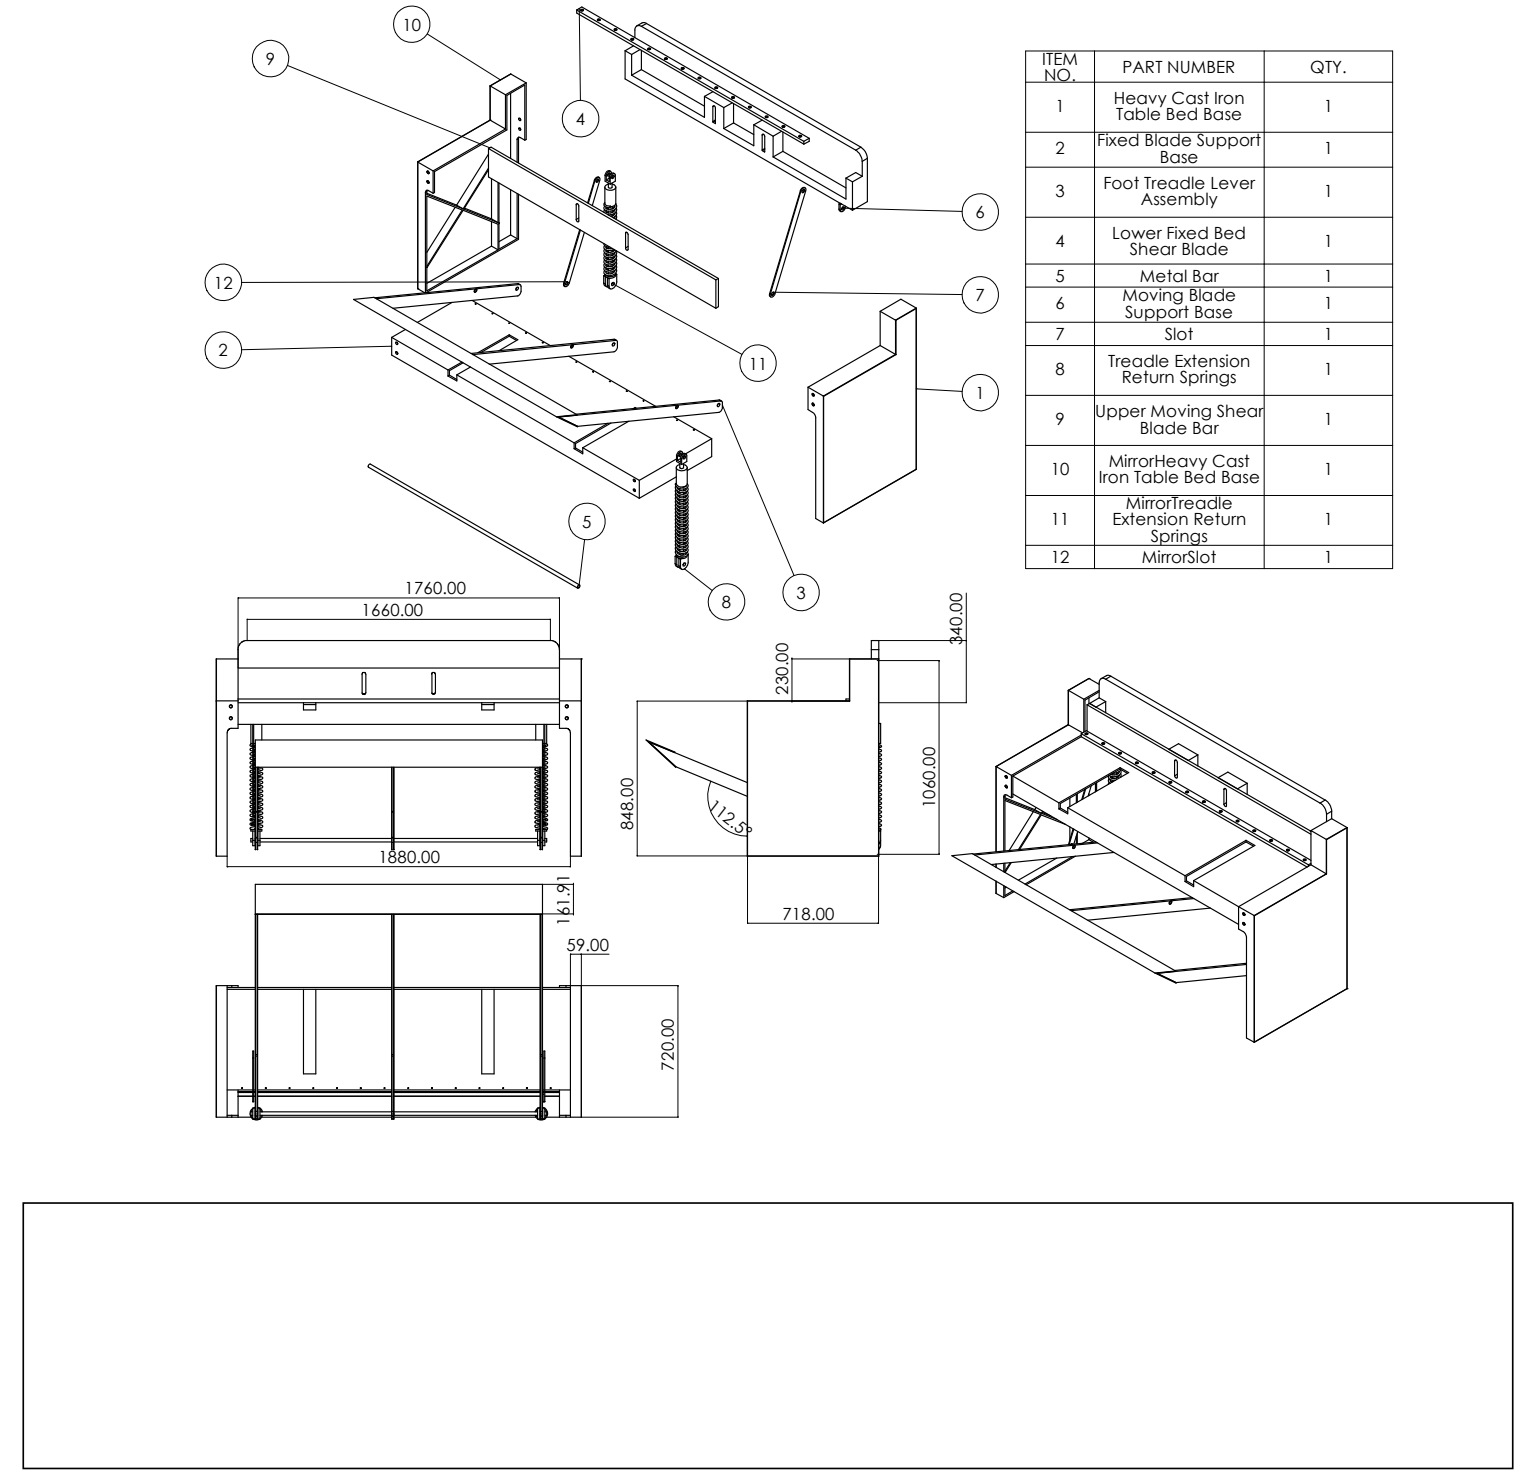
ISO-10303-21;
HEADER;
FILE_DESCRIPTION (('STEP AP214'),
    '1' );
FILE_NAME ('MAS-320',
    '2026-10-21T17:07:05',
    ( '' ),
    ( '' ),
    'SwSTEP 2.0',
    'SolidWorks 2025',
    '' );
FILE_SCHEMA (( 'AUTOMOTIVE_DESIGN' ));
ENDSEC;

DATA;
#1 = CARTESIAN_POINT ( 'NONE',  ( 745.1769319972822814, -41.80559628986934229, -346.2694204179732083 ) ) ;
#2 = CARTESIAN_POINT ( 'NONE',  ( 764.0069404352550464, -207.0783235625960685, -359.2566176426627180 ) ) ;
#3 = CARTESIAN_POINT ( 'NONE',  ( 745.1769319972822814, -209.8055962898687881, 346.2694204179732083 ) ) ;
#4 = CARTESIAN_POINT ( 'NONE',  ( 797.8594530101009923, -13.54369356751140963, 322.1405469898982119 ) ) ;
#5 =( BOUNDED_CURVE ( )  B_SPLINE_CURVE ( 2, ( #42977, #27813, #34735, #31272, #11342, #6564, #43210, #24332, #11582, #18730, #45142, #13500, #10036, #41910, #10254, #1170, #25872, #11803, #43435, #23072, #9239, #22634, #8789, #2069, #32818, #29794, #39983, #36732, #8332, #5090, #40437, #18964, #26092, #37170, #33058, #30023, #43655, #1395, #5529, #15499, #33484, #44108, #12472, #23310, #5303, #15279, #37412, #22395, #5769, #44335, #36499, #29579, #1830, #4863, #29365, #26551, #22857, #19625, #33720, #12025, #40649, #40206, #8568, #36950, #19181, #16161, #33266, #30243, #12690, #26770, #1612, #19399, #15711, #15939, #43874, #12253, #26333, #9002, #40875, #10150, #30713, #2768, #31156, #19857, #37866, #12929, #13166, #27016, #27245, #16861, #37632, #16626, #2991, #23530, #9913, #34150, #5983, #34634, #20075, #27462, #30941, #23985, #24225, #41115, #45034, #20540, #41337, #2520, #17078, #6462, #13390, #45254, #13613, #9467, #44568, #44809, #9687, #23751, #6212, #20305, #34397, #38106, #41560, #41801, #2288, #16387, #38333, #27697, #6679, #33937, #30466, #15422, #12398, #1747, #26925, #19779, #41028, #9388, #44026, #23223, #23455, #33195, #36878, #12841, #8717, #20002, #22552, #9151, #5912, #29712, #34079, #37554, #2216, #29500, #43572, #5445, #30169, #11940, #22783, #8482, #26008, #43789, #19319, #16085, #5228, #40579, #33403, #33863, #12618, #26252, #15629, #5690, #12171, #44260, #19540, #40117, #26477, #26696, #33635, #15854, #29942, #1532, #16310, #37328, #1988, #30392, #44485, #19108, #36657, #40365, #8925, #5017, #22995, #37090, #40793, #41950, #41259, #37788, #45414, #7068, #13775, #27854, #23906, #13537, #9837, #2443, #45176, #34552, #13999, #6822, #28067, #42163, #31078, #10291, #10514, #21149, #17466, #24367, #41720, #10074, #9615, #38471, #38706, #16781, #16545, #24589, #34998, #30630, #44725, #38254, #17221, #13088, #41483, #23677, #27171, #38027, #6137, #20227, #6382, #27611, #34315, #20901, #2684, #20678, #30861, #44955, #13312, #27388, #20463, #2911, #17001, #3131, #24145, #6600, #3375, #34768, #31548, #45650, #31306, #14912, #129, #7303, #25284, #14218, #22057, #14460, #39636, #15137, #18602, #39862, #7748, #17698, #21827, #3611, #28288, #42386, #10757, #25523, #11673, #10994, #31759, #24833, #4055, #29230, #32687, #35920, #38953, #25750, #43305, #11439, #28993, #21380, #32231, #8203, #35454, #4291, #35231, #3826, #25062, #1034, #28537, #17915, #39175, #7525, #810, #31985, #356, #42632, #21599, #35679, #18156, #591, #18382, #14693, #42848, #28769, #11215, #39397, #32462, #43074, #7991, #36147, #4509, #5627, #30330, #11887, #1692, #26638, #29661, #33579, #33143, #44424, #37267, #30115, #12115, #40065, #43737, #15796, #12561, #1930, #8664, #32923, #15579, #43521, #26859, #26196, #40311, #12778, #5175, #33808, #29886, #25959, #18831, #43973, #19052, #19721, #15367, #37036, #8426, #16253, #26424, #4729, #40734, #1268, #36823, #2162, #40968, #40524, #29448, #22271, #36367, #44203, #16033, #22495, #19261, #36606, #4960, #12348, #1479, #22726, #33350, #8875, #22939, #9090, #5388, #19482, #23158, #37501, #27335, #5861, #31026, #30804, #17168, #10234, #2854, #17407, #16481, #41428, #34247, #9779, #27554, #3076, #2380, #44662, #6543, #13939, #20623, #16947, #41658, #16720, #19950, #45124, #44897, #3310, #24083, #24313, #13482, #10013, #38197, #34717, #30561, #31253, #45591, #23620, #28014, #34943, #41890, #23399, #34025, #45354, #13715, #31489, #2620, #13023, #9330, #13257, #27113, #41203, #23846, #34494, #9560, #27793, #37729, #38418, #6081, #20168, #37958, #6317, #20845, #20399, #6769, #42797, #3555, #38648, #35867, #32175, #763, #32414, #42108, #21772, #7006, #14163, #538, #21093, #28940, #21320, #14864, #22007, #25464, #976, #14642, #24535, #28716, #10458, #35179, #17640, #31704, #43017, #18551, #17859, #71, #11382, #28234, #39119, #42329, #298, #10695, #31926, #3994, #24778, #35396, #39583, #38896, #39339, #7250, #3769, #7940, #14398, #11157, #25227, #28478, #32633, #42579, #18092, #18334, #10937, #25009, #36097, #4244, #7692, #4462, #15079, #7468, #21540, #35622, #32859, #18773, #4675, #11839, #29399, #22894, #25910, #9040, #11621, #25699, #5575, #40474, #4903, #40253, #36545, #29166, #26138, #15533, #40685, #33527, #23109, #37211, #12064, #36986, #19667, #2112, #19002, #39810, #40020, #29836, #36314, #8157, #5340, #19215, #1875, #19434, #43250, #8826, #22220, #22440, #1209, #33760, #33094, #1431, #15317, #8610, #12511, #43471, #15748, #8371, #43917, #29614, #43692, #22675, #36772, #15983, #5127, #33302, #12297, #30066, #26372, #44147, #26587, #45296, #34441, #12730, #41840, #38146, #9957, #23352, #13210, #13655, #31199, #41380, #9282, #23573, #30281, #41600, #13431, #38369, #37454, #23794, #6497, #6027, #33978, #20575, #37905, #37678, #24027, #17117, #9729, #24261, #5813, #2564, #41158, #16669, #2806, #16429, #34671, #12973, #10185, #44374, #26809, #6716, #27736, #20119, #40915, #6259, #34194, #20792, #30978, #34888, #20346, #16897, #16201, #2329, #45076, #19901, #30509, #30755, #44612, #9509, #27063, #44848, #27287, #39526, #31651, #27962, #45535, #21263, #38836, #42277, #17805, #32114, #25404, #10880, #31872, #24948, #19, #7189, #3939, #35342, #28417, #10637, #21712, #7881, #38590, #42515, #7635, #24718, #14584, #14111, #3251, #21957, #42058, #17343, #14805, #13888, #28184, #18033, #10406, #24483, #42736, #39063, #35809, #39280, #3718, #3493, #6945, #21028, #7411, #35116, #4185, #243, #18280, #28879, #32354, #31429, #21486, #17581, #35563, #14339, #479, #28658, #11100, #708, #25170, #42959, #11327, #5288, #36043, #33043, #43193, #39969, #11562, #25859, #43639, #22167, #29348, #40421, #36257, #33249, #1154, #4614, #26315, #18711, #4406, #1595, #15693, #12456, #29109, #12008, #12236, #8314, #8106, #8773, #29777, #22614, #22841, #36934, #39758, #15021, #32800, #15259, #25644, #43421, #8550, #11788, #43853, #22379, #15920, #18496, #32575, #26535, #19381, #36483, #1381, #4848, #918, #15484, #18947, #30004, #33466, #44091, #40633, #29564, #36714, #8986, #26072, #40185, #5074, #19165, #27679, #30228, #16845, #13596, #37396, #41784, #2973, #9895, #37153, #5512, #13149, #37848, #45236, #16371, #5968, #30698, #5750, #26999, #23738, #12911, #2504, #30448, #41543, #23054, #41322, #17062, #23968, #19608, #33701, #27230, #6197, #2051, #44551, #16145, #44794, #19839, #41095, #20288, #9450, #16610, #23514, #38090, #44319, #9672, #12674, #26754, #40858, #9220, #34618, #23295, #33921, #34381, #2272, #37615, #20058, #2750, #13373, #30924, #34135, #45020, #27446, #6445, #20524, #31139, #42687, #35062, #14529, #35753, #39233, #14755, #28354, #38317, #42458, #24207, #3194, #24897, #31372, #4132, #14285, #45710, #31822, #25119, #10134, #7134, #17283, #14062, #45480, #28134, #17758, #42010, #3436, #28605, #10354, #7362, #7586, #35293 ),
 .UNSPECIFIED., .F., .T. ) 
 B_SPLINE_CURVE_WITH_KNOTS ( ( 3, 2, 2, 2, 2, 2, 2, 2, 2, 2, 2, 2, 2, 2, 2, 2, 2, 2, 2, 2, 2, 2, 2, 2, 2, 2, 2, 2, 2, 2, 2, 2, 2, 2, 2, 2, 2, 2, 2, 2, 2, 2, 2, 2, 2, 2, 2, 2, 2, 2, 2, 2, 2, 2, 2, 2, 2, 2, 2, 2, 2, 2, 2, 2, 2, 2, 2, 2, 2, 2, 2, 2, 2, 2, 2, 2, 2, 2, 2, 2, 2, 2, 2, 2, 2, 2, 2, 2, 2, 2, 2, 2, 2, 2, 2, 2, 2, 2, 2, 2, 2, 2, 2, 2, 2, 2, 2, 2, 2, 2, 2, 2, 2, 2, 2, 2, 2, 2, 2, 2, 2, 2, 2, 2, 2, 2, 2, 2, 2, 2, 2, 2, 2, 2, 2, 2, 2, 2, 2, 2, 2, 2, 2, 2, 2, 2, 2, 2, 2, 2, 2, 2, 2, 2, 2, 2, 2, 2, 2, 2, 2, 2, 2, 2, 2, 2, 2, 2, 2, 2, 2, 2, 2, 2, 2, 2, 2, 2, 2, 2, 2, 2, 2, 2, 2, 2, 2, 2, 2, 2, 2, 2, 2, 2, 2, 2, 2, 2, 2, 2, 2, 2, 2, 2, 2, 2, 2, 2, 2, 2, 2, 2, 2, 2, 2, 2, 2, 2, 2, 2, 2, 2, 2, 2, 2, 2, 2, 2, 2, 2, 2, 2, 2, 2, 2, 2, 2, 2, 2, 2, 2, 2, 2, 2, 2, 2, 2, 2, 2, 2, 2, 2, 2, 2, 2, 2, 2, 2, 2, 2, 2, 2, 2, 2, 2, 2, 2, 2, 2, 2, 2, 2, 2, 2, 2, 2, 2, 2, 2, 2, 2, 2, 2, 2, 2, 2, 2, 2, 2, 2, 2, 2, 2, 2, 2, 2, 2, 2, 2, 2, 2, 2, 2, 2, 2, 2, 2, 2, 2, 2, 2, 2, 2, 2, 2, 2, 2, 2, 2, 2, 2, 2, 2, 2, 2, 2, 2, 2, 2, 2, 2, 2, 2, 2, 2, 2, 2, 2, 2, 2, 2, 2, 2, 2, 2, 2, 2, 2, 2, 2, 2, 2, 2, 2, 2, 2, 2, 2, 2, 2, 2, 2, 2, 2, 2, 2, 2, 2, 2, 2, 2, 2, 2, 2, 2, 2, 2, 2, 2, 2, 2, 2, 2, 2, 2, 2, 2, 2, 2, 2, 2, 2, 2, 2, 2, 2, 2, 2, 2, 2, 2, 2, 2, 2, 2, 2, 2, 2, 2, 2, 2, 2, 2, 2, 2, 2, 2, 2, 2, 2, 2, 2, 2, 2, 2, 2, 2, 2, 2, 2, 2, 3 ),
 ( 0.000000000000000000, 0.002272727272727272617, 0.004545454545454545234, 0.006818181818181817851, 0.009090909090909090468, 0.01136363636363636395, 0.01363636363636363570, 0.01590909090909090745, 0.01818181818181818094, 0.02045454545454545442, 0.02272727272727272790, 0.02500000000000000139, 0.02727272727272727140, 0.02954545454545454489, 0.03181818181818181490, 0.03409090909090908839, 0.03636363636363636187, 0.03863636363636363535, 0.04090909090909090884, 0.04318181818181818232, 0.04545454545454545581, 0.04772727272727272929, 0.05000000000000000278, 0.05227272727272727626, 0.05454545454545454281, 0.05681818181818181629, 0.05909090909090908977, 0.06136363636363636326, 0.06363636363636362980, 0.06590909090909090329, 0.06818181818181817677, 0.07045454545454545026, 0.07272727272727272374, 0.07499999999999999722, 0.07727272727272727071, 0.07954545454545454419, 0.08181818181818181768, 0.08409090909090909116, 0.08636363636363636465, 0.08863636363636363813, 0.09090909090909091161, 0.09318181818181818510, 0.09545454545454545858, 0.09772727272727273207, 0.1000000000000000056, 0.1022727272727272790, 0.1045454545454545525, 0.1068181818181818121, 0.1090909090909090856, 0.1113636363636363591, 0.1136363636363636326, 0.1159090909090909061, 0.1181818181818181795, 0.1204545454545454530, 0.1227272727272727265, 0.1250000000000000000, 0.1272727272727272596, 0.1295454545454545470, 0.1318181818181818066, 0.1340909090909090939, 0.1363636363636363535, 0.1386363636363636409, 0.1409090909090909005, 0.1431818181818181879, 0.1454545454545454475, 0.1477272727272727348, 0.1499999999999999944, 0.1522727272727272818, 0.1545454545454545414, 0.1568181818181818288, 0.1590909090909090884, 0.1613636363636363757, 0.1636363636363636354, 0.1659090909090909227, 0.1681818181818181823, 0.1704545454545454419, 0.1727272727272727293, 0.1749999999999999889, 0.1772727272727272763, 0.1795454545454545359, 0.1818181818181818232, 0.1840909090909090828, 0.1863636363636363702, 0.1886363636363636298, 0.1909090909090909172, 0.1931818181818181768, 0.1954545454545454641, 0.1977272727272727237, 0.2000000000000000111, 0.2022727272727272707, 0.2045454545454545581, 0.2068181818181818177, 0.2090909090909091050, 0.2113636363636363646, 0.2136363636363636243, 0.2159090909090909116, 0.2181818181818181712, 0.2204545454545454586, 0.2227272727272727182, 0.2250000000000000056, 0.2272727272727272652, 0.2295454545454545525, 0.2318181818181818121, 0.2340909090909090995, 0.2363636363636363591, 0.2386363636363636465, 0.2409090909090909061, 0.2431818181818181934, 0.2454545454545454530, 0.2477272727272727404, 0.2500000000000000000, 0.2522727272727272596, 0.2545454545454545192, 0.2568181818181818343, 0.2590909090909090939, 0.2613636363636363535, 0.2636363636363636131, 0.2659090909090909283, 0.2681818181818181879, 0.2704545454545454475, 0.2727272727272727071, 0.2750000000000000222, 0.2772727272727272818, 0.2795454545454545414, 0.2818181818181818010, 0.2840909090909091161, 0.2863636363636363757, 0.2886363636363636354, 0.2909090909090908950, 0.2931818181818181546, 0.2954545454545454697, 0.2977272727272727293, 0.2999999999999999889, 0.3022727272727272485, 0.3045454545454545636, 0.3068181818181818232, 0.3090909090909090828, 0.3113636363636363424, 0.3136363636363636576, 0.3159090909090909172, 0.3181818181818181768, 0.3204545454545454364, 0.3227272727272727515, 0.3250000000000000111, 0.3272727272727272707, 0.3295454545454545303, 0.3318181818181818454, 0.3340909090909090495, 0.3363636363636363646, 0.3386363636363636243, 0.3409090909090908839, 0.3431818181818181990, 0.3454545454545454586, 0.3477272727272727182, 0.3499999999999999778, 0.3522727272727272929, 0.3545454545454545525, 0.3568181818181818121, 0.3590909090909090717, 0.3613636363636363869, 0.3636363636363636465, 0.3659090909090909061, 0.3681818181818181657, 0.3704545454545454808, 0.3727272727272727404, 0.3750000000000000000, 0.3772727272727272596, 0.3795454545454545192, 0.3818181818181818343, 0.3840909090909090939, 0.3863636363636363535, 0.3886363636363636131, 0.3909090909090909283, 0.3931818181818181879, 0.3954545454545454475, 0.3977272727272727071, 0.4000000000000000222, 0.4022727272727272818, 0.4045454545454545414, 0.4068181818181818010, 0.4090909090909091161, 0.4113636363636363757, 0.4136363636363636354, 0.4159090909090908950, 0.4181818181818182101, 0.4204545454545454697, 0.4227272727272727293, 0.4249999999999999889, 0.4272727272727272485, 0.4295454545454545636, 0.4318181818181818232, 0.4340909090909090828, 0.4363636363636363424, 0.4386363636363636576, 0.4409090909090909172, 0.4431818181818181768, 0.4454545454545454364, 0.4477272727272727515, 0.4500000000000000111, 0.4522727272727272707, 0.4545454545454545303, 0.4568181818181818454, 0.4590909090909091050, 0.4613636363636363646, 0.4636363636363636243, 0.4659090909090908839, 0.4681818181818181990, 0.4704545454545454586, 0.4727272727272727182, 0.4749999999999999778, 0.4772727272727272929, 0.4795454545454545525, 0.4818181818181818121, 0.4840909090909090717, 0.4863636363636363869, 0.4886363636363636465, 0.4909090909090909061, 0.4931818181818181657, 0.4954545454545454808, 0.4977272727272727959, 0.5000000000000000000, 0.5022727272727273151, 0.5045454545454545192, 0.5068181818181818343, 0.5090909090909090384, 0.5113636363636363535, 0.5136363636363636687, 0.5159090909090908728, 0.5181818181818181879, 0.5204545454545455030, 0.5227272727272727071, 0.5250000000000000222, 0.5272727272727272263, 0.5295454545454545414, 0.5318181818181818565, 0.5340909090909090606, 0.5363636363636363757, 0.5386363636363636909, 0.5409090909090908950, 0.5431818181818182101, 0.5454545454545454142, 0.5477272727272727293, 0.5500000000000000444, 0.5522727272727272485, 0.5545454545454545636, 0.5568181818181817677, 0.5590909090909090828, 0.5613636363636363980, 0.5636363636363636020, 0.5659090909090909172, 0.5681818181818182323, 0.5704545454545454364, 0.5727272727272727515, 0.5749999999999999556, 0.5772727272727272707, 0.5795454545454545858, 0.5818181818181817899, 0.5840909090909089940, 0.5863636363636363091, 0.5886363636363636243, 0.5909090909090909394, 0.5931818181818181435, 0.5954545454545454586, 0.5977272727272727737, 0.5999999999999999778, 0.6022727272727272929, 0.6045454545454544970, 0.6068181818181818121, 0.6090909090909091272, 0.6113636363636363313, 0.6136363636363636465, 0.6159090909090909616, 0.6181818181818181657, 0.6204545454545454808, 0.6227272727272726849, 0.6250000000000000000, 0.6272727272727273151, 0.6295454545454545192, 0.6318181818181818343, 0.6340909090909090384, 0.6363636363636363535, 0.6386363636363636687, 0.6409090909090908728, 0.6431818181818181879, 0.6454545454545455030, 0.6477272727272727071, 0.6500000000000000222, 0.6522727272727272263, 0.6545454545454545414, 0.6568181818181818565, 0.6590909090909090606, 0.6613636363636363757, 0.6636363636363636909, 0.6659090909090908950, 0.6681818181818180991, 0.6704545454545454142, 0.6727272727272727293, 0.6750000000000000444, 0.6772727272727272485, 0.6795454545454545636, 0.6818181818181817677, 0.6840909090909090828, 0.6863636363636363980, 0.6886363636363636020, 0.6909090909090909172, 0.6931818181818182323, 0.6954545454545454364, 0.6977272727272727515, 0.6999999999999999556, 0.7022727272727272707, 0.7045454545454545858, 0.7068181818181817899, 0.7090909090909091050, 0.7113636363636363091, 0.7136363636363636243, 0.7159090909090909394, 0.7181818181818181435, 0.7204545454545454586, 0.7227272727272727737, 0.7249999999999999778, 0.7272727272727272929, 0.7295454545454544970, 0.7318181818181818121, 0.7340909090909091272, 0.7363636363636363313, 0.7386363636363636465, 0.7409090909090909616, 0.7431818181818181657, 0.7454545454545454808, 0.7477272727272726849, 0.7500000000000000000, 0.7522727272727273151, 0.7545454545454545192, 0.7568181818181818343, 0.7590909090909090384, 0.7613636363636363535, 0.7636363636363636687, 0.7659090909090908728, 0.7681818181818181879, 0.7704545454545455030, 0.7727272727272727071, 0.7750000000000000222, 0.7772727272727272263, 0.7795454545454545414, 0.7818181818181818565, 0.7840909090909090606, 0.7863636363636363757, 0.7886363636363636909, 0.7909090909090908950, 0.7931818181818182101, 0.7954545454545454142, 0.7977272727272727293, 0.8000000000000000444, 0.8022727272727272485, 0.8045454545454545636, 0.8068181818181817677, 0.8090909090909090828, 0.8113636363636363980, 0.8136363636363636020, 0.8159090909090909172, 0.8181818181818182323, 0.8204545454545454364, 0.8227272727272727515, 0.8249999999999999556, 0.8272727272727272707, 0.8295454545454545858, 0.8318181818181817899, 0.8340909090909091050, 0.8363636363636364202, 0.8386363636363636243, 0.8409090909090909394, 0.8431818181818181435, 0.8454545454545454586, 0.8477272727272727737, 0.8499999999999999778, 0.8522727272727272929, 0.8545454545454544970, 0.8568181818181818121, 0.8590909090909091272, 0.8613636363636363313, 0.8636363636363636465, 0.8659090909090909616, 0.8681818181818181657, 0.8704545454545454808, 0.8727272727272726849, 0.8750000000000000000, 0.8772727272727273151, 0.8795454545454545192, 0.8818181818181818343, 0.8840909090909090384, 0.8863636363636363535, 0.8886363636363636687, 0.8909090909090908728, 0.8931818181818181879, 0.8954545454545455030, 0.8977272727272727071, 0.9000000000000000222, 0.9022727272727272263, 0.9045454545454545414, 0.9068181818181818565, 0.9090909090909090606, 0.9113636363636363757, 0.9136363636363636909, 0.9159090909090908950, 0.9181818181818182101, 0.9204545454545453032, 0.9227272727272727293, 0.9250000000000000444, 0.9272727272727272485, 0.9295454545454545636, 0.9318181818181817677, 0.9340909090909090828, 0.9363636363636363980, 0.9386363636363636020, 0.9409090909090909172, 0.9431818181818182323, 0.9454545454545454364, 0.9477272727272727515, 0.9499999999999999556, 0.9522727272727272707, 0.9545454545454545858, 0.9568181818181817899, 0.9590909090909091050, 0.9613636363636363091, 0.9636363636363636243, 0.9659090909090909394, 0.9681818181818181435, 0.9704545454545454586, 0.9727272727272727737, 0.9749999999999999778, 0.9772727272727272929, 0.9779695260516495514 ),
 .UNSPECIFIED. ) 
 CURVE ( )  GEOMETRIC_REPRESENTATION_ITEM ( )  RATIONAL_B_SPLINE_CURVE ( ( 1.000000000000000000, 0.9898214418809326842, 1.000000000000000000, 0.9898214418809326842, 1.000000000000000000, 0.9898214418809326842, 1.000000000000000000, 0.9898214418809326842, 1.000000000000000000, 0.9898214418809326842, 1.000000000000000000, 0.9898214418809326842, 1.000000000000000000, 0.9898214418809326842, 1.000000000000000000, 0.9898214418809326842, 1.000000000000000000, 0.9898214418809326842, 1.000000000000000000, 0.9898214418809326842, 1.000000000000000000, 0.9898214418809326842, 1.000000000000000000, 0.9898214418809326842, 1.000000000000000000, 0.9898214418809326842, 1.000000000000000000, 0.9898214418809326842, 1.000000000000000000, 0.9898214418809326842, 1.000000000000000000, 0.9898214418809326842, 1.000000000000000000, 0.9898214418809326842, 1.000000000000000000, 0.9898214418809326842, 1.000000000000000000, 0.9898214418809326842, 1.000000000000000000, 0.9898214418809326842, 1.000000000000000000, 0.9898214418809326842, 1.000000000000000000, 0.9898214418809326842, 1.000000000000000000, 0.9898214418809326842, 1.000000000000000000, 0.9898214418809326842, 1.000000000000000000, 0.9898214418809326842, 1.000000000000000000, 0.9898214418809326842, 1.000000000000000000, 0.9898214418809326842, 1.000000000000000000, 0.9898214418809326842, 1.000000000000000000, 0.9898214418809326842, 1.000000000000000000, 0.9898214418809326842, 1.000000000000000000, 0.9898214418809326842, 1.000000000000000000, 0.9898214418809326842, 1.000000000000000000, 0.9898214418809326842, 1.000000000000000000, 0.9898214418809326842, 1.000000000000000000, 0.9898214418809326842, 1.000000000000000000, 0.9898214418809326842, 1.000000000000000000, 0.9898214418809326842, 1.000000000000000000, 0.9898214418809326842, 1.000000000000000000, 0.9898214418809326842, 1.000000000000000000, 0.9898214418809326842, 1.000000000000000000, 0.9898214418809326842, 1.000000000000000000, 0.9898214418809326842, 1.000000000000000000, 0.9898214418809326842, 1.000000000000000000, 0.9898214418809326842, 1.000000000000000000, 0.9898214418809326842, 1.000000000000000000, 0.9898214418809326842, 1.000000000000000000, 0.9898214418809326842, 1.000000000000000000, 0.9898214418809326842, 1.000000000000000000, 0.9898214418809326842, 1.000000000000000000, 0.9898214418809326842, 1.000000000000000000, 0.9898214418809326842, 1.000000000000000000, 0.9898214418809326842, 1.000000000000000000, 0.9898214418809326842, 1.000000000000000000, 0.9898214418809326842, 1.000000000000000000, 0.9898214418809326842, 1.000000000000000000, 0.9898214418809326842, 1.000000000000000000, 0.9898214418809326842, 1.000000000000000000, 0.9898214418809326842, 1.000000000000000000, 0.9898214418809326842, 1.000000000000000000, 0.9898214418809326842, 1.000000000000000000, 0.9898214418809326842, 1.000000000000000000, 0.9898214418809326842, 1.000000000000000000, 0.9898214418809326842, 1.000000000000000000, 0.9898214418809326842, 1.000000000000000000, 0.9898214418809326842, 1.000000000000000000, 0.9898214418809326842, 1.000000000000000000, 0.9898214418809326842, 1.000000000000000000, 0.9898214418809326842, 1.000000000000000000, 0.9898214418809326842, 1.000000000000000000, 0.9898214418809326842, 1.000000000000000000, 0.9898214418809326842, 1.000000000000000000, 0.9898214418809326842, 1.000000000000000000, 0.9898214418809326842, 1.000000000000000000, 0.9898214418809326842, 1.000000000000000000, 0.9898214418809326842, 1.000000000000000000, 0.9898214418809326842, 1.000000000000000000, 0.9898214418809326842, 1.000000000000000000, 0.9898214418809326842, 1.000000000000000000, 0.9898214418809326842, 1.000000000000000000, 0.9898214418809326842, 1.000000000000000000, 0.9898214418809326842, 1.000000000000000000, 0.9898214418809326842, 1.000000000000000000, 0.9898214418809326842, 1.000000000000000000, 0.9898214418809326842, 1.000000000000000000, 0.9898214418809326842, 1.000000000000000000, 0.9898214418809326842, 1.000000000000000000, 0.9898214418809326842, 1.000000000000000000, 0.9898214418809326842, 1.000000000000000000, 0.9898214418809326842, 1.000000000000000000, 0.9898214418809326842, 1.000000000000000000, 0.9898214418809326842, 1.000000000000000000, 0.9898214418809326842, 1.000000000000000000, 0.9898214418809326842, 1.000000000000000000, 0.9898214418809326842, 1.000000000000000000, 0.9898214418809326842, 1.000000000000000000, 0.9898214418809326842, 1.000000000000000000, 0.9898214418809326842, 1.000000000000000000, 0.9898214418809326842, 1.000000000000000000, 0.9898214418809326842, 1.000000000000000000, 0.9898214418809326842, 1.000000000000000000, 0.9898214418809326842, 1.000000000000000000, 0.9898214418809326842, 1.000000000000000000, 0.9898214418809326842, 1.000000000000000000, 0.9898214418809326842, 1.000000000000000000, 0.9898214418809326842, 1.000000000000000000, 0.9898214418809326842, 1.000000000000000000, 0.9898214418809326842, 1.000000000000000000, 0.9898214418809326842, 1.000000000000000000, 0.9898214418809326842, 1.000000000000000000, 0.9898214418809326842, 1.000000000000000000, 0.9898214418809326842, 1.000000000000000000, 0.9898214418809326842, 1.000000000000000000, 0.9898214418809326842, 1.000000000000000000, 0.9898214418809326842, 1.000000000000000000, 0.9898214418809326842, 1.000000000000000000, 0.9898214418809326842, 1.000000000000000000, 0.9898214418809326842, 1.000000000000000000, 0.9898214418809326842, 1.000000000000000000, 0.9898214418809326842, 1.000000000000000000, 0.9898214418809326842, 1.000000000000000000, 0.9898214418809326842, 1.000000000000000000, 0.9898214418809326842, 1.000000000000000000, 0.9898214418809326842, 1.000000000000000000, 0.9898214418809326842, 1.000000000000000000, 0.9898214418809326842, 1.000000000000000000, 0.9898214418809326842, 1.000000000000000000, 0.9898214418809326842, 1.000000000000000000, 0.9898214418809326842, 1.000000000000000000, 0.9898214418809326842, 1.000000000000000000, 0.9898214418809326842, 1.000000000000000000, 0.9898214418809326842, 1.000000000000000000, 0.9898214418809326842, 1.000000000000000000, 0.9898214418809326842, 1.000000000000000000, 0.9898214418809326842, 1.000000000000000000, 0.9898214418809326842, 1.000000000000000000, 0.9898214418809326842, 1.000000000000000000, 0.9898214418809326842, 1.000000000000000000, 0.9898214418809326842, 1.000000000000000000, 0.9898214418809326842, 1.000000000000000000, 0.9898214418809326842, 1.000000000000000000, 0.9898214418809326842, 1.000000000000000000, 0.9898214418809326842, 1.000000000000000000, 0.9898214418809326842, 1.000000000000000000, 0.9898214418809326842, 1.000000000000000000, 0.9898214418809326842, 1.000000000000000000, 0.9898214418809326842, 1.000000000000000000, 0.9898214418809326842, 1.000000000000000000, 0.9898214418809326842, 1.000000000000000000, 0.9898214418809326842, 1.000000000000000000, 0.9898214418809326842, 1.000000000000000000, 0.9898214418809326842, 1.000000000000000000, 0.9898214418809326842, 1.000000000000000000, 0.9898214418809326842, 1.000000000000000000, 0.9898214418809326842, 1.000000000000000000, 0.9898214418809326842, 1.000000000000000000, 0.9898214418809326842, 1.000000000000000000, 0.9898214418809326842, 1.000000000000000000, 0.9898214418809326842, 1.000000000000000000, 0.9898214418809326842, 1.000000000000000000, 0.9898214418809326842, 1.000000000000000000, 0.9898214418809326842, 1.000000000000000000, 0.9898214418809326842, 1.000000000000000000, 0.9898214418809326842, 1.000000000000000000, 0.9898214418809326842, 1.000000000000000000, 0.9898214418809326842, 1.000000000000000000, 0.9898214418809326842, 1.000000000000000000, 0.9898214418809326842, 1.000000000000000000, 0.9898214418809326842, 1.000000000000000000, 0.9898214418809326842, 1.000000000000000000, 0.9898214418809326842, 1.000000000000000000, 0.9898214418809326842, 1.000000000000000000, 0.9898214418809326842, 1.000000000000000000, 0.9898214418809326842, 1.000000000000000000, 0.9898214418809326842, 1.000000000000000000, 0.9898214418809326842, 1.000000000000000000, 0.9898214418809326842, 1.000000000000000000, 0.9898214418809326842, 1.000000000000000000, 0.9898214418809326842, 1.000000000000000000, 0.9898214418809326842, 1.000000000000000000, 0.9898214418809326842, 1.000000000000000000, 0.9898214418809326842, 1.000000000000000000, 0.9898214418809326842, 1.000000000000000000, 0.9898214418809326842, 1.000000000000000000, 0.9898214418809326842, 1.000000000000000000, 0.9898214418809326842, 1.000000000000000000, 0.9898214418809326842, 1.000000000000000000, 0.9898214418809326842, 1.000000000000000000, 0.9898214418809326842, 1.000000000000000000, 0.9898214418809326842, 1.000000000000000000, 0.9898214418809326842, 1.000000000000000000, 0.9898214418809326842, 1.000000000000000000, 0.9898214418809326842, 1.000000000000000000, 0.9898214418809326842, 1.000000000000000000, 0.9898214418809326842, 1.000000000000000000, 0.9898214418809326842, 1.000000000000000000, 0.9898214418809326842, 1.000000000000000000, 0.9898214418809326842, 1.000000000000000000, 0.9898214418809326842, 1.000000000000000000, 0.9898214418809326842, 1.000000000000000000, 0.9898214418809326842, 1.000000000000000000, 0.9898214418809326842, 1.000000000000000000, 0.9898214418809326842, 1.000000000000000000, 0.9898214418809326842, 1.000000000000000000, 0.9898214418809326842, 1.000000000000000000, 0.9898214418809326842, 1.000000000000000000, 0.9898214418809326842, 1.000000000000000000, 0.9898214418809326842, 1.000000000000000000, 0.9898214418809326842, 1.000000000000000000, 0.9898214418809326842, 1.000000000000000000, 0.9898214418809326842, 1.000000000000000000, 0.9898214418809326842, 1.000000000000000000, 0.9898214418809326842, 1.000000000000000000, 0.9898214418809326842, 1.000000000000000000, 0.9898214418809326842, 1.000000000000000000, 0.9898214418809326842, 1.000000000000000000, 0.9898214418809326842, 1.000000000000000000, 0.9898214418809326842, 1.000000000000000000, 0.9898214418809326842, 1.000000000000000000, 0.9898214418809326842, 1.000000000000000000, 0.9898214418809326842, 1.000000000000000000, 0.9898214418809326842, 1.000000000000000000, 0.9898214418809326842, 1.000000000000000000, 0.9898214418809326842, 1.000000000000000000, 0.9898214418809326842, 1.000000000000000000, 0.9898214418809326842, 1.000000000000000000, 0.9898214418809326842, 1.000000000000000000, 0.9898214418809326842, 1.000000000000000000, 0.9898214418809326842, 1.000000000000000000, 0.9898214418809326842, 1.000000000000000000, 0.9898214418809326842, 1.000000000000000000, 0.9898214418809326842, 1.000000000000000000, 0.9898214418809326842, 1.000000000000000000, 0.9898214418809326842, 1.000000000000000000, 0.9898214418809326842, 1.000000000000000000, 0.9898214418809326842, 1.000000000000000000, 0.9898214418809326842, 1.000000000000000000, 0.9898214418809326842, 1.000000000000000000, 0.9898214418809326842, 1.000000000000000000, 0.9898214418809326842, 1.000000000000000000, 0.9898214418809326842, 1.000000000000000000, 0.9898214418809326842, 1.000000000000000000, 0.9898214418809326842, 1.000000000000000000, 0.9898214418809326842, 1.000000000000000000, 0.9898214418809326842, 1.000000000000000000, 0.9898214418809326842, 1.000000000000000000, 0.9898214418809326842, 1.000000000000000000, 0.9898214418809326842, 1.000000000000000000, 0.9898214418809326842, 1.000000000000000000, 0.9898214418809326842, 1.000000000000000000, 0.9898214418809326842, 1.000000000000000000, 0.9898214418809326842, 1.000000000000000000, 0.9898214418809326842, 1.000000000000000000, 0.9898214418809326842, 1.000000000000000000, 0.9898214418809326842, 1.000000000000000000, 0.9898214418809326842, 1.000000000000000000, 0.9898214418809326842, 1.000000000000000000, 0.9898214418809326842, 1.000000000000000000, 0.9898214418809326842, 1.000000000000000000, 0.9898214418809326842, 1.000000000000000000, 0.9898214418809326842, 1.000000000000000000, 0.9898214418809326842, 1.000000000000000000, 0.9898214418809326842, 1.000000000000000000, 0.9898214418809326842, 1.000000000000000000, 0.9898214418809326842, 1.000000000000000000, 0.9898214418809326842, 1.000000000000000000, 0.9898214418809326842, 1.000000000000000000, 0.9898214418809326842, 1.000000000000000000, 0.9898214418809326842, 1.000000000000000000, 0.9898214418809326842, 1.000000000000000000, 0.9898214418809326842, 1.000000000000000000, 0.9898214418809326842, 1.000000000000000000, 0.9898214418809326842, 1.000000000000000000, 0.9898214418809326842, 1.000000000000000000, 0.9898214418809326842, 1.000000000000000000, 0.9898214418809326842, 1.000000000000000000, 0.9898214418809326842, 1.000000000000000000, 0.9898214418809326842, 1.000000000000000000, 0.9898214418809326842, 1.000000000000000000, 0.9898214418809326842, 1.000000000000000000, 0.9898214418809326842, 1.000000000000000000, 0.9898214418809326842, 1.000000000000000000, 0.9898214418809326842, 1.000000000000000000, 0.9898214418809326842, 1.000000000000000000, 0.9898214418809326842, 1.000000000000000000, 0.9898214418809326842, 1.000000000000000000, 0.9898214418809326842, 1.000000000000000000, 0.9898214418809326842, 1.000000000000000000, 0.9898214418809326842, 1.000000000000000000, 0.9898214418809326842, 1.000000000000000000, 0.9898214418809326842, 1.000000000000000000, 0.9898214418809326842, 1.000000000000000000, 0.9898214418809326842, 1.000000000000000000, 0.9898214418809326842, 1.000000000000000000, 0.9898214418809326842, 1.000000000000000000, 0.9898214418809326842, 1.000000000000000000, 0.9898214418809326842, 1.000000000000000000, 0.9898214418809326842, 1.000000000000000000, 0.9898214418809326842, 1.000000000000000000, 0.9898214418809326842, 1.000000000000000000, 0.9898214418809326842, 1.000000000000000000, 0.9898214418809326842, 1.000000000000000000, 0.9898214418809326842, 1.000000000000000000, 0.9898214418809326842, 1.000000000000000000, 0.9898214418809326842, 1.000000000000000000, 0.9898214418809326842, 1.000000000000000000, 0.9898214418809326842, 1.000000000000000000, 0.9898214418809326842, 1.000000000000000000, 0.9898214418809326842, 1.000000000000000000, 0.9898214418809326842, 1.000000000000000000, 0.9898214418809326842, 1.000000000000000000, 0.9898214418809326842, 1.000000000000000000, 0.9898214418809326842, 1.000000000000000000, 0.9898214418809326842, 1.000000000000000000, 0.9898214418809326842, 1.000000000000000000, 0.9898214418809326842, 1.000000000000000000, 0.9898214418809326842, 1.000000000000000000, 0.9898214418809326842, 1.000000000000000000, 0.9898214418809326842, 1.000000000000000000, 0.9898214418809326842, 1.000000000000000000, 0.9898214418809326842, 1.000000000000000000, 0.9898214418809326842, 1.000000000000000000, 0.9898214418809326842, 1.000000000000000000, 0.9898214418809326842, 1.000000000000000000, 0.9898214418809326842, 1.000000000000000000, 0.9898214418809326842, 1.000000000000000000, 0.9898214418809326842, 1.000000000000000000, 0.9898214418809326842, 1.000000000000000000, 0.9898214418809326842, 1.000000000000000000, 0.9898214418809326842, 1.000000000000000000, 0.9898214418809326842, 1.000000000000000000, 0.9898214418809326842, 1.000000000000000000, 0.9898214418809326842, 1.000000000000000000, 0.9898214418809326842, 1.000000000000000000, 0.9898214418809326842, 1.000000000000000000, 0.9898214418809326842, 1.000000000000000000, 0.9898214418809326842, 1.000000000000000000, 0.9898214418809326842, 1.000000000000000000, 0.9898214418809326842, 1.000000000000000000, 0.9898214418809326842, 1.000000000000000000, 0.9898214418809326842, 1.000000000000000000, 0.9898214418809326842, 1.000000000000000000, 0.9898214418809326842, 1.000000000000000000, 0.9898214418809326842, 1.000000000000000000, 0.9898214418809326842, 1.000000000000000000, 0.9898214418809326842, 1.000000000000000000, 0.9898214418809326842, 1.000000000000000000, 0.9898214418809326842, 1.000000000000000000, 0.9898214418809326842, 1.000000000000000000, 0.9898214418809326842, 1.000000000000000000, 0.9898214418809326842, 1.000000000000000000, 0.9898214418809326842, 1.000000000000000000, 0.9898214418809326842, 1.000000000000000000, 0.9898214418809326842, 1.000000000000000000, 0.9898214418809326842, 1.000000000000000000, 0.9898214418809326842, 1.000000000000000000, 0.9898214418809326842, 1.000000000000000000, 0.9898214418809326842, 1.000000000000000000, 0.9898214418809326842, 1.000000000000000000, 0.9898214418809326842, 1.000000000000000000, 0.9898214418809326842, 1.000000000000000000, 0.9898214418809326842, 1.000000000000000000, 0.9898214418809326842, 1.000000000000000000, 0.9898214418809326842, 1.000000000000000000, 0.9898214418809326842, 1.000000000000000000, 0.9898214418809326842, 1.000000000000000000, 0.9898214418809326842, 1.000000000000000000, 0.9898214418809326842, 1.000000000000000000, 0.9898214418809326842, 1.000000000000000000, 0.9898214418809326842, 1.000000000000000000, 0.9898214418809326842, 1.000000000000000000, 0.9898214418809326842, 1.000000000000000000, 0.9898214418809326842, 1.000000000000000000, 0.9898214418809326842, 1.000000000000000000, 0.9898214418809326842, 1.000000000000000000, 0.9898214418809326842, 1.000000000000000000, 0.9898214418809326842, 1.000000000000000000, 0.9898214418809326842, 1.000000000000000000, 0.9898214418809326842, 1.000000000000000000, 0.9898214418809326842, 1.000000000000000000, 0.9898214418809326842, 1.000000000000000000, 0.9898214418809326842, 1.000000000000000000, 0.9898214418809326842, 1.000000000000000000, 0.9898214418809326842, 1.000000000000000000, 0.9898214418809326842, 1.000000000000000000, 0.9898214418809326842, 1.000000000000000000, 0.9898214418809326842, 1.000000000000000000, 0.9898214418809326842, 1.000000000000000000, 0.9898214418809326842, 1.000000000000000000, 0.9898214418809326842, 1.000000000000000000, 0.9898214418809326842, 1.000000000000000000, 0.9898214418809326842, 1.000000000000000000, 0.9898214418809326842, 1.000000000000000000, 0.9898214418809326842, 1.000000000000000000, 0.9898214418809326842, 1.000000000000000000, 0.9898214418809326842, 1.000000000000000000, 0.9898214418809326842, 1.000000000000000000, 0.9898214418809326842, 1.000000000000000000, 0.9898214418809326842, 1.000000000000000000, 0.9898214418809326842, 1.000000000000000000, 0.9898214418809326842, 1.000000000000000000, 0.9898214418809326842, 1.000000000000000000, 0.9898214418809326842, 1.000000000000000000, 0.9898214418809326842, 1.000000000000000000, 0.9898214418809326842, 1.000000000000000000, 0.9898214418809326842, 1.000000000000000000, 0.9898214418809326842, 1.000000000000000000, 0.9898214418809326842, 1.000000000000000000, 0.9898214418809326842, 1.000000000000000000, 0.9898214418809326842, 1.000000000000000000, 0.9898214418809326842, 1.000000000000000000, 0.9898214418809326842, 1.000000000000000000, 0.9898214418809326842, 1.000000000000000000, 0.9898214418809326842, 1.000000000000000000, 0.9898214418809326842, 1.000000000000000000, 0.9898214418809326842, 1.000000000000000000, 0.9898214418809326842, 1.000000000000000000, 0.9898214418809326842, 1.000000000000000000, 0.9898214418809326842, 1.000000000000000000, 0.9898214418809326842, 1.000000000000000000, 0.9898214418809326842, 1.000000000000000000, 0.9898214418809326842, 1.000000000000000000, 0.9898214418809326842, 1.000000000000000000, 0.9898214418809326842, 1.000000000000000000, 0.9898214418809326842, 1.000000000000000000, 0.9898214418809326842, 1.000000000000000000, 0.9898214418809326842, 1.000000000000000000, 0.9898214418809326842, 1.000000000000000000, 0.9898214418809326842, 1.000000000000000000, 0.9898214418809326842, 1.000000000000000000, 0.9898214418809326842, 1.000000000000000000, 0.9968793409778355930, 0.9956722167842187998 ) ) 
 REPRESENTATION_ITEM ( '' )  );
#6 = VERTEX_POINT ( 'NONE', #33122 ) ;
#7 = CARTESIAN_POINT ( 'NONE',  ( 770.0799878456142551, -205.9874144716870035, -362.9823548866085616 ) ) ;
#8 = CARTESIAN_POINT ( 'NONE',  ( 781.8018195045266339, -190.2709662947835909, 365.1927285166406705 ) ) ;
#9 = CARTESIAN_POINT ( 'NONE',  ( 768.8385539511368734, -47.26014174441477422, -306.4236121716840557 ) ) ;
#10 = CARTESIAN_POINT ( 'NONE',  ( 757.8323909638828582, -314.6346026584195101, 352.1044303154654358 ) ) ;
#11 = LINE ( 'NONE', #39516, #42666 ) ;
#12 = ORIENTED_EDGE ( 'NONE', *, *, #22946, .T. ) ;
#13 = CARTESIAN_POINT ( 'NONE',  ( 755.8398074228967971, -67.44195992623289726, 333.4516893846970333 ) ) ;
#14 = CARTESIAN_POINT ( 'NONE',  ( 786.2694204179717872, -309.2817908451525568, -305.1769319972829067 ) ) ;
#15 = CARTESIAN_POINT ( 'NONE',  ( 812.7932403749906598, -255.1800572038742700, 327.7687537140311633 ) ) ;
#16 = CARTESIAN_POINT ( 'NONE',  ( 748.3538107759620743, 7.285312801039605546, 355.8262568251490165 ) ) ;
#17 = CARTESIAN_POINT ( 'NONE',  ( 758.4439275373578084, -156.5545181178802636, -353.2243759319684386 ) ) ;
#18 = CARTESIAN_POINT ( 'NONE',  ( 804.9363028652555840, -160.2709662947836762, -338.2165204200192079 ) ) ;
#19 = CARTESIAN_POINT ( 'NONE',  ( 755.3201227861273992, -339.7255117493285184, -345.3687786644892981 ) ) ;
#20 = ORIENTED_EDGE ( 'NONE', *, *, #3532, .T. ) ;
#21 = CARTESIAN_POINT ( 'NONE',  ( 808.0189434323515343, -278.0891481129651197, 319.0252816721025511 ) ) ;
#22 = CARTESIAN_POINT ( 'NONE',  ( 798.6699377194444196, -457.0491014588743042, 363.8754770338464368 ) ) ;
#23 = CARTESIAN_POINT ( 'NONE',  ( 756.1348686366196716, -329.2601417444138860, 347.5531968255698416 ) ) ;
#24 = CARTESIAN_POINT ( 'NONE',  ( 787.4999999999992042, -462.9681489794447202, -270.0000000000000568 ) ) ;
#25 = CARTESIAN_POINT ( 'NONE',  ( 800.9840315886518738, -148.9181544815166092, 354.1144889064786412 ) ) ;
#26 = CARTESIAN_POINT ( 'NONE',  ( 788.7366044899766848, -11.90732993114778182, 316.5762568750059813 ) ) ;
#27 = ORIENTED_EDGE ( 'NONE', *, *, #22756, .F. ) ;
#28 = CARTESIAN_POINT ( 'NONE',  ( 799.9636004259356241, -382.9181544815159555, -311.2241431872006956 ) ) ;
#29 = LINE ( 'NONE', #5647, #43867 ) ;
#30 = CARTESIAN_POINT ( 'NONE',  ( 745.7194118038753459, -229.6454272087890729, 348.7631598425976449 ) ) ;
#31 = CARTESIAN_POINT ( 'NONE',  ( 776.9566956441375396, -180.8965053807779952, 364.8461984189686405 ) ) ;
#32 = CARTESIAN_POINT ( 'NONE',  ( 804.4286716492782716, -377.3618753856920875, -345.3141322388244703 ) ) ;
#33 = CARTESIAN_POINT ( 'NONE',  ( 772.4999999999993179, -512.9681489794448908, 339.9999999999999432 ) ) ;
#34 = CARTESIAN_POINT ( 'NONE',  ( 755.5913626894240451, -229.6454272087890729, -346.6156483768012890 ) ) ;
#35 = CARTESIAN_POINT ( 'NONE',  ( 759.0252816721024374, -0.9982390220569063999, 368.0189434323527280 ) ) ;
#36 = CARTESIAN_POINT ( 'NONE',  ( 801.4587497624105481, -452.9681489794446634, 353.8271441104080282 ) ) ;
#37 = CARTESIAN_POINT ( 'NONE',  ( 796.7737145352015204, -404.6346026584193396, -370.7187646348536987 ) ) ;
#38 = ADVANCED_FACE ( 'NONE', ( #15558 ), #12093, .F. ) ;
#39 = LINE ( 'NONE', #14132, #32055 ) ;
#40 = CARTESIAN_POINT ( 'NONE',  ( 814.2805881961230625, -337.6454272087888171, 331.2368401574024119 ) ) ;
#41 = DIRECTION ( 'NONE',  ( 1.000000000000000000, 0.000000000000000000, 0.000000000000000000 ) ) ;
#42 = CARTESIAN_POINT ( 'NONE',  ( 814.9108240113580450, -328.2709662947831362, 337.5031285880265273 ) ) ;
#43 = CARTESIAN_POINT ( 'NONE',  ( 812.7932403749906598, -39.18005720387496638, -327.7687537140311633 ) ) ;
#44 = CARTESIAN_POINT ( 'NONE',  ( 803.6646147819161570, -281.9073299311468759, -348.8264449731210561 ) ) ;
#45 = CARTESIAN_POINT ( 'NONE',  ( -454.7528517110260964, 240.0000000000001421, -122.7905160835438068 ) ) ;
#46 = CARTESIAN_POINT ( 'NONE',  ( 781.8018195045266339, -430.2709662947827383, 365.1927285166406705 ) ) ;
#47 = CARTESIAN_POINT ( 'NONE',  ( 799.2566176426618085, -168.0090635724256458, 324.0069404352559559 ) ) ;
#48 = CARTESIAN_POINT ( 'NONE',  ( 773.7305795820266212, -33.28179084515333130, -374.8230680027170365 ) ) ;
#49 = CARTESIAN_POINT ( 'NONE',  ( 760.5453621957607311, -93.07832356259645223, -323.8424801807151425 ) ) ;
#50 = CARTESIAN_POINT ( 'NONE',  ( 815.0009284576459549, -102.3510508353236901, 338.7629533639073429 ) ) ;
#51 = CARTESIAN_POINT ( 'NONE',  ( 795.1360043628808398, -404.0891481129646650, 360.2193346964456282 ) ) ;
#52 = CYLINDRICAL_SURFACE ( 'NONE', #32876, 9.999999999999980460 ) ;
#53 = CARTESIAN_POINT ( 'NONE',  ( 771.2368401574024119, -157.4419599262326130, 374.2805881961240857 ) ) ;
#54 = CARTESIAN_POINT ( 'NONE',  ( 804.9363028652555840, -448.2709662947827951, 338.2165204200192079 ) ) ;
#56 = VERTEX_POINT ( 'NONE', #45682 ) ;
#55 = CARTESIAN_POINT ( 'NONE',  ( 793.2243759319678702, -98.53286901714187707, -318.4439275373583200 ) ) ;
#57 = CARTESIAN_POINT ( 'NONE',  ( 794.9819416627830151, -84.99823902205663728, -319.9864689768909898 ) ) ;
#58 = CARTESIAN_POINT ( 'NONE',  ( 805.1016975059191054, -390.8965053807772279, -343.0745993439771837 ) ) ;
#59 = EDGE_CURVE ( 'NONE', #755, #21705, #14891, .T. ) ;
#61 = CARTESIAN_POINT ( 'NONE',  ( 797.8594530101009923, -229.5436935675107009, 322.1405469898982119 ) ) ;
#60 = CARTESIAN_POINT ( 'NONE',  ( 767.8955696845333705, -240.4527844766015221, 362.1676090361162323 ) ) ;
#62 = CARTESIAN_POINT ( 'NONE',  ( 791.1614460488616487, -395.2601417444136587, -373.5763878283158874 ) ) ;
#63 = CARTESIAN_POINT ( 'NONE',  ( 812.6845335610512393, -439.9874144716862929, 353.5525998758768651 ) ) ;
#64 = DIRECTION ( 'NONE',  ( 0.000000000000000000, 0.000000000000000000, 1.000000000000000000 ) ) ;
#65 = ORIENTED_EDGE ( 'NONE', *, *, #36847, .T. ) ;
#66 = VERTEX_POINT ( 'NONE', #43052 ) ;
#67 = CARTESIAN_POINT ( 'NONE',  ( 814.5518280994195948, -255.7255117493287742, -332.4837098697145734 ) ) ;
#68 = CARTESIAN_POINT ( 'NONE',  ( 767.7687537140311633, -143.9073299311473590, 372.7932403749916830 ) ) ;
#69 = VERTEX_POINT ( 'NONE', #2595 ) ;
#70 = CARTESIAN_POINT ( 'NONE',  ( 752.4576283171824116, -189.0783235625961822, 317.7880784355627952 ) ) ;
#71 = CARTESIAN_POINT ( 'NONE',  ( 755.5713283507202505, -245.3618753856925139, -334.6858677611754729 ) ) ;
#72 = ORIENTED_EDGE ( 'NONE', *, *, #44085, .T. ) ;
#73 = CARTESIAN_POINT ( 'NONE',  ( 767.8955696845333705, -360.4527844766010958, -362.1676090361162323 ) ) ;
#74 = CARTESIAN_POINT ( 'NONE',  ( 778.2165204200184689, -22.81642084023865280, -364.9363028652563230 ) ) ;
#75 = CARTESIAN_POINT ( 'NONE',  ( 763.2154366446407039, -213.6237781080506011, 321.4292242960311228 ) ) ;
#76 = DIRECTION ( 'NONE',  ( 1.000000000000000000, -5.551115123125783688E-16, 0.000000000000000000 ) ) ;
#77 = CARTESIAN_POINT ( 'NONE',  ( -39.63011601220123481, -365.3551492539851893, -28.13243251470704109 ) ) ;
#78 = EDGE_CURVE ( 'NONE', #4330, #41889, #5365, .T. ) ;
#79 = PRODUCT ( 'Metal Bar', 'Metal Bar', '', ( #35741 ) ) ;
#80 = ORIENTED_EDGE ( 'NONE', *, *, #38468, .F. ) ;
#81 = CARTESIAN_POINT ( 'NONE',  ( 768.0187753319979720, -32.63460265842044095, -318.0580252608186242 ) ) ;
#82 = DIRECTION ( 'NONE',  ( -0.000000000000000000, -1.000000000000000000, -0.000000000000000000 ) ) ;
#83 = CARTESIAN_POINT ( 'NONE',  ( 745.7194118038753459, -277.6454272087889308, -348.7631598425976449 ) ) ;
#84 = CARTESIAN_POINT ( 'NONE',  ( 802.2119215644370342, -150.0090635724257027, 367.5423716828165084 ) ) ;
#86 = CARTESIAN_POINT ( 'NONE',  ( 795.1360043628807261, -212.0891481129652902, -360.2193346964456282 ) ) ;
#85 = CARTESIAN_POINT ( 'NONE',  ( -949.5497976682736407, 240.0000000000002274, -2132.806278688367456 ) ) ;
#87 = CARTESIAN_POINT ( 'NONE',  ( 787.6308680596127942, -395.2601417444136587, -364.1105419155492768 ) ) ;
#88 = LINE ( 'NONE', #17428, #8305 ) ;
#89 = CARTESIAN_POINT ( 'NONE',  ( 779.4763451958990572, -104.7363362996985785, -365.0264073115438919 ) ) ;
#90 = EDGE_CURVE ( 'NONE', #25509, #42507, #33534, .T. ) ;
#91 = CARTESIAN_POINT ( 'NONE',  ( 781.2370466360911223, -380.7363362996977116, 304.9990715423533629 ) ) ;
#92 = DIRECTION ( 'NONE',  ( -1.000000000000000000, 0.000000000000000000, 0.000000000000000000 ) ) ;
#93 = CARTESIAN_POINT ( 'NONE',  ( 745.1769319972822814, 6.194403710130517382, -346.2694204179732083 ) ) ;
#94 = CARTESIAN_POINT ( 'NONE',  ( 792.2312462859673587, -323.9073299311468190, -307.2067596250082602 ) ) ;
#95 = DIRECTION ( 'NONE',  ( 1.000000000000000000, 0.000000000000000000, 0.000000000000000000 ) ) ;
#96 = CARTESIAN_POINT ( 'NONE',  ( 788.7366044899766848, -11.90732993114778182, 316.5762568750059813 ) ) ;
#97 = CARTESIAN_POINT ( 'NONE',  ( 771.2633955100217236, -71.90732993114760063, -363.4237431249939618 ) ) ;
#98 = CARTESIAN_POINT ( 'NONE',  ( 786.2694204179717872, -261.2817908451526705, 305.1769319972829067 ) ) ;
#99 = CARTESIAN_POINT ( 'NONE',  ( 793.4146539503750546, -193.9874144716870319, -307.6481478633938877 ) ) ;
#100 = CARTESIAN_POINT ( 'NONE',  ( 814.2001403089898304, -209.3618753856926276, 347.4397851343538264 ) ) ;
#101 = CARTESIAN_POINT ( 'NONE',  ( 792.2312462859673587, -443.9073299311464780, -307.2067596250082602 ) ) ;
#102 = FACE_OUTER_BOUND ( 'NONE', #34490, .T. ) ;
#103 = CARTESIAN_POINT ( 'NONE',  ( 804.9363028652555840, -304.2709662947832499, 338.2165204200192079 ) ) ;
#104 = CARTESIAN_POINT ( 'NONE',  ( 802.9823548866075953, -97.09997266333496668, 330.0799878456151077 ) ) ;
#105 = ADVANCED_FACE ( 'NONE', ( #37931 ), #16695, .F. ) ;
#106 = CARTESIAN_POINT ( 'NONE',  ( 803.6646147819161570, -449.9073299311463643, -348.8264449731210561 ) ) ;
#107 = CARTESIAN_POINT ( 'NONE',  ( 779.9999999999992042, -462.9681489794448339, -370.0000000000000568 ) ) ;
#109 = EDGE_CURVE ( 'NONE', #28297, #10740, #37704, .T. ) ;
#108 = CARTESIAN_POINT ( 'NONE',  ( 799.9999999999993179, 205.0000000000000568, 319.9999999999999432 ) ) ;
#111 = CARTESIAN_POINT ( 'NONE',  ( 768.0187753319979720, -368.6346026584193964, 318.0580252608186242 ) ) ;
#110 = CARTESIAN_POINT ( 'NONE',  ( 776.9566956441375396, -132.8965053807781374, 364.8461984189686405 ) ) ;
#112 = ORIENTED_EDGE ( 'NONE', *, *, #9772, .T. ) ;
#113 = CARTESIAN_POINT ( 'NONE',  ( 756.1348686366196716, -305.2601417444139429, -347.5531968255698416 ) ) ;
#114 = EDGE_CURVE ( 'NONE', #22938, #120, #8459, .T. ) ;
#115 = CARTESIAN_POINT ( 'NONE',  ( 795.1360043628807261, -140.0891481129654892, 360.2193346964456282 ) ) ;
#116 = CARTESIAN_POINT ( 'NONE',  ( 788.7366044899766848, -107.9073299311474727, 316.5762568750059813 ) ) ;
#117 = CARTESIAN_POINT ( 'NONE',  ( 749.8865473780648472, -284.5328690171412518, -322.1177392798429082 ) ) ;
#118 = LINE ( 'NONE', #10283, #45262 ) ;
#119 = CARTESIAN_POINT ( 'NONE',  ( 788.7631598425961101, -409.4419599262317320, 305.7194118038759143 ) ) ;
#120 = VERTEX_POINT ( 'NONE', #34001 ) ;
#121 = CARTESIAN_POINT ( 'NONE',  ( 805.1927285166397041, -328.8164208402375834, 341.8018195045277707 ) ) ;
#122 = CARTESIAN_POINT ( 'NONE',  ( 803.8651313633788504, -53.26014174441475291, -332.4468031744301015 ) ) ;
#123 = CARTESIAN_POINT ( 'NONE',  ( 756.5762568750052424, -147.1800572038746395, -348.7366044899774238 ) ) ;
#124 = CARTESIAN_POINT ( 'NONE',  ( 797.8594530101008786, -205.5436935675108430, -322.1405469898980982 ) ) ;
#125 = CARTESIAN_POINT ( 'NONE',  ( 794.9819416627830151, -420.9982390220555999, 319.9864689768909898 ) ) ;
#126 = CARTESIAN_POINT ( 'NONE',  ( 745.7998596910086917, -149.3618753856928265, -332.5602148656461168 ) ) ;
#127 = APPLICATION_CONTEXT ( 'automotive_design' ) ;
#128 = PRESENTATION_LAYER_ASSIGNMENT (  '', '', ( #19308 ) ) ;
#129 = CARTESIAN_POINT ( 'NONE',  ( 755.5713283507202505, -125.3618753856928834, -334.6858677611754729 ) ) ;
#130 = ORIENTED_EDGE ( 'NONE', *, *, #13131, .F. ) ;
#131 = CARTESIAN_POINT ( 'NONE',  ( 800.9840315886518738, -388.9181544815158986, -354.1144889064786412 ) ) ;
#132 = EDGE_CURVE ( 'NONE', #43251, #1390, #14358, .T. ) ;
#133 = CARTESIAN_POINT ( 'NONE',  ( 763.0428371773158460, -443.4636090269702322, 358.7617431975195359 ) ) ;
#134 = CARTESIAN_POINT ( 'NONE',  ( 800.7704444035546203, -124.1692326535054463, 326.0291762391768771 ) ) ;
#137 = CARTESIAN_POINT ( 'NONE',  ( 801.9858362298568863, -387.0783235625955285, 312.7379699480935642 ) ) ;
#136 = CARTESIAN_POINT ( 'NONE',  ( 701.1634899080286232, 259.9999999999999432, -208.0249999999989825 ) ) ;
#135 = DIRECTION ( 'NONE',  ( 0.000000000000000000, 1.110223024625155554E-15, -1.000000000000000000 ) ) ;
#138 = EDGE_CURVE ( 'NONE', #11154, #34810, #22920, .T. ) ;
#139 = ORIENTED_EDGE ( 'NONE', *, *, #25849, .T. ) ;
#140 = CARTESIAN_POINT ( 'NONE',  ( 772.4468031744293057, -393.8272453906067199, -363.8651313633793620 ) ) ;
#141 = CARTESIAN_POINT ( 'NONE',  ( 756.3353852180819104, -365.9073299311465917, -331.1735550268788302 ) ) ;
#142 = CARTESIAN_POINT ( 'NONE',  ( 781.2370466360911223, -164.7363362996983938, -304.9990715423533629 ) ) ;
#143 = CARTESIAN_POINT ( 'NONE',  ( 797.8822607201568644, -30.55451811788062244, 370.1134526219340160 ) ) ;
#145 = CARTESIAN_POINT ( 'NONE',  ( 187.1337867209877857, 56.73212367640085318, 362.5753187112032379 ) ) ;
#144 = CARTESIAN_POINT ( 'NONE',  ( -786.4999999999993179, -512.9681489794448908, -339.9999999999999432 ) ) ;
#146 = CARTESIAN_POINT ( 'NONE',  ( 805.0264073115434940, -294.3510508353230648, -339.4763451958999099 ) ) ;
#147 = CARTESIAN_POINT ( 'NONE',  ( 803.6646147819161570, -449.9073299311463643, -348.8264449731210561 ) ) ;
#148 = CARTESIAN_POINT ( 'NONE',  ( 802.2119215644370342, -150.0090635724257027, -367.5423716828165084 ) ) ;
#149 = LINE ( 'NONE', #21398, #31138 ) ;
#150 = CARTESIAN_POINT ( 'NONE',  ( 441.1634899080286232, 259.9999999999999432, -208.0249999999972488 ) ) ;
#151 = EDGE_CURVE ( 'NONE', #10014, #17032, #19697, .T. ) ;
#152 = CARTESIAN_POINT ( 'NONE',  ( 755.3028492785439312, -351.2817908451523294, 335.9200461376539693 ) ) ;
#153 = CARTESIAN_POINT ( 'NONE',  ( 805.6418435158337843, -341.4636090269705733, 363.8556311672236916 ) ) ;
#154 = CARTESIAN_POINT ( 'NONE',  ( 749.2812353651451076, -198.4527844766017495, -323.2262854647983090 ) ) ;
#155 = DIRECTION ( 'NONE',  ( 0.000000000000000000, 0.000000000000000000, 1.000000000000000000 ) ) ;
#156 = CARTESIAN_POINT ( 'NONE',  ( 311.1634899080286232, 260.0000000000000000, -208.0249999999963109 ) ) ;
#157 = CARTESIAN_POINT ( 'NONE',  ( 778.7629533639073998, -152.7363362996983938, 375.0009284576466371 ) ) ;
#158 = CARTESIAN_POINT ( 'NONE',  ( 746.7653713866222915, -113.2601417444145682, -351.0478386215610271 ) ) ;
#159 = CARTESIAN_POINT ( 'NONE',  ( 792.3570229623688874, -117.1800572038746964, 373.1304606946836202 ) ) ;
#160 = CARTESIAN_POINT ( 'NONE',  ( 754.9967657858570647, -337.5436935675102177, -365.0032342141425374 ) ) ;
#161 = LINE ( 'NONE', #18412, #9196 ) ;
#162 = CARTESIAN_POINT ( 'NONE',  ( -208.8365100919714052, 260.0000000000001137, -197.2499999999928377 ) ) ;
#163 = CARTESIAN_POINT ( 'NONE',  ( 768.0187753319979720, -200.6346026584199365, 318.0580252608186242 ) ) ;
#164 = VECTOR ( 'NONE', #10534, 1000.000000000000000 ) ;
#165 = CARTESIAN_POINT ( 'NONE',  ( 776.9254006560222479, 3.809118245755632959, 314.8983024940802125 ) ) ;
#166 = CARTESIAN_POINT ( 'NONE',  ( 791.1614460488616487, -395.2601417444136587, -373.5763878283158874 ) ) ;
#167 = CARTESIAN_POINT ( 'NONE',  ( 745.7998596910086917, -413.3618753856920307, -332.5602148656461168 ) ) ;
#169 = EDGE_CURVE ( 'NONE', #1813, #29494, #23376, .T. ) ;
#168 = CARTESIAN_POINT ( 'NONE',  ( -338.8365100919713200, 256.5000000000001137, -199.9999999999917861 ) ) ;
#170 = CARTESIAN_POINT ( 'NONE',  ( 808.7758568127978833, -4.169232653505813069, 320.0363995740631822 ) ) ;
#171 = ORIENTED_EDGE ( 'NONE', *, *, #19921, .T. ) ;
#172 = CARTESIAN_POINT ( 'NONE',  ( 776.2433038121456548, -180.8965053807779952, -374.8207195650711014 ) ) ;
#173 = CARTESIAN_POINT ( 'NONE',  ( 791.1614460488616487, -323.2601417444138860, 373.5763878283158874 ) ) ;
#174 = CARTESIAN_POINT ( 'NONE',  ( 754.8072714833583632, -124.8164208402383366, 338.1981804954721156 ) ) ;
#175 = ORIENTED_EDGE ( 'NONE', *, *, #22188, .T. ) ;
#176 = CARTESIAN_POINT ( 'NONE',  ( 785.3141322388236176, -309.7255117493287457, 364.4286716492789537 ) ) ;
#177 = CARTESIAN_POINT ( 'NONE',  ( 747.2067596250078623, -27.18005720387500901, -352.2312462859687230 ) ) ;
#178 = VECTOR ( 'NONE', #201, 1000.000000000000114 ) ;
#179 = CARTESIAN_POINT ( 'NONE',  ( 792.2312462859673587, -83.90732993114754379, 307.2067596250082602 ) ) ;
#180 = ORIENTED_EDGE ( 'NONE', *, *, #7452, .F. ) ;
#181 = CARTESIAN_POINT ( 'NONE',  ( 810.4231160770870019, -456.5545181178792404, -321.9338519418446936 ) ) ;
#182 = ORIENTED_EDGE ( 'NONE', *, *, #32039, .F. ) ;
#183 = APPLICATION_PROTOCOL_DEFINITION ( 'draft international standard', 'automotive_design', 1998, #20748 ) ;
#184 = EDGE_CURVE ( 'NONE', #12197, #1931, #19516, .T. ) ;
#185 = CARTESIAN_POINT ( 'NONE',  ( 778.2165204200184689, -22.81642084023865280, 364.9363028652563230 ) ) ;
#186 = CARTESIAN_POINT ( 'NONE',  ( 785.3141322388236176, -285.7255117493286889, -364.4286716492789537 ) ) ;
#188 = CARTESIAN_POINT ( 'NONE',  ( 747.3154664389472828, -283.9874144716867477, 326.4474001241230781 ) ) ;
#187 = CARTESIAN_POINT ( 'NONE',  ( 805.0032342141413437, -349.5436935675103314, 314.9967657858572352 ) ) ;
#189 = ADVANCED_FACE ( 'NONE', ( #37479 ), #13000, .F. ) ;
#190 = CARTESIAN_POINT ( 'NONE',  ( 808.7758568127978833, -76.16923265350557415, 320.0363995740631822 ) ) ;
#191 = CARTESIAN_POINT ( 'NONE',  ( 799.2566176426618085, -264.0090635724253616, -324.0069404352559559 ) ) ;
#192 = CARTESIAN_POINT ( 'NONE',  ( 778.2165204200184689, -238.8164208402379813, -364.9363028652563230 ) ) ;
#193 = CARTESIAN_POINT ( 'NONE',  ( -879.9999999999992042, 529.9999999999997726, -360.0000000000000000 ) ) ;
#194 = CARTESIAN_POINT ( 'NONE',  ( 800.0135310231082713, -110.0891481129656597, -325.0180583372163028 ) ) ;
#195 = DIRECTION ( 'NONE',  ( 0.000000000000000000, -1.000000000000000000, 1.672022627447525240E-16 ) ) ;
#196 = CARTESIAN_POINT ( 'NONE',  ( 782.4968714119720516, -394.8164208402374697, 305.0891759886411023 ) ) ;
#198 = CARTESIAN_POINT ( 'NONE',  ( 791.7608162188021197, 205.0000000000000568, -339.9999999999999432 ) ) ;
#197 = CARTESIAN_POINT ( 'NONE',  ( 784.4999999999993179, -513.1383975375929367, -369.9999999999999432 ) ) ;
#199 = CARTESIAN_POINT ( 'NONE',  ( 755.8990559732751535, -35.46360902697151829, -365.9055244015606831 ) ) ;
#200 = CARTESIAN_POINT ( 'NONE',  ( 779.9999999999992042, 16.45630643248849267, -339.9999999999999432 ) ) ;
#202 = EDGE_CURVE ( 'NONE', #18957, #27321, #40211, .T. ) ;
#201 = DIRECTION ( 'NONE',  ( -1.236450975029139710E-16, 0.7517448203044212462, 0.6594541114781782287 ) ) ;
#203 = CARTESIAN_POINT ( 'NONE',  ( 780.5236548040995785, -260.7363362996981095, 314.9735926884559944 ) ) ;
#204 = CARTESIAN_POINT ( 'NONE',  ( 788.8264449731200330, -117.1800572038746964, 363.6646147819171233 ) ) ;
#205 = EDGE_LOOP ( 'NONE', ( #30686, #19358, #44949, #34895 ) ) ;
#206 = CARTESIAN_POINT ( 'NONE',  ( 780.5236548040995785, 3.263663700301089765, -314.9735926884559944 ) ) ;
#207 = CARTESIAN_POINT ( 'NONE',  ( 808.3070685750232087, -114.9982390220565378, -361.1904061080339829 ) ) ;
#208 = CARTESIAN_POINT ( 'NONE',  ( 801.3366627262608972, -296.5328690171411949, 353.0897708529566899 ) ) ;
#209 = PLANE ( 'NONE',  #44022 ) ;
#210 = CARTESIAN_POINT ( 'NONE',  ( 814.4686193811664907, -51.28179084515328867, 346.2056067578752732 ) ) ;
#211 = CARTESIAN_POINT ( 'NONE',  ( 796.9462024416508257, -228.4527844766015789, -308.9653473494370246 ) ) ;
#212 = CARTESIAN_POINT ( 'NONE',  ( 814.5518280994195948, -183.7255117493290015, 332.4837098697145734 ) ) ;
#213 = CARTESIAN_POINT ( 'NONE',  ( 774.6312213355099630, -71.36187538569302546, 364.6798772138717482 ) ) ;
#214 = AXIS2_PLACEMENT_3D ( 'NONE', #42407, #11013, #31569 ) ;
#215 = DIRECTION ( 'NONE',  ( 0.000000000000000000, 0.000000000000000000, 1.000000000000000000 ) ) ;
#216 = CARTESIAN_POINT ( 'NONE',  ( 773.7943932421234194, -287.8055962898685038, -305.5313806188329409 ) ) ;
#217 = CARTESIAN_POINT ( 'NONE',  ( 802.2119215644370342, -438.0090635724247932, 367.5423716828165084 ) ) ;
#218 = CARTESIAN_POINT ( 'NONE',  ( 749.2812353651451076, -318.4527844766014368, -323.2262854647983090 ) ) ;
#219 = LINE ( 'NONE', #30953, #25011 ) ;
#220 = CARTESIAN_POINT ( 'NONE',  ( 787.6308680596127942, -347.2601417444138860, 364.1105419155492768 ) ) ;
#221 = CARTESIAN_POINT ( 'NONE',  ( 745.7998596910086917, -53.36187538569310362, 332.5602148656461168 ) ) ;
#222 = CARTESIAN_POINT ( 'NONE',  ( 756.5762568750052424, -387.1800572038738437, -348.7366044899774238 ) ) ;
#223 = CARTESIAN_POINT ( 'NONE',  ( 776.9566956441375396, -60.89650538077837894, 364.8461984189686405 ) ) ;
#224 = CARTESIAN_POINT ( 'NONE',  ( 755.0636971347428243, -196.2709662947835909, -341.7834795799807353 ) ) ;
#225 = CARTESIAN_POINT ( 'NONE',  ( 776.2433038121456548, -84.89650538077830788, -374.8207195650711014 ) ) ;
#226 = CARTESIAN_POINT ( 'NONE',  ( 773.7943932421234194, -215.8055962898687881, 305.5313806188329409 ) ) ;
#227 = CARTESIAN_POINT ( 'NONE',  ( 781.7834795799800531, -10.81642084023869543, 315.0636971347436202 ) ) ;
#228 = EDGE_LOOP ( 'NONE', ( #38649, #28007, #19169, #34955 ) ) ;
#229 = CARTESIAN_POINT ( 'NONE',  ( 779.4709603349208464, -216.3510508353233490, -314.7162404726379918 ) ) ;
#230 = CARTESIAN_POINT ( 'NONE',  ( 791.9812246680005501, -212.6346026584198796, 361.9419747391813189 ) ) ;
#231 = CARTESIAN_POINT ( 'NONE',  ( 798.0661480581538854, -50.53286901714203339, -309.5768839229118043 ) ) ;
#232 = CARTESIAN_POINT ( 'NONE',  ( 756.3353852180820240, -317.9073299311467622, 331.1735550268787733 ) ) ;
#233 = CARTESIAN_POINT ( 'NONE',  ( 808.9106007788763009, -452.9681489794446065, -335.7521713694408731 ) ) ;
#234 = DIRECTION ( 'NONE',  ( 1.000000000000000000, 0.000000000000000000, 0.000000000000000000 ) ) ;
#235 = ORIENTED_EDGE ( 'NONE', *, *, #15168, .F. ) ;
#236 = CARTESIAN_POINT ( 'NONE',  ( 789.9200121543843807, -49.98741447168749374, 317.0176451133914384 ) ) ;
#237 = CARTESIAN_POINT ( 'NONE',  ( 814.8207195650702488, -338.1908817542433212, -336.2433038121456548 ) ) ;
#238 = CARTESIAN_POINT ( 'NONE',  ( 759.0252816721024374, -264.9982390220561115, 368.0189434323527280 ) ) ;
#239 = CARTESIAN_POINT ( 'NONE',  ( 746.7653713866222915, 6.739858255585061464, 351.0478386215610271 ) ) ;
#240 = CARTESIAN_POINT ( 'NONE',  ( 754.7162404726377645, -134.7363362996984790, -339.4709603349214717 ) ) ;
#241 = CARTESIAN_POINT ( 'NONE',  ( 801.9419747391806368, -162.4527844766018632, -351.9812246680014027 ) ) ;
#242 = CIRCLE ( 'NONE', #11326, 24.99999999999991118 ) ;
#243 = CARTESIAN_POINT ( 'NONE',  ( 778.2165204200184689, -358.8164208402375834, -364.9363028652563230 ) ) ;
#244 = ORIENTED_EDGE ( 'NONE', *, *, #43927, .T. ) ;
#245 = AXIS2_PLACEMENT_3D ( 'NONE', #12504, #37447, #37670 ) ;
#246 = CARTESIAN_POINT ( 'NONE',  ( 763.0537975583475827, -288.4527844766014937, 371.0346526505627480 ) ) ;
#247 = CARTESIAN_POINT ( 'NONE',  ( 775.4999999999993179, -544.8427095258973623, -350.0000000000000000 ) ) ;
#248 = CARTESIAN_POINT ( 'NONE',  ( 794.1144889064781864, -322.1692326535048210, 360.9840315886528401 ) ) ;
#249 = DIRECTION ( 'NONE',  ( -0.000000000000000000, 1.000000000000000000, -0.000000000000000000 ) ) ;
#250 = CARTESIAN_POINT ( 'NONE',  ( 799.2566176426618085, -168.0090635724256458, 324.0069404352559559 ) ) ;
#251 = CARTESIAN_POINT ( 'NONE',  ( 759.9864689768902508, -26.08914811296592262, 354.9819416627836404 ) ) ;
#252 = ORIENTED_EDGE ( 'NONE', *, *, #2953, .T. ) ;
#253 = CARTESIAN_POINT ( 'NONE',  ( 810.4231160770870019, -384.5545181178795247, -321.9338519418446936 ) ) ;
#254 = CARTESIAN_POINT ( 'NONE',  ( 782.4968714119720516, 13.18357915976123174, -305.0891759886411023 ) ) ;
#255 = CARTESIAN_POINT ( 'NONE',  ( 750.9282345327678740, -232.9181544815163249, 319.8311093483690115 ) ) ;
#256 = CARTESIAN_POINT ( 'NONE',  ( 786.6156483768007774, -193.4419599262325278, 315.5913626894246136 ) ) ;
#257 = CARTESIAN_POINT ( 'NONE',  ( 771.2633955100217236, -359.9073299311467053, -363.4237431249939618 ) ) ;
#258 = VECTOR ( 'NONE', #1525, 1000.000000000000000 ) ;
#259 = CARTESIAN_POINT ( 'NONE',  ( 781.7834795799800531, 13.18357915976123174, 315.0636971347436202 ) ) ;
#260 = LINE ( 'NONE', #35579, #37744 ) ;
#261 = CARTESIAN_POINT ( 'NONE',  ( 784.1219089521767955, -237.2817908451526421, -315.0488828828318333 ) ) ;
#262 = CARTESIAN_POINT ( 'NONE',  ( 767.6429770376289525, -9.180057203875058747, 306.8695393053162093 ) ) ;
#263 = CARTESIAN_POINT ( 'NONE',  ( 782.4968714119720516, -82.81642084023846451, 305.0891759886411023 ) ) ;
#264 = CARTESIAN_POINT ( 'NONE',  ( 779.9999999999992042, 126.4563064324884465, -329.9999999999999432 ) ) ;
#265 = CARTESIAN_POINT ( 'NONE',  ( 808.3070685750232087, -426.9982390220555430, -361.1904061080339829 ) ) ;
#266 = CARTESIAN_POINT ( 'NONE',  ( -180.7583438952258348, 394.6698570112193920, -224.9999999999999716 ) ) ;
#267 =( BOUNDED_CURVE ( )  B_SPLINE_CURVE ( 3, ( #30983, #13892, #3032, #6720 ),
 .UNSPECIFIED., .F., .T. ) 
 B_SPLINE_CURVE_WITH_KNOTS ( ( 4, 4 ),
 ( 1.570796326794896558, 3.141592653589793116 ),
 .UNSPECIFIED. ) 
 CURVE ( )  GEOMETRIC_REPRESENTATION_ITEM ( )  RATIONAL_B_SPLINE_CURVE ( ( 1.000000000000000000, 0.8047378541243649375, 0.8047378541243649375, 1.000000000000000000 ) ) 
 REPRESENTATION_ITEM ( '' )  );
#268 = CARTESIAN_POINT ( 'NONE',  ( 793.5525998758768083, -367.0999726633342561, 372.6845335610516941 ) ) ;
#269 = CARTESIAN_POINT ( 'NONE',  ( 809.4421496042219815, -454.3218287316016699, -345.7584569706272077 ) ) ;
#270 = CARTESIAN_POINT ( 'NONE',  ( 767.7687537140311633, -335.9073299311468190, 372.7932403749916830 ) ) ;
#271 = CARTESIAN_POINT ( 'NONE',  ( 796.9462024416508257, -60.45278447660215448, -308.9653473494370246 ) ) ;
#272 = CARTESIAN_POINT ( 'NONE',  ( 758.0580252608178853, -270.4527844766014937, -328.0187753319985404 ) ) ;
#273 = CARTESIAN_POINT ( 'NONE',  ( 879.9999999999992042, 479.9999999999998863, -210.0000000000000000 ) ) ;
#274 = CARTESIAN_POINT ( 'NONE',  ( 759.9864689768902508, -434.0891481129646081, 354.9819416627836404 ) ) ;
#275 = CARTESIAN_POINT ( 'NONE',  ( 755.1538015810308480, -206.1908817542437191, 343.0433043558613804 ) ) ;
#276 = CARTESIAN_POINT ( 'NONE',  ( 764.1737431748507561, -58.37269993606236085, -371.6461892240376415 ) ) ;
#277 = CARTESIAN_POINT ( 'NONE',  ( 803.8651313633788504, -77.26014174441466764, -332.4468031744301015 ) ) ;
#278 = CARTESIAN_POINT ( 'NONE',  ( 786.2056067578752163, -107.8055962898691433, 374.4686193811670023 ) ) ;
#279 = CARTESIAN_POINT ( 'NONE',  ( 778.2165204200184689, -406.8164208402375266, 364.9363028652563230 ) ) ;
#280 = VECTOR ( 'NONE', #1161, 1000.000000000000000 ) ;
#281 = CARTESIAN_POINT ( 'NONE',  ( 801.9419747391806368, -450.4527844766009821, 351.9812246680014027 ) ) ;
#282 = VERTEX_POINT ( 'NONE', #6289 ) ;
#283 = CARTESIAN_POINT ( 'NONE',  ( 771.2633955100217236, -95.90732993114751537, -363.4237431249939618 ) ) ;
#284 = CARTESIAN_POINT ( 'NONE',  ( 803.8651313633788504, -389.2601417444136018, -332.4468031744301015 ) ) ;
#286 = CARTESIAN_POINT ( 'NONE',  ( 778.1981804954715471, -226.2709662947834488, 314.8072714833591021 ) ) ;
#285 = CARTESIAN_POINT ( 'NONE',  ( 762.3223304703356007, -223.5436935675107577, 322.3223304703362828 ) ) ;
#287 = CARTESIAN_POINT ( 'NONE',  ( 793.4146539503750546, -409.9874144716863498, -307.6481478633938877 ) ) ;
#288 = CARTESIAN_POINT ( 'NONE',  ( 919.9999999999993179, 219.9999999999998863, -360.0000000000000000 ) ) ;
#289 = EDGE_LOOP ( 'NONE', ( #32622, #40266, #14008, #33528 ) ) ;
#290 = CARTESIAN_POINT ( 'NONE',  ( 765.0180583372156207, -432.9982390220555999, 360.0135310231089534 ) ) ;
#291 = AXIS2_PLACEMENT_3D ( 'NONE', #13040, #41443, #41905 ) ;
#292 = ORIENTED_EDGE ( 'NONE', *, *, #37389, .F. ) ;
#293 = CARTESIAN_POINT ( 'NONE',  ( 796.7737145352015204, -260.6346026584197375, -370.7187646348536987 ) ) ;
#294 = CARTESIAN_POINT ( 'NONE',  ( 804.7487373415286811, -163.5436935675109567, 364.7487373415288516 ) ) ;
#295 = CARTESIAN_POINT ( 'NONE',  ( 759.0159684113467620, -280.9181544815162965, 325.8855110935213020 ) ) ;
#296 = VERTEX_POINT ( 'NONE', #37011 ) ;
#297 = CARTESIAN_POINT ( 'NONE',  ( 783.7566961878529810, -192.8965053807779668, 305.1792804349288417 ) ) ;
#298 = CARTESIAN_POINT ( 'NONE',  ( 764.8639956371174549, -248.0891481129651766, -319.7806653035542581 ) ) ;
#299 = ORIENTED_EDGE ( 'NONE', *, *, #28143, .F. ) ;
#300 = CARTESIAN_POINT ( 'NONE',  ( 788.7366044899766848, -371.9073299311465917, -316.5762568750059813 ) ) ;
#301 = CARTESIAN_POINT ( 'NONE',  ( 759.7806653035534055, -30.99823902205680071, -324.8639956371180801 ) ) ;
#302 = CARTESIAN_POINT ( 'NONE',  ( 790.8726784830453198, -226.7146871989596661, 362.5472867521010585 ) ) ;
#303 = CARTESIAN_POINT ( 'NONE',  ( -468.8365100919714337, 260.0000000000001705, -199.9999999999908766 ) ) ;
#304 = FACE_OUTER_BOUND ( 'NONE', #10068, .T. ) ;
#305 = ORIENTED_EDGE ( 'NONE', *, *, #27775, .T. ) ;
#306 = CARTESIAN_POINT ( 'NONE',  ( 794.9819416627830151, -12.99823902205686821, -319.9864689768909898 ) ) ;
#307 = DIRECTION ( 'NONE',  ( 1.000000000000000000, 0.000000000000000000, -0.000000000000000000 ) ) ;
#308 = DIRECTION ( 'NONE',  ( -1.880165489482579047E-16, -1.000000000000000000, -0.000000000000000000 ) ) ;
#309 = ORIENTED_EDGE ( 'NONE', *, *, #5989, .F. ) ;
#310 = CARTESIAN_POINT ( 'NONE',  ( 799.9636004259356241, -262.9181544815162965, -311.2241431872006956 ) ) ;
#311 = CARTESIAN_POINT ( 'NONE',  ( 762.1177392798416577, -138.5545181178802636, 309.8865473780659272 ) ) ;
#313 = CARTESIAN_POINT ( 'NONE',  ( 800.0135310231082713, -254.0891481129652334, -325.0180583372163028 ) ) ;
#312 = FACE_OUTER_BOUND ( 'NONE', #6954, .T. ) ;
#314 = CARTESIAN_POINT ( 'NONE',  ( 789.9200121543843807, -385.9874144716864066, -317.0176451133914384 ) ) ;
#315 = DIRECTION ( 'NONE',  ( 0.000000000000000000, 1.000000000000000000, -0.000000000000000000 ) ) ;
#316 = CARTESIAN_POINT ( 'NONE',  ( 763.0428371773158460, -131.4636090269711985, -358.7617431975195359 ) ) ;
#317 = EDGE_CURVE ( 'NONE', #3483, #7856, #33327, .T. ) ;
#318 = DIRECTION ( 'NONE',  ( 0.000000000000000000, 0.000000000000000000, 1.000000000000000000 ) ) ;
#319 = CARTESIAN_POINT ( 'NONE',  ( 808.7758568127978833, -4.169232653505813069, -320.0363995740631822 ) ) ;
#320 = CARTESIAN_POINT ( 'NONE',  ( 777.4774526936600978, -322.2709662947830793, -304.7301800767028226 ) ) ;
#321 = CARTESIAN_POINT ( 'NONE',  ( 759.9999999999992042, 205.0000000000000568, -360.0000000000000000 ) ) ;
#322 = CARTESIAN_POINT ( 'NONE',  ( 795.1360043628807261, 3.910851887033985896, 360.2193346964456282 ) ) ;
#323 = CIRCLE ( 'NONE', #21716, 6.118999999999985562 ) ;
#324 = CARTESIAN_POINT ( 'NONE',  ( 814.2805881961230625, -265.6454272087889876, 331.2368401574024119 ) ) ;
#325 = CARTESIAN_POINT ( 'NONE',  ( 813.2346286133761168, -197.2601417444143124, -328.9521613784389160 ) ) ;
#326 = CARTESIAN_POINT ( 'NONE',  ( 746.8695393053150156, -221.9073299311470464, 327.6429770376306010 ) ) ;
#327 = CARTESIAN_POINT ( 'NONE',  ( 755.2512626584698410, -439.5436935675101040, -315.2512626584710915 ) ) ;
#328 = CARTESIAN_POINT ( 'NONE',  ( 914.9999999999992042, 74.99999999999984368, 360.0000000000000000 ) ) ;
#329 = AXIS2_PLACEMENT_3D ( 'NONE', #6576, #23655, #31056 ) ;
#330 = CARTESIAN_POINT ( 'NONE',  ( 795.1360043628807261, -308.0891481129650629, 360.2193346964456282 ) ) ;
#331 = CARTESIAN_POINT ( 'NONE',  ( 772.4468031744293057, -81.82724539060772884, 363.8651313633793620 ) ) ;
#332 = CARTESIAN_POINT ( 'NONE',  ( 802.5472867521000353, -76.37269993606228979, 350.8726784830461156 ) ) ;
#333 = CARTESIAN_POINT ( 'NONE',  ( 790.8050863131179540, -452.8379544210779954, -362.5841948692291226 ) ) ;
#334 = PLANE ( 'NONE',  #18115 ) ;
#335 = DIRECTION ( 'NONE',  ( -0.000000000000000000, 1.000000000000000000, -0.000000000000000000 ) ) ;
#337 = CARTESIAN_POINT ( 'NONE',  ( 797.8594530101008786, -373.5436935675101040, 322.1405469898980982 ) ) ;
#336 = CARTESIAN_POINT ( 'NONE',  ( 773.3843516231979720, -109.4419599262327836, 364.4086373105754433 ) ) ;
#338 = VERTEX_POINT ( 'NONE', #40712 ) ;
#339 = VECTOR ( 'NONE', #33787, 1000.000000000000000 ) ;
#340 = CARTESIAN_POINT ( 'NONE',  ( 757.2208543904082489, -304.7146871989594388, -350.9844846989624330 ) ) ;
#341 = CARTESIAN_POINT ( 'NONE',  ( 803.4237431249931660, -111.1800572038747532, 331.2633955100225194 ) ) ;
#342 = AXIS2_PLACEMENT_3D ( 'NONE', #45315, #17601, #13908 ) ;
#343 = CARTESIAN_POINT ( 'NONE',  ( 766.5853460496234675, -301.9874144716867477, -372.3518521366060554 ) ) ;
#344 = CARTESIAN_POINT ( 'NONE',  ( 181.1634899080285948, 256.5000000000000000, -202.7499999999952820 ) ) ;
#345 = CARTESIAN_POINT ( 'NONE',  ( 800.1688906516307043, -418.1692326535044799, 369.0717654672308186 ) ) ;
#346 = VERTEX_POINT ( 'NONE', #30093 ) ;
#347 = CARTESIAN_POINT ( 'NONE',  ( 774.6312213355099630, -311.3618753856922581, 364.6798772138717482 ) ) ;
#348 = AXIS2_PLACEMENT_3D ( 'NONE', #27817, #38919, #20427 ) ;
#349 = CARTESIAN_POINT ( 'NONE',  ( 755.5713283507202505, -149.3618753856928265, -334.6858677611754729 ) ) ;
#350 = CARTESIAN_POINT ( 'NONE',  ( 759.7806653035534055, -222.9982390220561399, -324.8639956371180801 ) ) ;
#351 = CARTESIAN_POINT ( 'NONE',  ( 803.4237431249931660, -423.1800572038737300, 331.2633955100225194 ) ) ;
#352 = EDGE_CURVE ( 'NONE', #861, #2741, #13234, .T. ) ;
#353 = CARTESIAN_POINT ( 'NONE',  ( 745.4481719005789273, -147.7255117493291152, -347.5162901302853129 ) ) ;
#354 = ORIENTED_EDGE ( 'NONE', *, *, #13193, .T. ) ;
#355 = AXIS2_PLACEMENT_3D ( 'NONE', #23312, #5092, #16163 ) ;
#356 = CARTESIAN_POINT ( 'NONE',  ( 758.0580252608178853, -150.4527844766018916, -328.0187753319985404 ) ) ;
#357 = ORIENTED_EDGE ( 'NONE', *, *, #4281, .F. ) ;
#358 = CARTESIAN_POINT ( 'NONE',  ( 790.9844846989617508, -406.3726999360612808, -317.2208543904092721 ) ) ;
#359 = AXIS2_PLACEMENT_3D ( 'NONE', #31798, #9874, #27892 ) ;
#361 = CARTESIAN_POINT ( 'NONE',  ( 758.4439275373578084, -444.5545181178792973, 353.2243759319684386 ) ) ;
#360 = CARTESIAN_POINT ( 'NONE',  ( 762.3223304703356007, -127.5436935675110561, 322.3223304703362828 ) ) ;
#362 = CARTESIAN_POINT ( 'NONE',  ( 761.2382568024794409, -135.6237781080508853, 356.9571628226838129 ) ) ;
#365 = CARTESIAN_POINT ( 'NONE',  ( 745.1769319972822814, -377.8055962898682765, 346.2694204179732083 ) ) ;
#364 = CARTESIAN_POINT ( 'NONE',  ( -202.7175100919714055, 256.5000000000001137, -199.9999999999926956 ) ) ;
#363 = DIRECTION ( 'NONE',  ( 0.000000000000000000, 0.000000000000000000, 1.000000000000000000 ) ) ;
#366 = VECTOR ( 'NONE', #18473, 1000.000000000000000 ) ;
#367 = EDGE_LOOP ( 'NONE', ( #42116, #38302, #12349, #11045 ) ) ;
#368 = CARTESIAN_POINT ( 'NONE',  ( 761.4292242960306112, -377.4636090269704596, -323.2154366446414429 ) ) ;
#369 = CARTESIAN_POINT ( 'NONE',  ( 200.7583438952259485, 394.6698570112193920, -274.9999999999999432 ) ) ;
#370 = CARTESIAN_POINT ( 'NONE',  ( 755.8990559732751535, -179.4636090269710849, -365.9055244015606831 ) ) ;
#371 = CARTESIAN_POINT ( 'NONE',  ( 795.8262568251477660, -22.37269993606246743, 308.3538107759623585 ) ) ;
#373 = DIRECTION ( 'NONE',  ( 0.000000000000000000, 0.000000000000000000, 1.000000000000000000 ) ) ;
#372 = CARTESIAN_POINT ( 'NONE',  ( 799.9999999999993179, -365.3551492539851893, 18.13243251470705886 ) ) ;
#374 = CARTESIAN_POINT ( 'NONE',  ( 761.2382568024794409, -303.6237781080503169, -356.9571628226838129 ) ) ;
#375 = CARTESIAN_POINT ( 'NONE',  ( 800.2193346964447755, -450.9982390220554294, -355.1360043628815788 ) ) ;
#376 = CARTESIAN_POINT ( 'NONE',  ( 791.0478386215596629, -189.8272453906073736, -306.7653713866226326 ) ) ;
#377 = DIRECTION ( 'NONE',  ( 0.000000000000000000, -0.6594541114781790059, 0.7517448203044204691 ) ) ;
#378 = DIRECTION ( 'NONE',  ( -1.880165489482579047E-16, -1.000000000000000000, -0.000000000000000000 ) ) ;
#379 = CARTESIAN_POINT ( 'NONE',  ( 759.0159684113467620, -376.9181544815159555, 325.8855110935213020 ) ) ;
#380 = VECTOR ( 'NONE', #7221, 1000.000000000000000 ) ;
#381 = CARTESIAN_POINT ( 'NONE',  ( 766.4474001241216001, -331.0999726633342561, 307.3154664389482491 ) ) ;
#382 = MECHANICAL_DESIGN_GEOMETRIC_PRESENTATION_REPRESENTATION (  '', ( #11425 ), #4082 ) ;
#383 = CARTESIAN_POINT ( 'NONE',  ( 767.7687537140311633, -215.9073299311471317, -372.7932403749916830 ) ) ;
#384 = FACE_OUTER_BOUND ( 'NONE', #6648, .T. ) ;
#385 = DIRECTION ( 'NONE',  ( -0.000000000000000000, -0.3826834323650838976, -0.9238795325112892920 ) ) ;
#386 = CIRCLE ( 'NONE', #29134, 2.749999999999919176 ) ;
#387 = CARTESIAN_POINT ( 'NONE',  ( 788.6739635108323228, -151.6454272087892718, 373.9316612368139090 ) ) ;
#388 = CARTESIAN_POINT ( 'NONE',  ( 807.5423716828161105, -105.0783235625964096, -362.2119215644372048 ) ) ;
#389 = CARTESIAN_POINT ( 'NONE',  ( 792.2312462859673587, -131.9073299311473875, 307.2067596250082602 ) ) ;
#390 = CARTESIAN_POINT ( 'NONE',  ( 814.5518280994195948, -351.7255117493284047, -332.4837098697145734 ) ) ;
#391 = CYLINDRICAL_SURFACE ( 'NONE', #1235, 2.749999999999863665 ) ;
#392 = CARTESIAN_POINT ( 'NONE',  ( 758.7867965644027208, 16.45630643248849267, -318.7867965644036872 ) ) ;
#393 = CARTESIAN_POINT ( 'NONE',  ( 764.8639956371174549, -224.0891481129653187, 319.7806653035542013 ) ) ;
#394 = CARTESIAN_POINT ( 'NONE',  ( 790.9844846989617508, 1.627300063937458408, 317.2208543904092721 ) ) ;
#395 = CARTESIAN_POINT ( 'NONE',  ( 752.4576283171824116, -405.0783235625954148, -317.7880784355627952 ) ) ;
#396 = AXIS2_PLACEMENT_3D ( 'NONE', #5672, #19302, #1519 ) ;
#397 = CARTESIAN_POINT ( 'NONE',  ( 747.2067596250078623, -411.1800572038738437, -352.2312462859687230 ) ) ;
#398 = CARTESIAN_POINT ( 'NONE',  ( -769.9999999999992042, 205.0000000000000568, -329.9999999999999432 ) ) ;
#399 = CARTESIAN_POINT ( 'NONE',  ( 776.2433038121456548, -12.89650538077851216, 374.8207195650711014 ) ) ;
#400 = EDGE_LOOP ( 'NONE', ( #17798, #30805, #15022, #180 ) ) ;
#401 = AXIS2_PLACEMENT_3D ( 'NONE', #14674, #35902, #42831 ) ;
#402 = EDGE_CURVE ( 'NONE', #20839, #5125, #41180, .T. ) ;
#403 = CARTESIAN_POINT ( 'NONE',  ( 764.3348316497523456, -190.7146871989597798, -308.6759233522265617 ) ) ;
#404 = FACE_OUTER_BOUND ( 'NONE', #21934, .T. ) ;
#405 = CARTESIAN_POINT ( 'NONE',  ( 754.0944755984390895, -327.6237781080502600, 364.1009440267246760 ) ) ;
#406 = CARTESIAN_POINT ( 'NONE',  ( 794.9819416627830151, -108.9982390220565804, 319.9864689768909898 ) ) ;
#407 = ORIENTED_EDGE ( 'NONE', *, *, #12306, .F. ) ;
#408 = CARTESIAN_POINT ( 'NONE',  ( 771.1735550268778070, -297.1800572038740711, 316.3353852180827630 ) ) ;
#409 = EDGE_CURVE ( 'NONE', #40245, #10694, #7775, .T. ) ;
#410 = CARTESIAN_POINT ( 'NONE',  ( 748.9653473494363425, -26.63460265842045871, -356.9462024416521331 ) ) ;
#411 = CARTESIAN_POINT ( 'NONE',  ( 813.1304606946831655, -65.90732993114760063, 352.3570229623691716 ) ) ;
#412 = VECTOR ( 'NONE', #33820, 1000.000000000000000 ) ;
#413 = ORIENTED_EDGE ( 'NONE', *, *, #14771, .T. ) ;
#414 = CARTESIAN_POINT ( 'NONE',  ( 797.8822607201568644, -438.5545181178793541, -370.1134526219340160 ) ) ;
#415 = EDGE_LOOP ( 'NONE', ( #32873, #15091, #12065, #25455 ) ) ;
#416 = SHAPE_DEFINITION_REPRESENTATION ( #10394, #2289 ) ;
#417 = CARTESIAN_POINT ( 'NONE',  ( 759.9864689768902508, -26.08914811296592262, 354.9819416627836404 ) ) ;
#418 = CARTESIAN_POINT ( 'NONE',  ( 781.8018195045266339, -286.2709662947833635, -365.1927285166406705 ) ) ;
#420 = CARTESIAN_POINT ( 'NONE',  ( 746.0683387631852383, -283.4419599262321867, 331.3260364891676204 ) ) ;
#419 = CARTESIAN_POINT ( 'NONE',  ( 759.0252816721024374, -384.9982390220556567, 368.0189434323527280 ) ) ;
#421 = CARTESIAN_POINT ( 'NONE',  ( 754.0944755984390895, -87.62377810805102740, 364.1009440267246760 ) ) ;
#422 = CARTESIAN_POINT ( 'NONE',  ( 763.0428371773158460, -275.4636090269708575, -358.7617431975195359 ) ) ;
#423 = CARTESIAN_POINT ( 'NONE',  ( 804.9363028652555840, -256.2709662947834204, -338.2165204200192079 ) ) ;
#424 = CARTESIAN_POINT ( 'NONE',  ( 454.7528517110262101, 239.9999999999999716, -122.7905160835442615 ) ) ;
#425 = CARTESIAN_POINT ( 'NONE',  ( 781.7834795799800531, -130.8164208402383224, -315.0636971347436202 ) ) ;
#426 = EDGE_CURVE ( 'NONE', #13538, #14856, #40502, .T. ) ;
#427 = DIRECTION ( 'NONE',  ( 0.000000000000000000, 0.000000000000000000, 1.000000000000000000 ) ) ;
#428 = CARTESIAN_POINT ( 'NONE',  ( 782.5225473063381969, -406.2709662947829088, 375.2698199232970637 ) ) ;
#430 = CARTESIAN_POINT ( 'NONE',  ( 792.3126160409814247, -458.0040092590086260, 368.0749526239440570 ) ) ;
#429 = CARTESIAN_POINT ( 'NONE',  ( 762.3515768340985232, 20.87080523294372014, 315.3598267498177847 ) ) ;
#431 = EDGE_CURVE ( 'NONE', #22786, #36028, #26937, .T. ) ;
#432 = CARTESIAN_POINT ( 'NONE',  ( 745.1792804349281596, -86.19088175424408860, -343.7566961878542884 ) ) ;
#433 = CARTESIAN_POINT ( 'NONE',  ( -78.83651009197140525, 240.0000000000000568, -199.9999999999936051 ) ) ;
#434 = CYLINDRICAL_SURFACE ( 'NONE', #9840, 10.00000000000000888 ) ;
#435 = AXIS2_PLACEMENT_3D ( 'NONE', #25066, #43082, #39180 ) ;
#436 = CARTESIAN_POINT ( 'NONE',  ( 772.4468031744293057, -273.8272453906071746, 363.8651313633793620 ) ) ;
#437 = CARTESIAN_POINT ( 'NONE',  ( 805.1927285166397041, -136.8164208402382371, 341.8018195045277707 ) ) ;
#438 = ORIENTED_EDGE ( 'NONE', *, *, #28628, .T. ) ;
#439 = CARTESIAN_POINT ( 'NONE',  ( 804.1105419155481968, -51.82724539060782121, -347.6308680596136469 ) ) ;
#440 = CARTESIAN_POINT ( 'NONE',  ( 763.2262854647970016, -104.6346026584202207, -309.2812353651462445 ) ) ;
#441 = CARTESIAN_POINT ( 'NONE',  ( 798.7617431975189675, -315.6237781080503169, 323.0428371773161871 ) ) ;
#442 = CARTESIAN_POINT ( 'NONE',  ( -852.7175100919713486, 256.5000000000002274, -199.9999999999881481 ) ) ;
#443 = CARTESIAN_POINT ( 'NONE',  ( 814.2805881961230625, -25.64542720878973014, 331.2368401574024119 ) ) ;
#444 = CARTESIAN_POINT ( 'NONE',  ( 772.4837098697144029, -215.3618753856925423, 374.5518280994205611 ) ) ;
#445 = CARTESIAN_POINT ( 'NONE',  ( 771.2633955100217236, -71.90732993114760063, 363.4237431249939618 ) ) ;
#446 = DIRECTION ( 'NONE',  ( -0.000000000000000000, 1.000000000000000000, -0.000000000000000000 ) ) ;
#447 = CARTESIAN_POINT ( 'NONE',  ( 748.3538107759620743, -304.7146871989594388, -355.8262568251490165 ) ) ;
#448 = VECTOR ( 'NONE', #36830, 999.9999999999998863 ) ;
#449 = ADVANCED_FACE ( 'NONE', ( #27988 ), #38617, .F. ) ;
#450 = CARTESIAN_POINT ( 'NONE',  ( 778.7629533639073998, -440.7363362996975980, 375.0009284576466371 ) ) ;
#451 = CARTESIAN_POINT ( 'NONE',  ( 801.1904061080336987, -308.0891481129650629, -368.3070685750235498 ) ) ;
#452 = CARTESIAN_POINT ( 'NONE',  ( -2.220446049250310809E-13, 479.9999999999994884, 0.000000000000000000 ) ) ;
#453 = CARTESIAN_POINT ( 'NONE',  ( 761.2382568024794409, -375.6237781080501463, 356.9571628226838129 ) ) ;
#454 = VECTOR ( 'NONE', #45378, 1000.000000000000114 ) ;
#455 = CARTESIAN_POINT ( 'NONE',  ( 792.2312462859673587, -59.90732993114762905, 307.2067596250082602 ) ) ;
#456 = CARTESIAN_POINT ( 'NONE',  ( 774.6858677611749044, -393.7255117493283478, -315.5713283507209894 ) ) ;
#457 = ADVANCED_FACE ( 'NONE', ( #28210 ), #41866, .F. ) ;
#458 = CARTESIAN_POINT ( 'NONE',  ( 805.1016975059191054, -54.89650538077837183, 343.0745993439771837 ) ) ;
#459 = CARTESIAN_POINT ( 'NONE',  ( 791.1614460488616487, -83.26014174441466764, -373.5763878283158874 ) ) ;
#460 = CARTESIAN_POINT ( 'NONE',  ( 815.0009284576459549, -222.3510508353233206, 338.7629533639073429 ) ) ;
#461 = CARTESIAN_POINT ( 'NONE',  ( 758.0580252608178853, -6.452784476602343666, 328.0187753319985404 ) ) ;
#462 = VECTOR ( 'NONE', #12893, 1000.000000000000000 ) ;
#463 = VERTEX_POINT ( 'NONE', #38172 ) ;
#464 = CARTESIAN_POINT ( 'NONE',  ( 779.4709603349208464, -192.3510508353233774, -314.7162404726379918 ) ) ;
#465 = CARTESIAN_POINT ( 'NONE',  ( 785.3141322388236176, -189.7255117493290300, 364.4286716492789537 ) ) ;
#466 = VECTOR ( 'NONE', #30929, 1000.000000000000000 ) ;
#467 = ADVANCED_FACE ( 'NONE', ( #17609 ), #13685, .F. ) ;
#468 = CARTESIAN_POINT ( 'NONE',  ( 813.9316612368132837, -31.44195992623299674, -348.6739635108323228 ) ) ;
#469 = CARTESIAN_POINT ( 'NONE',  ( 804.4286716492782716, -329.3618753856922581, 345.3141322388244703 ) ) ;
#470 = CARTESIAN_POINT ( 'NONE',  ( 831.1634899080286232, 259.9999999999998863, -199.9999999999999432 ) ) ;
#471 = CARTESIAN_POINT ( 'NONE',  ( 758.9356612065449781, 18.10977687916123813, 318.6379319222613731 ) ) ;
#472 = ORIENTED_EDGE ( 'NONE', *, *, #31485, .F. ) ;
#473 = CARTESIAN_POINT ( 'NONE',  ( 804.1601925771018387, -55.44195992623293989, 346.5483106153029098 ) ) ;
#474 = CARTESIAN_POINT ( 'NONE',  ( 754.3581564841646241, -353.4636090269705733, -316.1443688327762516 ) ) ;
#475 = CARTESIAN_POINT ( 'NONE',  ( 808.0189434323515343, -302.0891481129650629, 319.0252816721025511 ) ) ;
#476 = CARTESIAN_POINT ( 'NONE',  ( 754.0944755984390895, 8.376221891948691933, 364.1009440267246760 ) ) ;
#477 = CARTESIAN_POINT ( 'NONE',  ( 786.5483106153019435, -175.6454272087892718, -364.1601925771022366 ) ) ;
#478 = CARTESIAN_POINT ( 'NONE',  ( 759.9864689768902508, -146.0891481129655176, -354.9819416627836404 ) ) ;
#479 = CARTESIAN_POINT ( 'NONE',  ( 755.3201227861273992, -363.7255117493284615, -345.3687786644892981 ) ) ;
#480 = EDGE_LOOP ( 'NONE', ( #309, #39907, #31918, #2309 ) ) ;
#481 = CARTESIAN_POINT ( 'NONE',  ( 770.0799878456142551, 10.01258552831232329, -362.9823548866085616 ) ) ;
#482 = CARTESIAN_POINT ( 'NONE',  ( 801.6550554848130332, -456.5036469134198001, 360.7619500998734452 ) ) ;
#483 = CARTESIAN_POINT ( 'NONE',  ( 770.0799878456142551, -349.9874144716865771, 362.9823548866085616 ) ) ;
#484 = CIRCLE ( 'NONE', #5652, 30.00000000000002842 ) ;
#485 = DIRECTION ( 'NONE',  ( -0.000000000000000000, 1.000000000000000000, -0.000000000000000000 ) ) ;
#486 = CARTESIAN_POINT ( 'NONE',  ( 804.1105419155481968, -171.8272453906074304, 347.6308680596136469 ) ) ;
#487 = CARTESIAN_POINT ( 'NONE',  ( 800.0135310231082713, -38.08914811296587999, 325.0180583372163028 ) ) ;
#488 = ORIENTED_EDGE ( 'NONE', *, *, #35724, .T. ) ;
#489 = CARTESIAN_POINT ( 'NONE',  ( 747.6481478633932056, -373.0999726633340856, -353.4146539503763620 ) ) ;
#490 = AXIS2_PLACEMENT_3D ( 'NONE', #32758, #32530, #29065 ) ;
#491 = CARTESIAN_POINT ( 'NONE',  ( 796.9462024416508257, 11.54721552339759860, -308.9653473494370246 ) ) ;
#492 = CARTESIAN_POINT ( 'NONE',  ( 746.4236121716829757, -279.8272453906071746, 328.8385539511384650 ) ) ;
#493 = CARTESIAN_POINT ( 'NONE',  ( 790.8726784830453198, -370.7146871989592114, 362.5472867521010585 ) ) ;
#494 = CARTESIAN_POINT ( 'NONE',  ( 756.1348686366196716, -185.2601417444143692, 347.5531968255698416 ) ) ;
#495 = CARTESIAN_POINT ( 'NONE',  ( 800.0135310231082713, -350.0891481129648923, -325.0180583372163028 ) ) ;
#496 = CARTESIAN_POINT ( 'NONE',  ( 804.9363028652555840, 7.729033705215793582, 338.2165204200192079 ) ) ;
#497 = DIRECTION ( 'NONE',  ( 0.000000000000000000, 0.000000000000000000, -1.000000000000000000 ) ) ;
#498 = CARTESIAN_POINT ( 'NONE',  ( 755.8894580844503253, -231.8272453906072315, -332.3691319403863531 ) ) ;
#499 = CARTESIAN_POINT ( 'NONE',  ( 746.8695393053150156, -5.907329931147798696, 327.6429770376306010 ) ) ;
#500 = CARTESIAN_POINT ( 'NONE',  ( 746.8695393053150156, -101.9073299311474727, 327.6429770376306010 ) ) ;
#501 = CARTESIAN_POINT ( 'NONE',  ( -39.63011601220123481, -563.3203001761230553, -342.3463313526983143 ) ) ;
#502 = CARTESIAN_POINT ( 'NONE',  ( 759.0252816721024374, -432.9982390220555999, -368.0189434323527280 ) ) ;
#503 = CARTESIAN_POINT ( 'NONE',  ( -773.4999999999993179, -512.9681489794448908, -339.9999999999999432 ) ) ;
#504 = CARTESIAN_POINT ( 'NONE',  ( 813.5763878283155464, -363.8272453906068336, 351.1614460488615350 ) ) ;
#505 = CYLINDRICAL_SURFACE ( 'NONE', #16137, 30.00000000000008171 ) ;
#506 = CARTESIAN_POINT ( 'NONE',  ( 744.7301800767019131, -340.8164208402376971, 337.4774526936615757 ) ) ;
#507 = CARTESIAN_POINT ( 'NONE',  ( 777.5031285880264704, -70.81642084023850714, -374.9108240113588408 ) ) ;
#508 = CARTESIAN_POINT ( 'NONE',  ( 758.0580252608178853, -294.4527844766013800, -328.0187753319985404 ) ) ;
#509 = DIRECTION ( 'NONE',  ( 0.000000000000000000, -1.000000000000000000, 0.000000000000000000 ) ) ;
#510 = CARTESIAN_POINT ( 'NONE',  ( 764.8639956371174549, -440.0891481129644944, 319.7806653035542013 ) ) ;
#511 = CARTESIAN_POINT ( 'NONE',  ( 772.4468031744293057, -177.8272453906074304, 363.8651313633793620 ) ) ;
#512 = CARTESIAN_POINT ( 'NONE',  ( 797.8822607201568644, -78.55451811788046257, -370.1134526219340160 ) ) ;
#513 = CARTESIAN_POINT ( 'NONE',  ( 770.0799878456142551, -85.98741447168738716, -362.9823548866085616 ) ) ;
#514 = CARTESIAN_POINT ( 'NONE',  ( 745.1769319972822814, -89.80559628986918597, 346.2694204179732083 ) ) ;
#515 = CARTESIAN_POINT ( 'NONE',  ( 781.8018195045267476, -406.2709662947828519, 365.1927285166407273 ) ) ;
#516 = VECTOR ( 'NONE', #12520, 1000.000000000000000 ) ;
#517 = CARTESIAN_POINT ( 'NONE',  ( 754.8072714833581358, -4.816420840238714085, -338.1981804954720587 ) ) ;
#518 = VERTEX_POINT ( 'NONE', #16922 ) ;
#519 = CARTESIAN_POINT ( 'NONE',  ( 768.0187753319979720, -80.63460265842029173, -318.0580252608186242 ) ) ;
#520 = VECTOR ( 'NONE', #16329, 1000.000000000000000 ) ;
#521 = EDGE_CURVE ( 'NONE', #12460, #20164, #17350, .T. ) ;
#522 = CARTESIAN_POINT ( 'NONE',  ( 775.9200461376533440, -407.8055962898681628, -315.3028492785443291 ) ) ;
#524 = CARTESIAN_POINT ( 'NONE',  ( 762.3223304703356007, -223.5436935675107577, 322.3223304703362828 ) ) ;
#523 = CARTESIAN_POINT ( 'NONE',  ( 759.9864689768902508, -218.0891481129653187, 354.9819416627836404 ) ) ;
#525 = CARTESIAN_POINT ( 'NONE',  ( 812.6845335610512393, -415.9874144716862361, -353.5525998758768651 ) ) ;
#526 = CARTESIAN_POINT ( 'NONE',  ( 786.4999999999993179, -494.6608068873671300, -357.6536686473015720 ) ) ;
#527 = ORIENTED_EDGE ( 'NONE', *, *, #24678, .F. ) ;
#528 = CARTESIAN_POINT ( 'NONE',  ( 757.8323909638827445, -410.6346026584191122, 352.1044303154654358 ) ) ;
#529 = CIRCLE ( 'NONE', #15277, 10.00000000000000888 ) ;
#530 = ORIENTED_EDGE ( 'NONE', *, *, #3202, .F. ) ;
#531 = AXIS2_PLACEMENT_3D ( 'NONE', #37284, #44217, #1707 ) ;
#532 = CARTESIAN_POINT ( 'NONE',  ( 812.7932403749906598, -255.1800572038742700, -327.7687537140311633 ) ) ;
#533 = CARTESIAN_POINT ( 'NONE',  ( 787.4397851343537695, -165.7255117493291152, 374.2001403089903988 ) ) ;
#534 = CARTESIAN_POINT ( 'NONE',  ( 755.3028492785439312, -255.2817908451526705, 335.9200461376539693 ) ) ;
#535 = EDGE_LOOP ( 'NONE', ( #2161, #41639, #39801, #23830 ) ) ;
#536 = CARTESIAN_POINT ( 'NONE',  ( 760.7433823573367135, -60.00906357242598688, -355.9930595647440441 ) ) ;
#537 = CARTESIAN_POINT ( 'NONE',  ( 793.4146539503750546, -193.9874144716870319, 307.6481478633938877 ) ) ;
#538 = CARTESIAN_POINT ( 'NONE',  ( 797.6776695296629214, -235.5436935675107293, -357.6776695296636603 ) ) ;
#539 = ORIENTED_EDGE ( 'NONE', *, *, #26142, .F. ) ;
#540 = CARTESIAN_POINT ( 'NONE',  ( 800.2193346964447755, -354.9982390220557704, -355.1360043628815788 ) ) ;
#541 = CARTESIAN_POINT ( 'NONE',  ( 765.0180583372156207, -48.99823902205675807, -360.0135310231089534 ) ) ;
#542 = CARTESIAN_POINT ( 'NONE',  ( 783.0433043558608688, -240.8965053807777963, 315.1538015810313027 ) ) ;
#543 = LINE ( 'NONE', #39589, #26981 ) ;
#544 = CARTESIAN_POINT ( 'NONE',  ( 914.9999999999992042, 56.60618624968562074, -350.0000000000000000 ) ) ;
#545 = ORIENTED_EDGE ( 'NONE', *, *, #45289, .F. ) ;
#546 = CARTESIAN_POINT ( 'NONE',  ( 785.3687786644884454, -35.36187538569316047, -315.3201227861279676 ) ) ;
#547 = CARTESIAN_POINT ( 'NONE',  ( 311.1634899080286232, 260.0000000000000000, -199.9999999999963336 ) ) ;
#548 = DIRECTION ( 'NONE',  ( 0.000000000000000000, 0.000000000000000000, -1.000000000000000000 ) ) ;
#549 = ORIENTED_EDGE ( 'NONE', *, *, #40552, .F. ) ;
#550 = CARTESIAN_POINT ( 'NONE',  ( 786.2694204179717872, -285.2817908451526137, -305.1769319972829067 ) ) ;
#551 = CARTESIAN_POINT ( 'NONE',  ( 748.6759233522253680, -184.3726999360619629, 324.3348316497537098 ) ) ;
#552 = VECTOR ( 'NONE', #9585, 1000.000000000000000 ) ;
#554 = CARTESIAN_POINT ( 'NONE',  ( 804.4286716492782716, -257.3618753856924286, -345.3141322388244703 ) ) ;
#553 = LINE ( 'NONE', #7485, #44537 ) ;
#555 = DIRECTION ( 'NONE',  ( -1.000000000000000000, 0.000000000000000000, 0.000000000000000000 ) ) ;
#556 = CARTESIAN_POINT ( 'NONE',  ( 796.9571628226829034, -119.4636090269712554, -321.2382568024804641 ) ) ;
#557 = CARTESIAN_POINT ( 'NONE',  ( 745.5313806188320314, -375.2817908451523294, 333.7943932421247268 ) ) ;
#558 = FACE_BOUND ( 'NONE', #9290, .T. ) ;
#559 = CARTESIAN_POINT ( 'NONE',  ( 796.7737145352015204, -308.6346026584195670, -370.7187646348536987 ) ) ;
#560 = CARTESIAN_POINT ( 'NONE',  ( 989.9999999999992042, 469.9999999999999432, 350.0000000000000000 ) ) ;
#561 = CARTESIAN_POINT ( 'NONE',  ( 800.2193346964447755, 5.001760977943074948, 355.1360043628815788 ) ) ;
#562 = VECTOR ( 'NONE', #15359, 1000.000000000000000 ) ;
#563 = CARTESIAN_POINT ( 'NONE',  ( 778.7629533639073998, -248.7363362996981380, 375.0009284576466371 ) ) ;
#564 = CARTESIAN_POINT ( 'NONE',  ( 808.7758568127978833, -196.1692326535052473, -320.0363995740631822 ) ) ;
#565 = CARTESIAN_POINT ( 'NONE',  ( 782.5225473063381969, -214.2709662947834488, 375.2698199232970637 ) ) ;
#566 = CARTESIAN_POINT ( 'NONE',  ( 808.3070685750230950, -450.9982390220554294, -361.1904061080339261 ) ) ;
#567 = CARTESIAN_POINT ( 'NONE',  ( 441.1634899080286232, 256.4999999999999432, -206.1189999999972144 ) ) ;
#568 = CARTESIAN_POINT ( 'NONE',  ( 805.1927285166397041, -328.8164208402375834, 341.8018195045277707 ) ) ;
#569 = EDGE_CURVE ( 'NONE', #23226, #12347, #33564, .T. ) ;
#570 = CARTESIAN_POINT ( 'NONE',  ( 760.7433823573367135, -84.00906357242590161, 355.9930595647440441 ) ) ;
#571 = CARTESIAN_POINT ( 'NONE',  ( 804.6971507214547046, -75.28179084515321051, 344.0799538623459739 ) ) ;
#572 = CARTESIAN_POINT ( 'NONE',  ( 763.2154366446407039, 2.376221891948710585, -321.4292242960311228 ) ) ;
#573 = CARTESIAN_POINT ( 'NONE',  ( -773.4999999999993179, -365.3551492539851893, -28.13243251470704109 ) ) ;
#574 = CARTESIAN_POINT ( 'NONE',  ( 799.9999999999993179, -512.9681489794448908, -370.0000000000000000 ) ) ;
#576 = CARTESIAN_POINT ( 'NONE',  ( 756.5762568750052424, -363.1800572038739006, 348.7366044899774238 ) ) ;
#575 = CARTESIAN_POINT ( 'NONE',  ( 766.7756240680305382, -158.5328690171417065, 361.5560724626415663 ) ) ;
#577 = VERTEX_POINT ( 'NONE', #10432 ) ;
#578 = CARTESIAN_POINT ( 'NONE',  ( 779.4709603349208464, -288.3510508353231216, -314.7162404726379918 ) ) ;
#579 = CARTESIAN_POINT ( 'NONE',  ( 756.3353852180819104, -125.9073299311474159, 331.1735550268788302 ) ) ;
#580 = CARTESIAN_POINT ( 'NONE',  ( 815.0009284576459549, -294.3510508353230648, -338.7629533639073429 ) ) ;
#581 = DIRECTION ( 'NONE',  ( 1.000000000000000000, -0.000000000000000000, 0.000000000000000000 ) ) ;
#582 = CARTESIAN_POINT ( 'NONE',  ( 752.4576283171824116, -429.0783235625953580, 317.7880784355627952 ) ) ;
#583 = ORIENTED_EDGE ( 'NONE', *, *, #12485, .T. ) ;
#584 = CARTESIAN_POINT ( 'NONE',  ( 801.9419747391806368, -330.4527844766013231, 351.9812246680014027 ) ) ;
#585 = CARTESIAN_POINT ( 'NONE',  ( 758.6633372737375112, -68.53286901714197654, -326.9102291470432533 ) ) ;
#586 = CARTESIAN_POINT ( 'NONE',  ( 803.4237431249931660, -159.1800572038746111, -331.2633955100225194 ) ) ;
#587 = CARTESIAN_POINT ( 'NONE',  ( 781.7834795799800531, -202.8164208402380950, -315.0636971347436202 ) ) ;
#588 = CARTESIAN_POINT ( 'NONE',  ( 762.1405469898971887, -433.5436935675099903, 357.8594530101015607 ) ) ;
#589 = CARTESIAN_POINT ( 'NONE',  ( 815.2698199232961542, -136.8164208402382371, -342.5225473063383106 ) ) ;
#590 = ORIENTED_EDGE ( 'NONE', *, *, #29552, .T. ) ;
#591 = CARTESIAN_POINT ( 'NONE',  ( 771.1735550268780344, -153.1800572038746111, -316.3353852180828198 ) ) ;
#592 = ORIENTED_EDGE ( 'NONE', *, *, #31485, .T. ) ;
#593 = VECTOR ( 'NONE', #7682, 1000.000000000000000 ) ;
#594 = CARTESIAN_POINT ( 'NONE',  ( 804.6971507214547046, -387.2817908451522726, -344.0799538623459739 ) ) ;
#595 = CARTESIAN_POINT ( 'NONE',  ( 785.3687786644884454, 12.63812461430668321, 315.3201227861279676 ) ) ;
#596 = CARTESIAN_POINT ( 'NONE',  ( 782.4968714119720516, -226.8164208402380098, 305.0891759886411023 ) ) ;
#597 = CARTESIAN_POINT ( 'NONE',  ( 779.4709603349208464, -120.3510508353236048, 314.7162404726379918 ) ) ;
#600 = CARTESIAN_POINT ( 'NONE',  ( 746.0683387631852383, -403.4419599262317888, 331.3260364891676204 ) ) ;
#599 = LINE ( 'NONE', #35460, #21044 ) ;
#598 = CARTESIAN_POINT ( 'NONE',  ( -786.4999999999993179, -544.8427095258973623, -350.0000000000000000 ) ) ;
#601 = VERTEX_POINT ( 'NONE', #17377 ) ;
#602 = CARTESIAN_POINT ( 'NONE',  ( 805.2837595273609850, -386.7363362996977116, -340.5290396650784714 ) ) ;
#603 = CARTESIAN_POINT ( 'NONE',  ( 775.4999999999993179, 22.32581219114657856, 895.6886905569881492 ) ) ;
#604 = CARTESIAN_POINT ( 'NONE',  ( 749.5768839229115201, -180.5545181178801499, -358.0661480581553064 ) ) ;
#605 = CARTESIAN_POINT ( 'NONE',  ( 805.6418435158337843, -29.46360902697153250, 363.8556311672236916 ) ) ;
#607 = CARTESIAN_POINT ( 'NONE',  ( 919.9999999999993179, 219.9999999999998863, -360.0000000000000000 ) ) ;
#606 = DIRECTION ( 'NONE',  ( -1.000000000000000000, -0.000000000000000000, 0.000000000000000000 ) ) ;
#608 = CARTESIAN_POINT ( 'NONE',  ( 802.7791456095903868, -340.7146871989592114, -329.0155153010375102 ) ) ;
#609 = CARTESIAN_POINT ( 'NONE',  ( 754.8072714833581358, -436.8164208402372992, -338.1981804954720587 ) ) ;
#610 = CARTESIAN_POINT ( 'NONE',  ( 802.2119215644370342, -174.0090635724256742, -367.5423716828165084 ) ) ;
#611 = CARTESIAN_POINT ( 'NONE',  ( 775.4999999999993179, -365.3551492539851893, -18.13243251470705886 ) ) ;
#612 = FACE_OUTER_BOUND ( 'NONE', #6643, .T. ) ;
#613 = CARTESIAN_POINT ( 'NONE',  ( 784.1219089521767955, -381.2817908451523294, 315.0488828828318333 ) ) ;
#614 = CARTESIAN_POINT ( 'NONE',  ( 755.8990559732751535, -347.4636090269705733, 365.9055244015606831 ) ) ;
#615 = CARTESIAN_POINT ( 'NONE',  ( 813.1304606946831655, -209.9073299311471317, -352.3570229623691716 ) ) ;
#616 = LINE ( 'NONE', #11017, #6169 ) ;
#617 = CARTESIAN_POINT ( 'NONE',  ( 804.9363028652555840, -16.27096629478413092, -338.2165204200192079 ) ) ;
#618 = CARTESIAN_POINT ( 'NONE',  ( 755.8990559732751535, -131.4636090269711985, 365.9055244015606831 ) ) ;
#619 = CARTESIAN_POINT ( 'NONE',  ( 744.8212110874229666, -90.89650538077827946, -336.2046728542121627 ) ) ;
#620 = CARTESIAN_POINT ( 'NONE',  ( 813.1304606946830518, -113.9073299311474301, 352.3570229623690580 ) ) ;
#621 = CARTESIAN_POINT ( 'NONE',  ( 792.2312462859673587, -323.9073299311468190, -307.2067596250082602 ) ) ;
#622 = ADVANCED_FACE ( 'NONE', ( #10912, #13916, #35146, #24509, #31678, #3282, #39091, #20817, #34470, #34916, #6977, #31002, #31460, #31226, #3523 ), #24054, .F. ) ;
#623 = DIRECTION ( 'NONE',  ( -0.000000000000000000, -0.000000000000000000, 1.000000000000000000 ) ) ;
#624 = CARTESIAN_POINT ( 'NONE',  ( 999.9999999999992042, 239.9999999999998863, -209.9999999999999716 ) ) ;
#625 = CARTESIAN_POINT ( 'NONE',  ( 771.1735550268778070, -225.1800572038743269, 316.3353852180827630 ) ) ;
#626 = CARTESIAN_POINT ( 'NONE',  ( 776.2046728542105711, -452.1908817542428665, 304.8212110874238761 ) ) ;
#627 = CARTESIAN_POINT ( 'NONE',  ( 815.1787889125755555, -414.8965053807771710, -343.7953271457877804 ) ) ;
#628 = AXIS2_PLACEMENT_3D ( 'NONE', #31793, #14497, #10794 ) ;
#629 = CARTESIAN_POINT ( 'NONE',  ( 800.9747183278959710, -420.9982390220555999, -311.9810565676471583 ) ) ;
#630 = PLANE ( 'NONE',  #9977 ) ;
#631 = CARTESIAN_POINT ( 'NONE',  ( 766.5853460496234675, 10.01258552831232329, 372.3518521366060554 ) ) ;
#632 = ORIENTED_EDGE ( 'NONE', *, *, #43023, .F. ) ;
#633 = CARTESIAN_POINT ( 'NONE',  ( 764.8639956371174549, -32.08914811296588709, 319.7806653035542013 ) ) ;
#634 = CARTESIAN_POINT ( 'NONE',  ( 746.0683387631852383, -187.4419599262325278, -331.3260364891676204 ) ) ;
#635 = CARTESIAN_POINT ( 'NONE',  ( 773.7943932421234194, -311.8055962898685038, 305.5313806188329409 ) ) ;
#636 = CARTESIAN_POINT ( 'NONE',  ( 755.0636971347428243, -172.2709662947836478, 341.7834795799807353 ) ) ;
#637 = VERTEX_POINT ( 'NONE', #20374 ) ;
#638 = CARTESIAN_POINT ( 'NONE',  ( 756.5762568750052424, -291.1800572038741848, 348.7366044899774238 ) ) ;
#639 = CARTESIAN_POINT ( 'NONE',  ( 815.2698199232961542, -40.81642084023859951, -342.5225473063383106 ) ) ;
#640 = EDGE_CURVE ( 'NONE', #10075, #33702, #9985, .T. ) ;
#641 = CARTESIAN_POINT ( 'NONE',  ( 751.6929314249750860, -78.99823902205665149, 318.8095938919659034 ) ) ;
#642 = ORIENTED_EDGE ( 'NONE', *, *, #31723, .T. ) ;
#643 = CARTESIAN_POINT ( 'NONE',  ( 745.7194118038753459, -445.6454272087883055, -348.7631598425976449 ) ) ;
#644 = ORIENTED_EDGE ( 'NONE', *, *, #14195, .F. ) ;
#645 = SHAPE_DEFINITION_REPRESENTATION ( #14496, #4721 ) ;
#647 = CARTESIAN_POINT ( 'NONE',  ( 758.4439275373578084, -324.5545181178796952, 353.2243759319684386 ) ) ;
#646 = CARTESIAN_POINT ( 'NONE',  ( 755.0636971347428243, -76.27096629478394618, 341.7834795799807353 ) ) ;
#648 = CARTESIAN_POINT ( 'NONE',  ( 791.9812246680005501, -284.6346026584196807, -361.9419747391813189 ) ) ;
#650 = CARTESIAN_POINT ( 'NONE',  ( 778.7502325331095108, -288.3510508353231216, 304.6391490659818828 ) ) ;
#649 = CARTESIAN_POINT ( 'NONE',  ( 746.8695393053151292, -389.9073299311465917, 327.6429770376306578 ) ) ;
#651 = CARTESIAN_POINT ( 'NONE',  ( 803.8556311672234642, -81.62377810805104161, 365.6418435158340117 ) ) ;
#652 = CARTESIAN_POINT ( 'NONE',  ( 796.9571628226829034, -287.4636090269708575, -321.2382568024804641 ) ) ;
#653 = CARTESIAN_POINT ( 'NONE',  ( 788.7366044899766848, -299.9073299311468759, -316.5762568750059813 ) ) ;
#654 = DIRECTION ( 'NONE',  ( -0.000000000000000000, 1.000000000000000000, -0.000000000000000000 ) ) ;
#655 = CARTESIAN_POINT ( 'NONE',  ( 803.6646147819161570, -113.9073299311474301, -348.8264449731210561 ) ) ;
#656 = FACE_OUTER_BOUND ( 'NONE', #25655, .T. ) ;
#657 = EDGE_LOOP ( 'NONE', ( #6082, #28881, #4838, #12896, #5628, #10326, #36542, #16472, #9881, #21547, #42805 ) ) ;
#658 = AXIS2_PLACEMENT_3D ( 'NONE', #4761, #18865, #32956 ) ;
#659 = CARTESIAN_POINT ( 'NONE',  ( 800.9747183278959710, -396.9982390220556567, 311.9810565676471583 ) ) ;
#661 = DIRECTION ( 'NONE',  ( -1.000000000000000000, -0.000000000000000000, -0.000000000000000000 ) ) ;
#660 = CARTESIAN_POINT ( 'NONE',  ( 989.9999999999992042, 62.79977829742938411, -207.3621835540872951 ) ) ;
#662 = CARTESIAN_POINT ( 'NONE',  ( 754.3581564841646241, -89.46360902697134065, -316.1443688327762516 ) ) ;
#663 = CARTESIAN_POINT ( 'NONE',  ( -208.8365100919714052, 256.5000000000001137, -206.1189999999926954 ) ) ;
#664 = DIRECTION ( 'NONE',  ( -0.000000000000000000, 1.000000000000000000, -0.000000000000000000 ) ) ;
#665 = EDGE_CURVE ( 'NONE', #10985, #9763, #35048, .T. ) ;
#666 = CARTESIAN_POINT ( 'NONE',  ( 796.9571628226829034, -263.4636090269708006, 321.2382568024804641 ) ) ;
#667 = CARTESIAN_POINT ( 'NONE',  ( 804.4286716492782716, -161.3618753856927697, 345.3141322388244703 ) ) ;
#668 = ORIENTED_EDGE ( 'NONE', *, *, #5793, .T. ) ;
#669 = CARTESIAN_POINT ( 'NONE',  ( 769.0155153010367712, -58.37269993606236085, -362.7791456095907279 ) ) ;
#670 = CARTESIAN_POINT ( 'NONE',  ( 782.5225473063383106, -94.27096629478387513, -375.2698199232970637 ) ) ;
#671 = CARTESIAN_POINT ( 'NONE',  ( 787.6308680596127942, -323.2601417444138860, 364.1105419155492768 ) ) ;
#672 = CARTESIAN_POINT ( 'NONE',  ( 797.6776695296629214, -451.5436935675099903, -357.6776695296636603 ) ) ;
#673 = CARTESIAN_POINT ( 'NONE',  ( 783.7953271457878373, -56.19088175424417386, 375.1787889125761239 ) ) ;
#674 = CARTESIAN_POINT ( 'NONE',  ( 808.3070685750230950, -234.9982390220561683, -361.1904061080339261 ) ) ;
#675 = ADVANCED_FACE ( 'NONE', ( #20599 ), #14394, .F. ) ;
#676 = CARTESIAN_POINT ( 'NONE',  ( 811.0346526505616112, -206.6346026584198512, 323.0537975583477532 ) ) ;
#677 = CARTESIAN_POINT ( 'NONE',  ( 785.3141322388236176, -117.7255117493292715, 364.4286716492789537 ) ) ;
#678 = CARTESIAN_POINT ( 'NONE',  ( 441.1634899080286232, 259.9999999999999432, -199.9999999999972431 ) ) ;
#679 = CARTESIAN_POINT ( 'NONE',  ( 811.6461892240364477, -316.7146871989593819, -324.1737431748509835 ) ) ;
#680 = CARTESIAN_POINT ( 'NONE',  ( 771.3260364891663130, -451.6454272087884192, 306.0683387631859773 ) ) ;
#681 = CARTESIAN_POINT ( 'NONE',  ( 763.2262854647970016, -320.6346026584195670, -309.2812353651462445 ) ) ;
#682 = DIRECTION ( 'NONE',  ( -0.000000000000000000, 1.000000000000000000, -0.000000000000000000 ) ) ;
#683 = CARTESIAN_POINT ( 'NONE',  ( 760.5453621957607311, -357.0783235625956422, 323.8424801807151425 ) ) ;
#684 = CARTESIAN_POINT ( 'NONE',  ( 758.8095938919644823, -56.08914811296581604, 311.6929314249762797 ) ) ;
#685 = CARTESIAN_POINT ( 'NONE',  ( 759.9864689768902508, -434.0891481129646081, -354.9819416627836404 ) ) ;
#686 = CARTESIAN_POINT ( 'NONE',  ( 754.8983024940795303, -42.89650538077842157, 336.9254006560228163 ) ) ;
#687 = CARTESIAN_POINT ( 'NONE',  ( 754.8072714833581358, -196.8164208402380950, -338.1981804954720587 ) ) ;
#688 = CARTESIAN_POINT ( 'NONE',  ( 813.9316612368132837, -79.44195992623286884, -348.6739635108323228 ) ) ;
#689 = EDGE_CURVE ( 'NONE', #12562, #45491, #45323, .T. ) ;
#690 = CARTESIAN_POINT ( 'NONE',  ( 815.0009284576459549, -198.3510508353234059, 338.7629533639073429 ) ) ;
#691 = CARTESIAN_POINT ( 'NONE',  ( 797.6776695296629214, -67.54369356751125508, 357.6776695296636603 ) ) ;
#692 = CIRCLE ( 'NONE', #18407, 30.00000000000008171 ) ;
#693 = EDGE_CURVE ( 'NONE', #4054, #5516, #21293, .T. ) ;
#694 = ORIENTED_EDGE ( 'NONE', *, *, #17918, .T. ) ;
#695 = CARTESIAN_POINT ( 'NONE',  ( 758.6633372737375112, -236.5328690171414792, -326.9102291470432533 ) ) ;
#696 = CARTESIAN_POINT ( 'NONE',  ( 804.9363028652555840, -208.2709662947835341, 338.2165204200192079 ) ) ;
#697 = CARTESIAN_POINT ( 'NONE',  ( 813.2346286133761168, -29.26014174441482751, -328.9521613784389160 ) ) ;
#698 = CARTESIAN_POINT ( 'NONE',  ( 765.0180583372156207, -312.9982390220559409, 360.0135310231089534 ) ) ;
#699 = CARTESIAN_POINT ( 'NONE',  ( 806.8957046614239061, -452.9681489794451181, -342.6393539086462852 ) ) ;
#700 = CARTESIAN_POINT ( 'NONE',  ( 809.9999999999993179, -512.9681489794448908, -339.9999999999999432 ) ) ;
#701 = ORIENTED_EDGE ( 'NONE', *, *, #28035, .F. ) ;
#702 = CARTESIAN_POINT ( 'NONE',  ( 756.1348686366196716, -65.26014174441471027, 347.5531968255698416 ) ) ;
#703 = CARTESIAN_POINT ( 'NONE',  ( 755.8990559732751535, -347.4636090269705733, -365.9055244015606831 ) ) ;
#704 = CARTESIAN_POINT ( 'NONE',  ( 812.7932403749906598, -303.1800572038740711, 327.7687537140311633 ) ) ;
#705 = CARTESIAN_POINT ( 'NONE',  ( 815.0009284576459549, -6.351050835323991173, 338.7629533639073429 ) ) ;
#706 = CARTESIAN_POINT ( 'NONE',  ( 790.0220218866281812, -175.0999726633346825, -363.2186876482849129 ) ) ;
#707 = CARTESIAN_POINT ( 'NONE',  ( 781.7834795799800531, -178.8164208402381519, -315.0636971347436202 ) ) ;
#708 = CARTESIAN_POINT ( 'NONE',  ( 755.5713283507202505, -365.3618753856920875, -334.6858677611754729 ) ) ;
#709 = ORIENTED_EDGE ( 'NONE', *, *, #5098, .T. ) ;
#710 = CARTESIAN_POINT ( 'NONE',  ( 777.4774526936600978, -274.2709662947833067, 304.7301800767027657 ) ) ;
#711 = EDGE_CURVE ( 'NONE', #43956, #10766, #14370, .T. ) ;
#712 = LINE ( 'NONE', #43645, #30692 ) ;
#713 = CARTESIAN_POINT ( 'NONE',  ( 795.9930595647434757, -363.0783235625955854, 320.7433823573372820 ) ) ;
#714 = CARTESIAN_POINT ( 'NONE',  ( -78.83651009197140525, 256.5000000000000568, -202.7499999999934914 ) ) ;
#715 = EDGE_CURVE ( 'NONE', #2952, #17860, #21035, .T. ) ;
#716 = CARTESIAN_POINT ( 'NONE',  ( 763.8424801807145741, -162.0090635724256742, 320.5453621957614700 ) ) ;
#717 = CARTESIAN_POINT ( 'NONE',  ( 754.8072714833581358, -52.81642084023856398, 338.1981804954720587 ) ) ;
#718 = ORIENTED_EDGE ( 'NONE', *, *, #22962, .T. ) ;
#719 = CARTESIAN_POINT ( 'NONE',  ( 812.3518521366052028, -409.0999726633340288, -326.5853460496235243 ) ) ;
#720 = CARTESIAN_POINT ( 'NONE',  ( 751.9810565676468741, -2.089148112965993231, -360.9747183278973921 ) ) ;
#721 = CARTESIAN_POINT ( 'NONE',  ( 745.1792804349281596, -278.1908817542434917, 343.7566961878542884 ) ) ;
#722 = CARTESIAN_POINT ( 'NONE',  ( 780.5290396650775619, -228.3510508353232922, 365.2837595273619513 ) ) ;
#723 = CARTESIAN_POINT ( 'NONE',  ( 803.4237431249931660, -351.1800572038740142, -331.2633955100225194 ) ) ;
#724 = CARTESIAN_POINT ( 'NONE',  ( 571.1634899080285095, 259.9999999999999432, -199.9999999999981526 ) ) ;
#725 = CARTESIAN_POINT ( 'NONE',  ( 802.5472867521000353, -460.3726999360611103, 350.8726784830461156 ) ) ;
#726 = CARTESIAN_POINT ( 'NONE',  ( 999.9999999999992042, 239.9999999999998863, -360.0000000000000000 ) ) ;
#727 = CARTESIAN_POINT ( 'NONE',  ( 783.0745993439762742, -272.1908817542434917, -365.1016975059196739 ) ) ;
#728 = EDGE_CURVE ( 'NONE', #13253, #15260, #21743, .T. ) ;
#729 = CARTESIAN_POINT ( 'NONE',  ( 744.7301800767019131, -4.816420840238714085, 337.4774526936615757 ) ) ;
#730 = CARTESIAN_POINT ( 'NONE',  ( 796.9462024416508257, -108.4527844766019911, 308.9653473494370246 ) ) ;
#731 = CARTESIAN_POINT ( 'NONE',  ( -208.8365100919714052, 258.0940000000001078, -193.8809999999926674 ) ) ;
#732 = CARTESIAN_POINT ( 'NONE',  ( 814.2001403089898304, -449.3618753856918602, -347.4397851343538264 ) ) ;
#733 = DIRECTION ( 'NONE',  ( -0.000000000000000000, 1.000000000000000000, -0.000000000000000000 ) ) ;
#734 = CARTESIAN_POINT ( 'NONE',  ( 745.5313806188320314, -375.2817908451523294, 333.7943932421247268 ) ) ;
#735 = LINE ( 'NONE', #4212, #45701 ) ;
#736 = CARTESIAN_POINT ( 'NONE',  ( 747.2067596250078623, -339.1800572038740142, 352.2312462859687230 ) ) ;
#737 = CARTESIAN_POINT ( 'NONE',  ( 763.0537975583475827, -96.45278447660203369, -371.0346526505627480 ) ) ;
#738 = CARTESIAN_POINT ( 'NONE',  ( 797.8594530101008786, -301.5436935675105588, -322.1405469898980982 ) ) ;
#739 = CARTESIAN_POINT ( 'NONE',  ( 928.0249999999991815, 219.9999999999998863, 339.9999999999999432 ) ) ;
#740 = CARTESIAN_POINT ( 'NONE',  ( 800.0135310231082713, -422.0891481129647218, 325.0180583372163028 ) ) ;
#741 = CARTESIAN_POINT ( 'NONE',  ( 790.9844846989617508, -190.3726999360619629, 317.2208543904092721 ) ) ;
#742 = CARTESIAN_POINT ( 'NONE',  ( 788.6739635108323228, -79.64542720878957027, -373.9316612368139090 ) ) ;
#743 = CARTESIAN_POINT ( 'NONE',  ( 786.6156483768007774, -97.44195992623281199, -315.5913626894246136 ) ) ;
#744 = CARTESIAN_POINT ( 'NONE',  ( 748.3538107759620743, -88.71468719896009247, 355.8262568251490165 ) ) ;
#745 = CARTESIAN_POINT ( 'NONE',  ( 800.0135310231082713, -422.0891481129647218, 325.0180583372163028 ) ) ;
#746 = ADVANCED_FACE ( 'NONE', ( #35841, #28910 ), #15052, .F. ) ;
#747 = CARTESIAN_POINT ( 'NONE',  ( 797.6776695296629214, 4.456306432488530866, -357.6776695296636603 ) ) ;
#749 = ORIENTED_EDGE ( 'NONE', *, *, #32375, .T. ) ;
#748 = CARTESIAN_POINT ( 'NONE',  ( 756.1348686366196716, -113.2601417444145682, -347.5531968255698416 ) ) ;
#750 = CARTESIAN_POINT ( 'NONE',  ( 762.3223304703356007, -103.5436935675111272, -322.3223304703362828 ) ) ;
#751 = CARTESIAN_POINT ( 'NONE',  ( 805.1016975059191054, -414.8965053807771710, -343.0745993439771837 ) ) ;
#753 = CARTESIAN_POINT ( 'NONE',  ( 788.7366044899766848, -227.9073299311471033, 316.5762568750059813 ) ) ;
#752 = CARTESIAN_POINT ( 'NONE',  ( 797.8594530101008786, -277.5436935675105019, 322.1405469898980982 ) ) ;
#754 = DIRECTION ( 'NONE',  ( -1.000000000000000000, -0.000000000000000000, -0.000000000000000000 ) ) ;
#755 = VERTEX_POINT ( 'NONE', #43223 ) ;
#756 = CARTESIAN_POINT ( 'NONE',  ( 802.1676090361156639, -422.6346026584192259, 327.8955696845344505 ) ) ;
#757 = VERTEX_POINT ( 'NONE', #11595 ) ;
#758 = CARTESIAN_POINT ( 'NONE',  ( 755.2512626584698410, -175.5436935675108998, 315.2512626584710915 ) ) ;
#759 = CARTESIAN_POINT ( 'NONE',  ( 800.9840315886518738, -268.9181544815162397, 354.1144889064786412 ) ) ;
#760 = ORIENTED_EDGE ( 'NONE', *, *, #25320, .T. ) ;
#761 = CARTESIAN_POINT ( 'NONE',  ( 793.0897708529556667, -78.55451811788046257, -361.3366627262616362 ) ) ;
#762 = CARTESIAN_POINT ( 'NONE',  ( 745.1769319972822814, -233.8055962898687028, 346.2694204179732083 ) ) ;
#763 = CARTESIAN_POINT ( 'NONE',  ( 804.9363028652555840, -232.2709662947834488, -338.2165204200192079 ) ) ;
#764 = ORIENTED_EDGE ( 'NONE', *, *, #41585, .T. ) ;
#765 = CARTESIAN_POINT ( 'NONE',  ( 797.8594530101008786, -397.5436935675100472, -322.1405469898980982 ) ) ;
#766 = CARTESIAN_POINT ( 'NONE',  ( 774.6858677611749044, -33.72551174932952733, -315.5713283507209894 ) ) ;
#767 = ADVANCED_FACE ( 'NONE', ( #39786 ), #14838, .T. ) ;
#768 = CARTESIAN_POINT ( 'NONE',  ( 756.1348686366196716, -281.2601417444139997, 347.5531968255698416 ) ) ;
#769 = CARTESIAN_POINT ( 'NONE',  ( 799.9999999999993179, -365.3551492539851893, 28.13243251470704109 ) ) ;
#770 = CARTESIAN_POINT ( 'NONE',  ( 919.9999999999993179, 154.9999999999998863, -360.0000000000000000 ) ) ;
#771 = EDGE_CURVE ( 'NONE', #13016, #19801, #19550, .T. ) ;
#772 = CARTESIAN_POINT ( 'NONE',  ( 755.0636971347428243, -4.270966294784170003, -341.7834795799807353 ) ) ;
#773 = DIRECTION ( 'NONE',  ( 0.000000000000000000, 0.000000000000000000, 1.000000000000000000 ) ) ;
#774 = ORIENTED_EDGE ( 'NONE', *, *, #715, .T. ) ;
#775 = CARTESIAN_POINT ( 'NONE',  ( 809.0717654672305343, -292.9181544815162397, -360.1688906516309885 ) ) ;
#776 = CARTESIAN_POINT ( 'NONE',  ( 813.5763878283155464, -171.8272453906074304, 351.1614460488615350 ) ) ;
#778 = CARTESIAN_POINT ( 'NONE',  ( 754.8072714833581358, -268.8164208402378108, -338.1981804954720587 ) ) ;
#777 = PLANE ( 'NONE',  #9882 ) ;
#779 = LINE ( 'NONE', #28956, #941 ) ;
#780 = CARTESIAN_POINT ( 'NONE',  ( 793.0897708529556667, -126.5545181178803205, -361.3366627262616362 ) ) ;
#781 = CARTESIAN_POINT ( 'NONE',  ( 810.7187646348534145, -18.45278447660230725, 356.7737145352016341 ) ) ;
#782 = PLANE ( 'NONE',  #39472 ) ;
#783 = CARTESIAN_POINT ( 'NONE',  ( 745.7998596910086917, -341.3618753856922012, -332.5602148656461168 ) ) ;
#784 = CARTESIAN_POINT ( 'NONE',  ( 1238.921997096861332, 430.0000000000002842, -320.0000000000000568 ) ) ;
#785 = CARTESIAN_POINT ( 'NONE',  ( 804.4286716492782716, 6.638124614306706306, 345.3141322388244703 ) ) ;
#786 = CARTESIAN_POINT ( 'NONE',  ( 748.6759233522253680, -280.3726999360616787, 324.3348316497537098 ) ) ;
#787 = CARTESIAN_POINT ( 'NONE',  ( 795.6651683502461765, -202.7146871989597514, -371.3240766477733814 ) ) ;
#788 = CARTESIAN_POINT ( 'NONE',  ( 815.2698199232961542, -208.8164208402380666, 342.5225473063383106 ) ) ;
#789 = CARTESIAN_POINT ( 'NONE',  ( 815.1787889125755555, -438.8965053807771710, -343.7953271457877804 ) ) ;
#790 = DIRECTION ( 'NONE',  ( -1.000000000000000000, -0.000000000000000000, -0.000000000000000000 ) ) ;
#791 = VERTEX_POINT ( 'NONE', #739 ) ;
#792 = CARTESIAN_POINT ( 'NONE',  ( 781.8018195045266339, -310.2709662947832499, 365.1927285166406705 ) ) ;
#793 = CARTESIAN_POINT ( 'NONE',  ( 798.5707757039680246, -77.46360902697138329, 356.7845633553585003 ) ) ;
#794 = CARTESIAN_POINT ( 'NONE',  ( 780.5290396650775619, 11.64894916467595642, -365.2837595273619513 ) ) ;
#795 = CARTESIAN_POINT ( 'NONE',  ( 999.9999999999992042, 249.9999999999998863, -360.0000000000000000 ) ) ;
#796 = CARTESIAN_POINT ( 'NONE',  ( -919.9999999999993179, 154.9999999999998863, 339.9999999999999432 ) ) ;
#798 = CARTESIAN_POINT ( 'NONE',  ( 792.1044303154645831, -372.4527844766010958, 317.8323909638837677 ) ) ;
#797 = CARTESIAN_POINT ( 'NONE',  ( 780.5290396650775619, -156.3510508353235480, 365.2837595273619513 ) ) ;
#799 = EDGE_LOOP ( 'NONE', ( #25522, #592, #42461, #2264, #39166 ) ) ;
#800 = CARTESIAN_POINT ( 'NONE',  ( 786.6156483768007774, -289.4419599262321299, -315.5913626894246136 ) ) ;
#801 = CARTESIAN_POINT ( 'NONE',  ( 751.2241431872005251, -280.1692326535049347, -359.9636004259367610 ) ) ;
#802 = CARTESIAN_POINT ( 'NONE',  ( 939.9999999999992042, 50.81038600091411439, -209.9999999999999716 ) ) ;
#803 = CARTESIAN_POINT ( 'NONE',  ( 804.7487373415286811, 4.456306432488530866, 364.7487373415288516 ) ) ;
#804 = ORIENTED_EDGE ( 'NONE', *, *, #1226, .T. ) ;
#805 = CARTESIAN_POINT ( 'NONE',  ( 774.6312213355099630, -335.3618753856920307, 364.6798772138717482 ) ) ;
#806 = CARTESIAN_POINT ( 'NONE',  ( 805.0264073115434940, -78.35105083532376113, -339.4763451958999099 ) ) ;
#807 = CARTESIAN_POINT ( 'NONE',  ( 802.1676090361156639, -446.6346026584189985, 327.8955696845344505 ) ) ;
#808 = CARTESIAN_POINT ( 'NONE',  ( 804.7487373415286811, -163.5436935675109567, -364.7487373415288516 ) ) ;
#809 = EDGE_LOOP ( 'NONE', ( #44423, #29622, #244, #36475, #38067, #15995 ) ) ;
#810 = CARTESIAN_POINT ( 'NONE',  ( 755.5713283507202505, -149.3618753856928265, -334.6858677611754729 ) ) ;
#811 = VERTEX_POINT ( 'NONE', #11356 ) ;
#812 = CARTESIAN_POINT ( 'NONE',  ( 769.0155153010367712, -442.3726999360611103, -362.7791456095907279 ) ) ;
#813 =( BOUNDED_CURVE ( )  B_SPLINE_CURVE ( 2, ( #30233, #2278, #8779, #33709, #16615, #44325, #30702 ),
 .UNSPECIFIED., .F., .T. ) 
 B_SPLINE_CURVE_WITH_KNOTS ( ( 3, 2, 2, 3 ),
 ( 0.006081874955971018626, 0.006818181818181817851, 0.009090909090909090468, 0.01033270150184909669 ),
 .UNSPECIFIED. ) 
 CURVE ( )  GEOMETRIC_REPRESENTATION_ITEM ( )  RATIONAL_B_SPLINE_CURVE ( ( 0.4977709609702910543, 0.4983514209501199721, 0.5000002209606653203, 0.4949109396520706694, 0.5000002209606653203, 0.4972194953619585855, 0.4974774836351868457 ) ) 
 REPRESENTATION_ITEM ( '' )  );
#814 = CARTESIAN_POINT ( 'NONE',  ( 802.1676090361156639, 9.365397341579420498, 327.8955696845344505 ) ) ;
#815 = CARTESIAN_POINT ( 'NONE',  ( 814.5518280994195948, -231.7255117493288310, 332.4837098697145734 ) ) ;
#816 = CARTESIAN_POINT ( 'NONE',  ( 775.9200461376533440, -119.8055962898690865, 315.3028492785443291 ) ) ;
#819 = CARTESIAN_POINT ( 'NONE',  ( 756.1443688327750579, -381.6237781080500326, 314.3581564841659315 ) ) ;
#818 = DIRECTION ( 'NONE',  ( 0.000000000000000000, -1.000000000000000000, 0.000000000000000000 ) ) ;
#817 = FACE_OUTER_BOUND ( 'NONE', #10229, .T. ) ;
#820 = VERTEX_POINT ( 'NONE', #11128 ) ;
#821 = CARTESIAN_POINT ( 'NONE',  ( 769.9779781133707957, -379.0999726633341993, -316.7813123517150871 ) ) ;
#822 = CARTESIAN_POINT ( 'NONE',  ( 799.9999999999993179, 205.0000000000000568, -255.0000000000000000 ) ) ;
#823 = CARTESIAN_POINT ( 'NONE',  ( 786.2694204179717872, -213.2817908451527842, -305.1769319972829067 ) ) ;
#824 = CIRCLE ( 'NONE', #26615, 2.749999999999808153 ) ;
#825 = CARTESIAN_POINT ( 'NONE',  ( 747.6481478633932056, -61.09997266333506616, 353.4146539503763620 ) ) ;
#827 = FACE_OUTER_BOUND ( 'NONE', #26973, .T. ) ;
#826 = DIRECTION ( 'NONE',  ( 1.000000000000000000, 0.000000000000000000, 0.000000000000000000 ) ) ;
#828 = CARTESIAN_POINT ( 'NONE',  ( 789.9200121543843807, -313.9874144716866908, -317.0176451133914384 ) ) ;
#829 = LINE ( 'NONE', #22074, #26924 ) ;
#830 = CARTESIAN_POINT ( 'NONE',  ( 768.9521613784389729, -177.8272453906074304, -373.2346286133773106 ) ) ;
#831 = DIRECTION ( 'NONE',  ( 1.000000000000000000, -0.000000000000000000, 0.000000000000000000 ) ) ;
#832 = FACE_BOUND ( 'NONE', #35157, .T. ) ;
#833 = CARTESIAN_POINT ( 'NONE',  ( 783.0745993439762742, -392.1908817542432075, 365.1016975059196739 ) ) ;
#834 = CARTESIAN_POINT ( 'NONE',  ( 772.4837098697145166, -215.3618753856925707, -374.5518280994205611 ) ) ;
#835 = CARTESIAN_POINT ( 'NONE',  ( -786.4999999999993179, -544.8427095258973623, -350.0000000000000000 ) ) ;
#836 = CARTESIAN_POINT ( 'NONE',  ( 758.0580252608178853, -6.452784476602343666, -328.0187753319985404 ) ) ;
#837 = CARTESIAN_POINT ( 'NONE',  ( 757.7880784355613741, -138.0090635724257311, 312.4576283171834916 ) ) ;
#838 = CARTESIAN_POINT ( 'NONE',  ( 778.7502325331095108, -96.35105083532370429, -304.6391490659818828 ) ) ;
#839 = CARTESIAN_POINT ( 'NONE',  ( 814.2001403089898304, -113.3618753856929260, 347.4397851343538264 ) ) ;
#840 = CARTESIAN_POINT ( 'NONE',  ( 751.6929314249748586, -342.9982390220557136, -318.8095938919659034 ) ) ;
#841 = CARTESIAN_POINT ( 'NONE',  ( 772.4999999999993179, -512.9681489794448908, 370.0000000000000000 ) ) ;
#842 = CYLINDRICAL_SURFACE ( 'NONE', #628, 12.00000000000001066 ) ;
#843 = CARTESIAN_POINT ( 'NONE',  ( 788.7366044899766848, -227.9073299311471033, 316.5762568750059813 ) ) ;
#844 = CARTESIAN_POINT ( 'NONE',  ( 769.9779781133707957, 4.900027336664720679, 316.7813123517150871 ) ) ;
#845 = CARTESIAN_POINT ( 'NONE',  ( 791.1614460488616487, -419.2601417444136587, -373.5763878283158874 ) ) ;
#846 = CARTESIAN_POINT ( 'NONE',  ( 749.2812353651451076, -414.4527844766010389, -323.2262854647983090 ) ) ;
#847 = LINE ( 'NONE', #398, #9226 ) ;
#848 = CARTESIAN_POINT ( 'NONE',  ( 751.2241431872005251, -16.16923265350578021, 359.9636004259367610 ) ) ;
#849 = EDGE_LOOP ( 'NONE', ( #8777, #12953, #44083, #25218 ) ) ;
#850 = CARTESIAN_POINT ( 'NONE',  ( 754.8983024940795303, -186.8965053807779668, -336.9254006560228163 ) ) ;
#851 = CARTESIAN_POINT ( 'NONE',  ( 774.6858677611749044, -33.72551174932952733, 315.5713283507209894 ) ) ;
#852 = CARTESIAN_POINT ( 'NONE',  ( 758.0141637701419768, -207.0783235625960685, -367.2620300519063790 ) ) ;
#853 =( NAMED_UNIT ( * ) PLANE_ANGLE_UNIT ( ) SI_UNIT ( $, .RADIAN. ) );
#854 = CARTESIAN_POINT ( 'NONE',  ( 764.3348316497523456, -358.7146871989592114, 308.6759233522265617 ) ) ;
#855 = CARTESIAN_POINT ( 'NONE',  ( 762.3223304703356007, -151.5436935675109851, 322.3223304703362828 ) ) ;
#856 = ORIENTED_EDGE ( 'NONE', *, *, #1291, .T. ) ;
#857 = CARTESIAN_POINT ( 'NONE',  ( 773.7943932421234194, -431.8055962898681059, 305.5313806188329409 ) ) ;
#858 = CARTESIAN_POINT ( 'NONE',  ( 756.5762568750052424, -339.1800572038740142, 348.7366044899774238 ) ) ;
#859 = CARTESIAN_POINT ( 'NONE',  ( 744.7301800767019131, -52.81642084023856398, -337.4774526936615757 ) ) ;
#860 = CARTESIAN_POINT ( 'NONE',  ( 757.7880784355613741, -450.0090635724248500, -312.4576283171834916 ) ) ;
#861 = VERTEX_POINT ( 'NONE', #21514 ) ;
#862 = CARTESIAN_POINT ( 'NONE',  ( 804.8461984189677878, -314.1908817542433781, -336.9566956441385628 ) ) ;
#863 = ITEM_DEFINED_TRANSFORMATION ( 'NONE', 'NONE', #37834,  #26858 ) ;
#865 = CARTESIAN_POINT ( 'NONE',  ( 796.9571628226829034, -359.4636090269705164, 321.2382568024804641 ) ) ;
#864 = CARTESIAN_POINT ( 'NONE',  ( 778.1981804954714335, -58.27096629478398171, 314.8072714833589885 ) ) ;
#867 = CARTESIAN_POINT ( 'NONE',  ( 813.2346286133761168, -293.2601417444139429, 328.9521613784389160 ) ) ;
#866 = CARTESIAN_POINT ( 'NONE',  ( 755.2512626584698410, -391.5436935675101608, 315.2512626584710915 ) ) ;
#868 = CARTESIAN_POINT ( 'NONE',  ( 744.8212110874229666, -66.89650538077835051, 336.2046728542121627 ) ) ;
#869 = CARTESIAN_POINT ( 'NONE',  ( 763.8424801807145741, -306.0090635724252479, -320.5453621957614700 ) ) ;
#870 = CARTESIAN_POINT ( 'NONE',  ( 781.7834795799800531, -274.8164208402378108, -315.0636971347436202 ) ) ;
#871 = DIRECTION ( 'NONE',  ( 1.000000000000000000, -0.000000000000000000, -0.000000000000000000 ) ) ;
#872 = CARTESIAN_POINT ( 'NONE',  ( 803.4237431249931660, -135.1800572038746679, -331.2633955100225194 ) ) ;
#873 = CARTESIAN_POINT ( 'NONE',  ( -728.8365100919714905, 240.0000000000001990, -199.9999999999890861 ) ) ;
#874 = ORIENTED_EDGE ( 'NONE', *, *, #5250, .T. ) ;
#875 = CARTESIAN_POINT ( 'NONE',  ( 751.6929314249748586, -438.9982390220553157, 318.8095938919659034 ) ) ;
#877 = CARTESIAN_POINT ( 'NONE',  ( -37.63011601220122770, -365.3551492539851893, -18.13243251470705886 ) ) ;
#876 = DIRECTION ( 'NONE',  ( -0.000000000000000000, -0.000000000000000000, 1.000000000000000000 ) ) ;
#878 = CARTESIAN_POINT ( 'NONE',  ( 795.8262568251477660, -70.37269993606230400, -308.3538107759623585 ) ) ;
#879 = DIRECTION ( 'NONE',  ( -0.000000000000000000, 1.000000000000000000, -0.000000000000000000 ) ) ;
#880 = CARTESIAN_POINT ( 'NONE',  ( -728.8365100919714905, 260.0000000000001705, -197.2499999999891998 ) ) ;
#881 = CARTESIAN_POINT ( 'NONE',  ( 772.4468031744293057, -249.8272453906072315, 363.8651313633793620 ) ) ;
#882 = CARTESIAN_POINT ( 'NONE',  ( 801.9419747391806368, -162.4527844766018632, 351.9812246680014027 ) ) ;
#883 = ORIENTED_EDGE ( 'NONE', *, *, #3255, .T. ) ;
#884 =( GEOMETRIC_REPRESENTATION_CONTEXT ( 3 ) GLOBAL_UNCERTAINTY_ASSIGNED_CONTEXT ( ( #29214 ) ) GLOBAL_UNIT_ASSIGNED_CONTEXT ( ( #30081, #19913, #9523 ) ) REPRESENTATION_CONTEXT ( 'NONE', 'WORKASPACE' ) );
#885 = CARTESIAN_POINT ( 'NONE',  ( 814.2001403089898304, -89.36187538569299704, -347.4397851343538264 ) ) ;
#886 = CARTESIAN_POINT ( 'NONE',  ( 775.9200461376533440, -311.8055962898685038, 315.3028492785443291 ) ) ;
#887 = DIRECTION ( 'NONE',  ( 1.000000000000000000, -0.000000000000000000, -0.000000000000000000 ) ) ;
#888 = CARTESIAN_POINT ( 'NONE',  ( 768.9521613784389729, -33.82724539060788516, 373.2346286133773106 ) ) ;
#889 = CARTESIAN_POINT ( 'NONE',  ( 754.9967657858570647, -241.5436935675106156, -365.0032342141425374 ) ) ;
#890 = CARTESIAN_POINT ( 'NONE',  ( 755.0636971347428243, -100.2709662947838609, 341.7834795799807353 ) ) ;
#891 = DIRECTION ( 'NONE',  ( 0.000000000000000000, 0.000000000000000000, 1.000000000000000000 ) ) ;
#892 = CARTESIAN_POINT ( 'NONE',  ( 810.1134526219336749, -320.5328690171411949, -357.8822607201570349 ) ) ;
#893 = CARTESIAN_POINT ( 'NONE',  ( 811.3240766477731540, -436.3726999360612240, 355.6651683502462902 ) ) ;
#894 = CARTESIAN_POINT ( 'NONE',  ( 758.8095938919642549, -320.0891481129648355, -311.6929314249763365 ) ) ;
#895 = DIRECTION ( 'NONE',  ( 0.000000000000000000, 0.000000000000000000, 1.000000000000000000 ) ) ;
#896 = CARTESIAN_POINT ( 'NONE',  ( 798.7617431975189675, -411.6237781080499758, 323.0428371773161871 ) ) ;
#897 = EDGE_LOOP ( 'NONE', ( #13761, #35388, #39807, #18362, #590, #6557 ) ) ;
#898 = CARTESIAN_POINT ( 'NONE',  ( 785.3141322388236176, -405.7255117493283478, -364.4286716492789537 ) ) ;
#899 = CARTESIAN_POINT ( 'NONE',  ( 778.1981804954714335, -226.2709662947834204, -314.8072714833589885 ) ) ;
#900 = CARTESIAN_POINT ( 'NONE',  ( 778.7502325331095108, -72.35105083532378956, -304.6391490659818828 ) ) ;
#901 = DIRECTION ( 'NONE',  ( -1.000000000000000000, 1.892425610156518354E-16, 0.000000000000000000 ) ) ;
#902 = CARTESIAN_POINT ( 'NONE',  ( 812.6845335610512393, -199.9874144716870603, 353.5525998758768651 ) ) ;
#903 = CARTESIAN_POINT ( 'NONE',  ( 792.1044303154646968, -36.45278447660224685, 317.8323909638837677 ) ) ;
#904 = ORIENTED_EDGE ( 'NONE', *, *, #41975, .F. ) ;
#905 = CARTESIAN_POINT ( 'NONE',  ( 763.2154366446407039, -237.6237781080505442, -321.4292242960311228 ) ) ;
#906 = CARTESIAN_POINT ( 'NONE',  ( 778.1981804954714335, -226.2709662947834204, 314.8072714833589885 ) ) ;
#907 = CARTESIAN_POINT ( 'NONE',  ( 810.1134526219336749, -56.53286901714201917, -357.8822607201570349 ) ) ;
#908 = CARTESIAN_POINT ( 'NONE',  ( 803.4237431249931660, -351.1800572038740142, 331.2633955100225194 ) ) ;
#909 = CIRCLE ( 'NONE', #14943, 12.00000000000001066 ) ;
#910 = DIRECTION ( 'NONE',  ( -0.000000000000000000, 1.000000000000000000, -0.000000000000000000 ) ) ;
#911 = VERTEX_POINT ( 'NONE', #25198 ) ;
#912 = CARTESIAN_POINT ( 'NONE',  ( 750.9282345327678740, -328.9181544815160692, -319.8311093483690115 ) ) ;
#913 = ADVANCED_FACE ( 'NONE', ( #39558 ), #7665, .T. ) ;
#914 = CARTESIAN_POINT ( 'NONE',  ( 745.0891759886404770, -292.2709662947831930, 342.4968714119734159 ) ) ;
#915 = CARTESIAN_POINT ( 'NONE',  ( 803.8556311672234642, 14.37622189194867417, 365.6418435158340117 ) ) ;
#916 = CARTESIAN_POINT ( 'NONE',  ( 804.4086373105744769, -193.6454272087891582, -333.3843516231986541 ) ) ;
#917 = CARTESIAN_POINT ( 'NONE',  ( 762.1405469898971887, -169.5436935675108430, -357.8594530101015607 ) ) ;
#918 = CARTESIAN_POINT ( 'NONE',  ( 778.1981804954715471, -394.2709662947829088, -314.8072714833591021 ) ) ;
#919 = EDGE_CURVE ( 'NONE', #14904, #3234, #12181, .T. ) ;
#920 = EDGE_LOOP ( 'NONE', ( #2986, #31243, #45604, #112 ) ) ;
#921 = ORIENTED_EDGE ( 'NONE', *, *, #22135, .T. ) ;
#922 = CARTESIAN_POINT ( 'NONE',  ( 772.4837098697144029, -287.3618753856923718, 374.5518280994205611 ) ) ;
#923 = CARTESIAN_POINT ( 'NONE',  ( 787.4999999999992042, -512.9681489794448908, 309.9999999999998863 ) ) ;
#924 = CARTESIAN_POINT ( 'NONE',  ( 790.9844846989617508, -214.3726999360618493, 317.2208543904092721 ) ) ;
#925 = CARTESIAN_POINT ( 'NONE',  ( 454.7528517110262101, 199.9999999999999432, -122.7905160835442615 ) ) ;
#926 = CARTESIAN_POINT ( 'NONE',  ( 754.7162404726377645, -158.7363362996984222, 339.4709603349214717 ) ) ;
#927 = CARTESIAN_POINT ( 'NONE',  ( 803.4237431249931660, -39.18005720387496638, 331.2633955100225194 ) ) ;
#928 = VERTEX_POINT ( 'NONE', #4438 ) ;
#929 = CARTESIAN_POINT ( 'NONE',  ( 749.5768839229115201, -396.5545181178794678, -358.0661480581553064 ) ) ;
#930 = CIRCLE ( 'NONE', #36312, 10.00000000000000888 ) ;
#931 = CARTESIAN_POINT ( 'NONE',  ( 787.5162901302840055, -11.36187538569323863, -305.4481719005793252 ) ) ;
#932 = CARTESIAN_POINT ( 'NONE',  ( 749.5768839229115201, -276.5545181178798657, 358.0661480581553064 ) ) ;
#933 = CARTESIAN_POINT ( 'NONE',  ( 756.1348686366196716, -209.2601417444142839, 347.5531968255698416 ) ) ;
#934 = CARTESIAN_POINT ( 'NONE',  ( 800.0135310231082713, -374.0891481129647786, -325.0180583372163028 ) ) ;
#935 = DIRECTION ( 'NONE',  ( 1.000000000000000000, -8.326672684688676025E-16, 0.000000000000000000 ) ) ;
#936 = CARTESIAN_POINT ( 'NONE',  ( 798.5707757039680246, -461.4636090269701754, 356.7845633553585003 ) ) ;
#937 = CYLINDRICAL_SURFACE ( 'NONE', #26687, 1.000000000000000888 ) ;
#938 = CARTESIAN_POINT ( 'NONE',  ( 793.0897708529556667, -246.5545181178799510, -361.3366627262616362 ) ) ;
#939 = CARTESIAN_POINT ( 'NONE',  ( 808.3070685750230950, -42.99823902205675807, 361.1904061080339261 ) ) ;
#940 = CARTESIAN_POINT ( 'NONE',  ( 787.4397851343537695, -117.7255117493292715, 374.2001403089903988 ) ) ;
#941 = VECTOR ( 'NONE', #28498, 1000.000000000000000 ) ;
#942 = CARTESIAN_POINT ( 'NONE',  ( 799.9999999999993179, -512.9681489794448908, 339.9999999999999432 ) ) ;
#943 = CARTESIAN_POINT ( 'NONE',  ( 772.4999999999993179, -512.9681489794448908, -339.9999999999999432 ) ) ;
#944 = CARTESIAN_POINT ( 'NONE',  ( 811.3240766477731540, -388.3726999360613945, 355.6651683502462902 ) ) ;
#945 = DIRECTION ( 'NONE',  ( 1.000000000000000000, 0.000000000000000000, 0.000000000000000000 ) ) ;
#946 = CARTESIAN_POINT ( 'NONE',  ( 782.5225473063381969, -358.2709662947829088, 375.2698199232970637 ) ) ;
#947 = CARTESIAN_POINT ( 'NONE',  ( 800.2193346964447755, -306.9982390220558273, -355.1360043628815788 ) ) ;
#948 = DIRECTION ( 'NONE',  ( -0.000000000000000000, 1.000000000000000000, -0.000000000000000000 ) ) ;
#949 = CARTESIAN_POINT ( 'NONE',  ( 802.1676090361156639, -446.6346026584189985, 327.8955696845344505 ) ) ;
#950 = CARTESIAN_POINT ( 'NONE',  ( 755.5913626894240451, -205.6454272087891297, 346.6156483768012890 ) ) ;
#951 = CARTESIAN_POINT ( 'NONE',  ( 768.9521613784389729, -57.82724539060780700, -373.2346286133773106 ) ) ;
#952 = CARTESIAN_POINT ( 'NONE',  ( 780.5290396650775619, -108.3510508353236759, -365.2837595273619513 ) ) ;
#953 = CARTESIAN_POINT ( 'NONE',  ( 749.8865473780648472, -92.53286901714190549, 322.1177392798429082 ) ) ;
#954 = CARTESIAN_POINT ( 'NONE',  ( 804.4286716492782716, -425.3618753856919170, 345.3141322388244703 ) ) ;
#955 = EDGE_CURVE ( 'NONE', #16933, #23058, #18525, .T. ) ;
#956 = CARTESIAN_POINT ( 'NONE',  ( 768.0187753319979720, -8.634602658420517329, -318.0580252608186242 ) ) ;
#958 = ORIENTED_EDGE ( 'NONE', *, *, #40695, .F. ) ;
#957 = CARTESIAN_POINT ( 'NONE',  ( 798.7617431975189675, -147.6237781080508285, -323.0428371773161871 ) ) ;
#959 = CARTESIAN_POINT ( 'NONE',  ( 804.9363028652555840, -112.2709662947838325, -338.2165204200192079 ) ) ;
#960 = EDGE_CURVE ( 'NONE', #27431, #8959, #32146, .T. ) ;
#961 = CARTESIAN_POINT ( 'NONE',  ( 765.8855110935204493, -406.1692326535045368, -319.0159684113471599 ) ) ;
#963 = CARTESIAN_POINT ( 'NONE',  ( 797.6776695296629214, -259.5436935675106156, 357.6776695296636603 ) ) ;
#962 = CARTESIAN_POINT ( 'NONE',  ( 803.4237431249931660, -255.1800572038742700, 331.2633955100225194 ) ) ;
#964 = VECTOR ( 'NONE', #44223, 999.9999999999998863 ) ;
#965 = LINE ( 'NONE', #21311, #37445 ) ;
#966 = VERTEX_POINT ( 'NONE', #41454 ) ;
#967 = CARTESIAN_POINT ( 'NONE',  ( 764.8639956371174549, -440.0891481129644944, 319.7806653035542013 ) ) ;
#968 = ORIENTED_EDGE ( 'NONE', *, *, #23222, .T. ) ;
#969 =( NAMED_UNIT ( * ) SI_UNIT ( $, .STERADIAN. ) SOLID_ANGLE_UNIT ( ) );
#970 = ADVANCED_FACE ( 'NONE', ( #44230 ), #9588, .F. ) ;
#971 = CARTESIAN_POINT ( 'NONE',  ( 787.4397851343537695, -189.7255117493290300, 374.2001403089903988 ) ) ;
#972 = CARTESIAN_POINT ( 'NONE',  ( 784.1219089521767955, -261.2817908451526705, 315.0488828828318333 ) ) ;
#973 = ORIENTED_EDGE ( 'NONE', *, *, #27496, .F. ) ;
#974 = CARTESIAN_POINT ( 'NONE',  ( 759.0159684113467620, -88.91815448151682233, -325.8855110935213020 ) ) ;
#975 = CARTESIAN_POINT ( 'NONE',  ( 766.5853460496234675, -205.9874144716870035, 372.3518521366060554 ) ) ;
#976 = CARTESIAN_POINT ( 'NONE',  ( 774.6312213355098493, -239.3618753856924855, -364.6798772138717482 ) ) ;
#977 = ORIENTED_EDGE ( 'NONE', *, *, #34820, .T. ) ;
#978 = CARTESIAN_POINT ( 'NONE',  ( 756.3353852180819104, -389.9073299311465348, -331.1735550268788302 ) ) ;
#979 = CARTESIAN_POINT ( 'NONE',  ( 759.9864689768902508, -50.08914811296584446, -354.9819416627836404 ) ) ;
#980 = AXIS2_PLACEMENT_3D ( 'NONE', #10116, #31353, #10336 ) ;
#981 = CARTESIAN_POINT ( 'NONE',  ( 776.9566956441375396, -276.8965053807776258, 364.8461984189686405 ) ) ;
#982 = CARTESIAN_POINT ( 'NONE',  ( 999.5857864376259840, -600.0000000000001137, 360.0000000000000000 ) ) ;
#983 = FACE_OUTER_BOUND ( 'NONE', #35453, .T. ) ;
#984 = CARTESIAN_POINT ( 'NONE',  ( 754.8072714833581358, -28.81642084023863148, -338.1981804954720587 ) ) ;
#985 = LINE ( 'NONE', #15090, #37294 ) ;
#986 = ORIENTED_EDGE ( 'NONE', *, *, #23842, .F. ) ;
#987 = CARTESIAN_POINT ( 'NONE',  ( 764.1737431748507561, -298.3726999360616787, -371.6461892240376415 ) ) ;
#988 = EDGE_CURVE ( 'NONE', #30488, #37811, #44694, .T. ) ;
#989 = CARTESIAN_POINT ( 'NONE',  ( 812.3518521366052028, -169.0999726633347393, 326.5853460496235243 ) ) ;
#991 = CARTESIAN_POINT ( 'NONE',  ( 774.6312213355099630, -263.3618753856924855, -364.6798772138717482 ) ) ;
#990 = CARTESIAN_POINT ( 'NONE',  ( -78.83651009197140525, 240.0000000000000853, -199.9999999999936051 ) ) ;
#992 = ADVANCED_FACE ( 'NONE', ( #19750 ), #19977, .F. ) ;
#993 = CARTESIAN_POINT ( 'NONE',  ( -39.63011601220123481, 26.27639943461401018, 900.0000000000001137 ) ) ;
#994 = CARTESIAN_POINT ( 'NONE',  ( 802.5472867521000353, -148.3726999360620198, -350.8726784830461156 ) ) ;
#995 = AXIS2_PLACEMENT_3D ( 'NONE', #25421, #31508, #45374 ) ;
#996 = CARTESIAN_POINT ( 'NONE',  ( -728.8365100919714905, 240.0000000000001990, -199.9999999999890861 ) ) ;
#997 = CARTESIAN_POINT ( 'NONE',  ( 759.8311093483677041, -22.16923265350575889, -310.9282345327691814 ) ) ;
#998 = CARTESIAN_POINT ( 'NONE',  ( 754.9967657858570647, -361.5436935675103882, -365.0032342141425943 ) ) ;
#999 = CARTESIAN_POINT ( 'NONE',  ( -598.8365100919716042, 240.0000000000001705, -199.9999999999899671 ) ) ;
#1000 = CARTESIAN_POINT ( 'NONE',  ( 762.1405469898971887, -25.54369356751136877, 357.8594530101015607 ) ) ;
#1001 = VECTOR ( 'NONE', #11333, 1000.000000000000000 ) ;
#1002 = CARTESIAN_POINT ( 'NONE',  ( 811.3240766477731540, -292.3726999360616219, 355.6651683502462902 ) ) ;
#1003 = CARTESIAN_POINT ( 'NONE',  ( 810.1134526219336749, -248.5328690171414223, -357.8822607201570349 ) ) ;
#1004 = CARTESIAN_POINT ( 'NONE',  ( 772.4837098697144029, -215.3618753856925423, 374.5518280994205611 ) ) ;
#1005 = CARTESIAN_POINT ( 'NONE',  ( 804.7487373415286811, 4.456306432488530866, -364.7487373415288516 ) ) ;
#1006 = DIRECTION ( 'NONE',  ( -0.000000000000000000, 1.000000000000000000, -0.000000000000000000 ) ) ;
#1007 = ORIENTED_EDGE ( 'NONE', *, *, #29695, .T. ) ;
#1008 = CARTESIAN_POINT ( 'NONE',  ( 781.7834795799800531, -322.8164208402377540, 315.0636971347436202 ) ) ;
#1009 = EDGE_CURVE ( 'NONE', #13600, #26360, #44455, .T. ) ;
#1010 = CARTESIAN_POINT ( 'NONE',  ( 790.9844846989617508, -94.37269993606224716, 317.2208543904092721 ) ) ;
#1011 = CARTESIAN_POINT ( 'NONE',  ( 803.8651313633788504, 18.73985825558501972, -332.4468031744301015 ) ) ;
#1012 = CYLINDRICAL_SURFACE ( 'NONE', #8516, 19.99999999999990763 ) ;
#1013 = VECTOR ( 'NONE', #42593, 1000.000000000000000 ) ;
#1014 = EDGE_CURVE ( 'NONE', #33458, #19810, #12588, .T. ) ;
#1015 = LINE ( 'NONE', #7286, #17369 ) ;
#1017 = CARTESIAN_POINT ( 'NONE',  ( 791.9812246680005501, -356.6346026584193964, 361.9419747391813189 ) ) ;
#1016 = CARTESIAN_POINT ( 'NONE',  ( 764.0069404352550464, -159.0783235625962391, 359.2566176426627180 ) ) ;
#1018 = ORIENTED_EDGE ( 'NONE', *, *, #15333, .T. ) ;
#1019 = EDGE_CURVE ( 'NONE', #16583, #8247, #41590, .T. ) ;
#1020 = CARTESIAN_POINT ( 'NONE',  ( 783.0433043558608688, -288.8965053807775121, -315.1538015810313027 ) ) ;
#1021 = CARTESIAN_POINT ( 'NONE',  ( 788.7366044899766848, -155.9073299311473306, 316.5762568750059813 ) ) ;
#1022 = UNCERTAINTY_MEASURE_WITH_UNIT (LENGTH_MEASURE( 1.000000000000000082E-05 ), #11175, 'distance_accuracy_value', 'NONE');
#1023 = CARTESIAN_POINT ( 'NONE',  ( 807.5423716828161105, -321.0783235625956991, -362.2119215644372048 ) ) ;
#1024 = DIRECTION ( 'NONE',  ( -1.000000000000000000, -0.000000000000000000, 0.000000000000000000 ) ) ;
#1025 = CARTESIAN_POINT ( 'NONE',  ( 808.0189434323515343, 9.910851887033969021, 319.0252816721025511 ) ) ;
#1026 = CARTESIAN_POINT ( 'NONE',  ( 800.0135310231082713, -302.0891481129650629, 325.0180583372163028 ) ) ;
#1027 = ORIENTED_EDGE ( 'NONE', *, *, #7837, .T. ) ;
#1028 = CARTESIAN_POINT ( 'NONE',  ( 755.3201227861273992, -339.7255117493285184, 345.3687786644892981 ) ) ;
#1029 = VERTEX_POINT ( 'NONE', #23428 ) ;
#1030 = DIRECTION ( 'NONE',  ( 0.000000000000000000, 0.000000000000000000, 1.000000000000000000 ) ) ;
#1031 = CARTESIAN_POINT ( 'NONE',  ( 749.2812353651451076, -198.4527844766017495, -323.2262854647983090 ) ) ;
#1032 = VERTEX_POINT ( 'NONE', #9806 ) ;
#1033 = VECTOR ( 'NONE', #41918, 1000.000000000000000 ) ;
#1034 = CARTESIAN_POINT ( 'NONE',  ( 757.8323909638828582, -146.6346026584200786, -352.1044303154654358 ) ) ;
#1035 = CIRCLE ( 'NONE', #26827, 20.00000000000004619 ) ;
#1036 = ORIENTED_EDGE ( 'NONE', *, *, #41383, .F. ) ;
#1037 = CARTESIAN_POINT ( 'NONE',  ( 757.4527132478984868, -424.3726999360612808, -329.1273215169538844 ) ) ;
#1038 = CARTESIAN_POINT ( 'NONE',  ( 781.8018195045266339, 1.729033705215812011, 365.1927285166406705 ) ) ;
#1039 = CARTESIAN_POINT ( 'NONE',  ( 796.7845633553578182, -153.6237781080508000, 358.5707757039688204 ) ) ;
#1041 = DIRECTION ( 'NONE',  ( -1.000000000000000000, 0.000000000000000000, 0.000000000000000000 ) ) ;
#1040 = DIRECTION ( 'NONE',  ( -1.880165489482579047E-16, -1.000000000000000000, -0.000000000000000000 ) ) ;
#1042 = ORIENTED_EDGE ( 'NONE', *, *, #30616, .F. ) ;
#1043 = CARTESIAN_POINT ( 'NONE',  ( 755.5913626894240451, -397.6454272087885329, -346.6156483768012890 ) ) ;
#1044 = CARTESIAN_POINT ( 'NONE',  ( 989.9999999999992042, -590.0000000000001137, 209.9999999999999716 ) ) ;
#1045 = CARTESIAN_POINT ( 'NONE',  ( 815.3608509340175488, -218.7363362996982232, -341.2497674668889545 ) ) ;
#1046 = CARTESIAN_POINT ( 'NONE',  ( 799.9636004259356241, -70.91815448151683654, 311.2241431872006956 ) ) ;
#1047 = CIRCLE ( 'NONE', #22428, 8.024999999999948841 ) ;
#1049 = DIRECTION ( 'NONE',  ( -0.000000000000000000, 1.000000000000000000, -0.000000000000000000 ) ) ;
#1048 = DIRECTION ( 'NONE',  ( -0.000000000000000000, -0.000000000000000000, 1.000000000000000000 ) ) ;
#1050 = CARTESIAN_POINT ( 'NONE',  ( 763.2154366446407039, -333.6237781080502600, -321.4292242960311228 ) ) ;
#1051 = FACE_OUTER_BOUND ( 'NONE', #38699, .T. ) ;
#1052 = CARTESIAN_POINT ( 'NONE',  ( 771.3260364891663130, -187.6454272087892434, -306.0683387631859773 ) ) ;
#1053 = CARTESIAN_POINT ( 'NONE',  ( -829.9999999999992042, 529.9999999999997726, -244.9999999999999716 ) ) ;
#1054 = FACE_BOUND ( 'NONE', #24359, .T. ) ;
#1055 = CARTESIAN_POINT ( 'NONE',  ( 757.4527132478984868, -400.3726999360612808, 329.1273215169538844 ) ) ;
#1056 = VECTOR ( 'NONE', #20439, 1000.000000000000000 ) ;
#1057 = CARTESIAN_POINT ( 'NONE',  ( 744.7301800767020268, -244.8164208402379245, -337.4774526936615189 ) ) ;
#1058 = CARTESIAN_POINT ( 'NONE',  ( -39.63011601220123481, -513.1383975375929367, -369.9999999999999432 ) ) ;
#1059 = CARTESIAN_POINT ( 'NONE',  ( 778.2165204200184689, -22.81642084023865280, -364.9363028652563230 ) ) ;
#1060 = CARTESIAN_POINT ( 'NONE',  ( 805.6418435158337843, -173.4636090269710849, 363.8556311672236916 ) ) ;
#1061 = CARTESIAN_POINT ( 'NONE',  ( 778.7502325331095108, -120.3510508353236048, -304.6391490659818828 ) ) ;
#1062 = CARTESIAN_POINT ( 'NONE',  ( 811.0346526505616112, -134.6346026584201070, 323.0537975583477532 ) ) ;
#1063 = CARTESIAN_POINT ( 'NONE',  ( 777.5031285880264704, -358.8164208402375834, -374.9108240113588408 ) ) ;
#1064 = CARTESIAN_POINT ( 'NONE',  ( 775.4999999999993179, -544.8427095258973623, -369.9999999999999432 ) ) ;
#1065 = DIRECTION ( 'NONE',  ( 0.000000000000000000, 0.000000000000000000, 1.000000000000000000 ) ) ;
#1066 = CARTESIAN_POINT ( 'NONE',  ( 797.6776695296629214, -211.5436935675107861, 357.6776695296636603 ) ) ;
#1067 = AXIS2_PLACEMENT_3D ( 'NONE', #33139, #27331, #40964 ) ;
#1068 = VECTOR ( 'NONE', #44629, 1000.000000000000000 ) ;
#1069 = CARTESIAN_POINT ( 'NONE',  ( 800.9840315886518738, -28.91815448151699286, 354.1144889064786412 ) ) ;
#1070 = CARTESIAN_POINT ( 'NONE',  ( 747.3154664389472828, -403.9874144716863498, -326.4474001241230781 ) ) ;
#1071 = CARTESIAN_POINT ( 'NONE',  ( 810.7187646348534145, -450.4527844766009821, -356.7737145352016341 ) ) ;
#1072 = CARTESIAN_POINT ( 'NONE',  ( 779.9999999999992042, 126.4563064324884465, 339.9999999999999432 ) ) ;
#1073 = CARTESIAN_POINT ( 'NONE',  ( 793.4146539503750546, -25.98741447168755769, 307.6481478633938877 ) ) ;
#1074 = ORIENTED_EDGE ( 'NONE', *, *, #6356, .T. ) ;
#1075 = CARTESIAN_POINT ( 'NONE',  ( 766.7756240680305382, -182.5328690171416497, -361.5560724626415663 ) ) ;
#1076 = CARTESIAN_POINT ( 'NONE',  ( 781.7834795799800531, -10.81642084023869543, 315.0636971347436202 ) ) ;
#1077 = CARTESIAN_POINT ( 'NONE',  ( 759.8311093483677041, -238.1692326535050768, -310.9282345327691814 ) ) ;
#1078 = CARTESIAN_POINT ( 'NONE',  ( 761.9338519418445230, -350.5328690171411381, 370.4231160770881957 ) ) ;
#1079 = CARTESIAN_POINT ( 'NONE',  ( 785.3141322388236176, -165.7255117493291152, 364.4286716492789537 ) ) ;
#1080 = EDGE_LOOP ( 'NONE', ( #33357, #6990 ) ) ;
#1081 = CARTESIAN_POINT ( 'NONE',  ( 744.9990715423526808, -426.3510508353226669, 341.2370466360926002 ) ) ;
#1082 = CARTESIAN_POINT ( 'NONE',  ( 785.3687786644884454, -155.3618753856927128, -315.3201227861279676 ) ) ;
#1083 = CARTESIAN_POINT ( 'NONE',  ( 803.4237431249931660, -351.1800572038740142, 331.2633955100225194 ) ) ;
#1084 = AXIS2_PLACEMENT_3D ( 'NONE', #12147, #33380, #29263 ) ;
#1085 = CARTESIAN_POINT ( 'NONE',  ( 772.5602148656447525, -57.72551174932945628, -305.7998596910095443 ) ) ;
#1086 = ORIENTED_EDGE ( 'NONE', *, *, #38685, .T. ) ;
#1087 = CARTESIAN_POINT ( 'NONE',  ( 807.2620300519052989, -432.0090635724247932, -318.0141637701419768 ) ) ;
#1088 = ORIENTED_EDGE ( 'NONE', *, *, #17337, .F. ) ;
#1089 = CARTESIAN_POINT ( 'NONE',  ( 805.2837595273609850, -314.7363362996979959, -340.5290396650784714 ) ) ;
#1090 = ITEM_DEFINED_TRANSFORMATION ( 'NONE', 'NONE', #3913,  #26858 ) ;
#1092 = CARTESIAN_POINT ( 'NONE',  ( 801.5560724626406000, -360.5545181178796383, 326.7756240680316182 ) ) ;
#1091 = CARTESIAN_POINT ( 'NONE',  ( 785.3141322388236176, -69.72551174932942786, 364.4286716492789537 ) ) ;
#1093 = CARTESIAN_POINT ( 'NONE',  ( 802.1676090361156639, -278.6346026584196807, -327.8955696845344505 ) ) ;
#1095 = CARTESIAN_POINT ( 'NONE',  ( 786.2056067578752163, -275.8055962898685038, 374.4686193811670023 ) ) ;
#1094 = CARTESIAN_POINT ( 'NONE',  ( 767.7687537140311633, -383.9073299311466485, 372.7932403749916830 ) ) ;
#1096 = CARTESIAN_POINT ( 'NONE',  ( 788.7631598425961101, -97.44195992623281199, 305.7194118038759143 ) ) ;
#1097 = CARTESIAN_POINT ( 'NONE',  ( 769.0155153010367712, -274.3726999360617356, -362.7791456095907279 ) ) ;
#1098 = CARTESIAN_POINT ( 'NONE',  ( 759.9864689768902508, -290.0891481129650629, -354.9819416627836404 ) ) ;
#1099 = CARTESIAN_POINT ( 'NONE',  ( 181.1634899080285948, 260.0000000000000000, -199.9999999999953957 ) ) ;
#1100 = CARTESIAN_POINT ( 'NONE',  ( 797.8594530101008786, -157.5436935675108998, -322.1405469898980982 ) ) ;
#1101 = PLANE ( 'NONE',  #32125 ) ;
#1102 = ORIENTED_EDGE ( 'NONE', *, *, #32866, .T. ) ;
#1103 = AXIS2_PLACEMENT_3D ( 'NONE', #14608, #33065, #18972 ) ;
#1105 = CARTESIAN_POINT ( 'NONE',  ( 767.9999999999992042, 205.0000000000000568, 319.9999999999999432 ) ) ;
#1104 = DIRECTION ( 'NONE',  ( 0.000000000000000000, 0.7517448203044204691, 0.6594541114781790059 ) ) ;
#1106 = CARTESIAN_POINT ( 'NONE',  ( 815.3608509340175488, -98.73633629969859271, -341.2497674668889545 ) ) ;
#1107 = LINE ( 'NONE', #18453, #27055 ) ;
#1108 = FACE_OUTER_BOUND ( 'NONE', #17628, .T. ) ;
#1109 = CARTESIAN_POINT ( 'NONE',  ( 760.7433823573367135, -300.0090635724252479, 355.9930595647440441 ) ) ;
#1110 = CARTESIAN_POINT ( 'NONE',  ( 785.3141322388236176, -165.7255117493291152, 364.4286716492789537 ) ) ;
#1111 = VERTEX_POINT ( 'NONE', #27142 ) ;
#1112 = CARTESIAN_POINT ( 'NONE',  ( 763.2262854647970016, -128.6346026584201354, -309.2812353651462445 ) ) ;
#1113 = CARTESIAN_POINT ( 'NONE',  ( 786.6156483768007774, -337.4419599262319593, 315.5913626894246136 ) ) ;
#1114 = CARTESIAN_POINT ( 'NONE',  ( 746.4999999999993179, -355.4967352946684969, -16.45562775363632113 ) ) ;
#1115 = AXIS2_PLACEMENT_3D ( 'NONE', #34295, #31290, #10275 ) ;
#1116 = CARTESIAN_POINT ( 'NONE',  ( 786.2694204179717872, -69.28179084515321051, 305.1769319972829067 ) ) ;
#1117 = CARTESIAN_POINT ( 'NONE',  ( 800.9747183278959710, -252.9982390220560831, -311.9810565676471583 ) ) ;
#1118 = VECTOR ( 'NONE', #10969, 1000.000000000000000 ) ;
#1119 = CONICAL_SURFACE ( 'NONE', #17339, 8.024999999999948841, 0.7853981633974337351 ) ;
#1120 = CARTESIAN_POINT ( 'NONE',  ( 758.0580252608178853, -102.4527844766020337, 328.0187753319985404 ) ) ;
#1121 = SURFACE_SIDE_STYLE ('',( #15233 ) ) ;
#1122 = CARTESIAN_POINT ( 'NONE',  ( 815.0009284576459549, -318.3510508353230080, -338.7629533639073429 ) ) ;
#1123 = CARTESIAN_POINT ( 'NONE',  ( 805.2837595273609850, -2.736336299698892027, 340.5290396650784714 ) ) ;
#1124 = CARTESIAN_POINT ( 'NONE',  ( 777.5031285880264704, -358.8164208402375834, -374.9108240113588408 ) ) ;
#1125 = DIRECTION ( 'NONE',  ( 0.000000000000000000, 0.000000000000000000, -1.000000000000000000 ) ) ;
#1126 = CARTESIAN_POINT ( 'NONE',  ( 760.5453621957607311, -405.0783235625954148, 323.8424801807151425 ) ) ;
#1127 = EDGE_LOOP ( 'NONE', ( #7257, #34123, #1263, #14595 ) ) ;
#1128 = CARTESIAN_POINT ( 'NONE',  ( 758.0580252608178853, -414.4527844766010389, -328.0187753319985404 ) ) ;
#1129 = AXIS2_PLACEMENT_3D ( 'NONE', #37239, #8853, #9534 ) ;
#1130 = CARTESIAN_POINT ( 'NONE',  ( 803.6646147819161570, -209.9073299311470748, -348.8264449731210561 ) ) ;
#1131 = ADVANCED_FACE ( 'NONE', ( #12811 ), #6108, .T. ) ;
#1132 = AXIS2_PLACEMENT_3D ( 'NONE', #28850, #42931, #11297 ) ;
#1133 = CARTESIAN_POINT ( 'NONE',  ( 808.7758568127978833, -100.1692326535055315, -320.0363995740631822 ) ) ;
#1134 = CARTESIAN_POINT ( 'NONE',  ( 51.16348990802859475, 260.0000000000000568, -199.9999999999945146 ) ) ;
#1135 = CARTESIAN_POINT ( 'NONE',  ( 801.9858362298568863, -243.0783235625959833, 312.7379699480935642 ) ) ;
#1136 = CARTESIAN_POINT ( 'NONE',  ( 803.4237431249931660, -63.18005720387488822, 331.2633955100225194 ) ) ;
#1137 = AXIS2_PLACEMENT_3D ( 'NONE', #35687, #24841, #32239 ) ;
#1138 = ORIENTED_EDGE ( 'NONE', *, *, #33206, .F. ) ;
#1139 = CARTESIAN_POINT ( 'NONE',  ( 803.8651313633788504, -221.2601417444142271, -332.4468031744301015 ) ) ;
#1140 = CARTESIAN_POINT ( 'NONE',  ( 771.2633955100217236, -239.9073299311470748, 363.4237431249939618 ) ) ;
#1141 = AXIS2_PLACEMENT_3D ( 'NONE', #10530, #3393, #38486 ) ;
#1142 = CARTESIAN_POINT ( 'NONE',  ( 749.8865473780648472, -68.53286901714197654, -322.1177392798429082 ) ) ;
#1143 = AXIS2_PLACEMENT_3D ( 'NONE', #37634, #44811, #30468 ) ;
#1144 = CARTESIAN_POINT ( 'NONE',  ( 805.7454966640377734, -452.9681489794450044, -346.1170114844039745 ) ) ;
#1145 = ORIENTED_EDGE ( 'NONE', *, *, #10271, .T. ) ;
#1146 = CARTESIAN_POINT ( 'NONE',  ( 765.8855110935204493, -70.16923265350563099, 319.0159684113471599 ) ) ;
#1147 = CARTESIAN_POINT ( 'NONE',  ( 804.1009440267234822, -359.4636090269705164, -314.0944755984392600 ) ) ;
#1148 = AXIS2_PLACEMENT_3D ( 'NONE', #41013, #19989, #15837 ) ;
#1149 = VECTOR ( 'NONE', #41633, 1000.000000000000000 ) ;
#1150 = CARTESIAN_POINT ( 'NONE',  ( 754.9967657858570647, -289.5436935675105019, 365.0032342141425943 ) ) ;
#1151 = CARTESIAN_POINT ( 'NONE',  ( 778.7502325331095108, -24.35105083532392811, 304.6391490659818828 ) ) ;
#1152 = CARTESIAN_POINT ( 'NONE',  ( 763.8424801807145741, -186.0090635724255890, -320.5453621957614700 ) ) ;
#1153 = CARTESIAN_POINT ( 'NONE',  ( 759.7806653035534055, -174.9982390220563673, -324.8639956371180801 ) ) ;
#1154 = CARTESIAN_POINT ( 'NONE',  ( 802.1676090361155502, -374.6346026584193396, -327.8955696845344505 ) ) ;
#1155 = VERTEX_POINT ( 'NONE', #15822 ) ;
#1156 = CARTESIAN_POINT ( 'NONE',  ( 765.8855110935204493, 25.83076734649409545, -319.0159684113471599 ) ) ;
#1157 = ORIENTED_EDGE ( 'NONE', *, *, #3258, .T. ) ;
#1158 = CARTESIAN_POINT ( 'NONE',  ( 763.0537975583475827, -312.4527844766012663, 371.0346526505627480 ) ) ;
#1159 = LINE ( 'NONE', #8320, #2670 ) ;
#1160 = CARTESIAN_POINT ( 'NONE',  ( 803.2186876482843445, -367.9874144716865203, 350.0220218866286928 ) ) ;
#1161 = DIRECTION ( 'NONE',  ( -0.000000000000000000, -1.110223024625155554E-15, -1.000000000000000000 ) ) ;
#1162 = CARTESIAN_POINT ( 'NONE',  ( 802.5472867521000353, -196.3726999360619061, 350.8726784830461156 ) ) ;
#1163 = CARTESIAN_POINT ( 'NONE',  ( 767.8955696845333705, -48.45278447660219712, 362.1676090361162323 ) ) ;
#1164 = ORIENTED_EDGE ( 'NONE', *, *, #21005, .T. ) ;
#1165 = CARTESIAN_POINT ( 'NONE',  ( 749.5768839229115201, -420.5545181178793541, -358.0661480581553064 ) ) ;
#1166 = CARTESIAN_POINT ( 'NONE',  ( 767.6429770376291799, -9.180057203875058747, -306.8695393053162093 ) ) ;
#1167 = CARTESIAN_POINT ( 'NONE',  ( 773.3843516231979720, -205.4419599262324425, 364.4086373105754433 ) ) ;
#1168 = AXIS2_PLACEMENT_3D ( 'NONE', #303, #36103, #29173 ) ;
#1169 = CARTESIAN_POINT ( 'NONE',  ( 771.1735550268778070, -393.1800572038737300, -316.3353852180827630 ) ) ;
#1170 = CARTESIAN_POINT ( 'NONE',  ( 804.6798772138710092, 8.274488250670337663, -334.6312213355106451 ) ) ;
#1171 = CARTESIAN_POINT ( 'NONE',  ( 799.2566176426618085, -456.0090635724247932, 324.0069404352559559 ) ) ;
#1172 = DIRECTION ( 'NONE',  ( 0.000000000000000000, 0.000000000000000000, -1.000000000000000000 ) ) ;
#1173 = CARTESIAN_POINT ( 'NONE',  ( 787.5531968255692163, -261.8272453906071746, -316.1348686366205811 ) ) ;
#1174 = AXIS2_PLACEMENT_3D ( 'NONE', #4069, #8002, #22282 ) ;
#1175 = CARTESIAN_POINT ( 'NONE',  ( 759.0252816721024374, -48.99823902205675807, 368.0189434323527280 ) ) ;
#1176 = CARTESIAN_POINT ( 'NONE',  ( 804.7487373415286811, -91.54369356751116982, 364.7487373415288516 ) ) ;
#1177 = FACE_BOUND ( 'NONE', #29400, .T. ) ;
#1178 = VECTOR ( 'NONE', #33127, 1000.000000000000114 ) ;
#1179 = CARTESIAN_POINT ( 'NONE',  ( 813.5763878283155464, -387.8272453906067767, 351.1614460488615350 ) ) ;
#1180 = CARTESIAN_POINT ( 'NONE',  ( -468.8365100919714337, 256.5000000000001705, -202.7499999999907914 ) ) ;
#1181 = CARTESIAN_POINT ( 'NONE',  ( 814.9108240113580450, -352.2709662947830225, 337.5031285880265273 ) ) ;
#1182 = EDGE_CURVE ( 'NONE', #41190, #5430, #42343, .T. ) ;
#1183 = CARTESIAN_POINT ( 'NONE',  ( 802.1676090361156639, -302.6346026584196238, -327.8955696845344505 ) ) ;
#1184 = VECTOR ( 'NONE', #2168, 1000.000000000000000 ) ;
#1185 = CARTESIAN_POINT ( 'NONE',  ( 789.9200121543843807, 22.01258552831228599, 317.0176451133914384 ) ) ;
#1186 = CARTESIAN_POINT ( 'NONE',  ( 755.3028492785439312, -183.2817908451528695, 335.9200461376539693 ) ) ;
#1187 = CARTESIAN_POINT ( 'NONE',  ( 814.4686193811664907, -51.28179084515328867, -346.2056067578752732 ) ) ;
#1188 = CARTESIAN_POINT ( 'NONE',  ( 796.7845633553578182, -105.6237781080509421, -358.5707757039688204 ) ) ;
#1189 = CARTESIAN_POINT ( 'NONE',  ( 773.7943932421234194, -143.8055962898690154, 305.5313806188329409 ) ) ;
#1190 = CARTESIAN_POINT ( 'NONE',  ( 768.0187753319979720, -440.6346026584191122, 318.0580252608186242 ) ) ;
#1191 = CARTESIAN_POINT ( 'NONE',  ( 746.7653713866222915, -161.2601417444143976, 351.0478386215610271 ) ) ;
#1192 = CARTESIAN_POINT ( 'NONE',  ( 801.9419747391806368, -18.45278447660230725, -351.9812246680014027 ) ) ;
#1193 = CARTESIAN_POINT ( 'NONE',  ( 772.3691319403857278, -119.2601417444145397, -315.8894580844506663 ) ) ;
#1194 = CARTESIAN_POINT ( 'NONE',  ( 788.7366044899766848, -131.9073299311473875, -316.5762568750059813 ) ) ;
#1195 = CARTESIAN_POINT ( 'NONE',  ( 786.6156483768007774, -433.4419599262316183, -315.5913626894246136 ) ) ;
#1197 = CARTESIAN_POINT ( 'NONE',  ( 781.8018195045267476, -262.2709662947832499, 365.1927285166407273 ) ) ;
#1196 = CARTESIAN_POINT ( 'NONE',  ( 781.8018195045266339, -262.2709662947831930, 365.1927285166406705 ) ) ;
#1198 = PLANE ( 'NONE',  #4293 ) ;
#1199 = EDGE_LOOP ( 'NONE', ( #16946, #35690 ) ) ;
#1200 = CARTESIAN_POINT ( 'NONE',  ( 804.9511171171677688, 18.19440371013048008, 335.8780910478229202 ) ) ;
#1201 = ORIENTED_EDGE ( 'NONE', *, *, #10607, .T. ) ;
#1202 =( LENGTH_UNIT ( ) NAMED_UNIT ( * ) SI_UNIT ( .MILLI., .METRE. ) );
#1203 = AXIS2_PLACEMENT_3D ( 'NONE', #24325, #16957, #10469 ) ;
#1204 = CARTESIAN_POINT ( 'NONE',  ( 745.0891759886404770, -196.2709662947835909, 342.4968714119734159 ) ) ;
#1205 = CARTESIAN_POINT ( 'NONE',  ( 760.7433823573367135, -276.0090635724253048, 355.9930595647440441 ) ) ;
#1206 = ORIENTED_EDGE ( 'NONE', *, *, #37580, .T. ) ;
#1207 = CARTESIAN_POINT ( 'NONE',  ( 784.1219089521767955, -93.28179084515315367, -315.0488828828318333 ) ) ;
#1208 = CARTESIAN_POINT ( 'NONE',  ( 793.4146539503750546, -217.9874144716870035, 307.6481478633938877 ) ) ;
#1209 = CARTESIAN_POINT ( 'NONE',  ( 781.8018195045267476, -286.2709662947833067, -365.1927285166407273 ) ) ;
#1210 = ORIENTED_EDGE ( 'NONE', *, *, #20424, .F. ) ;
#1211 = CARTESIAN_POINT ( 'NONE',  ( 765.0180583372156207, -384.9982390220556567, -360.0135310231089534 ) ) ;
#1212 = CARTESIAN_POINT ( 'NONE',  ( 803.6646147819161570, -65.90732993114758642, -348.8264449731210561 ) ) ;
#1213 = CARTESIAN_POINT ( 'NONE',  ( 757.2208543904082489, -256.7146871989595525, 350.9844846989624330 ) ) ;
#1214 = FACE_BOUND ( 'NONE', #39130, .T. ) ;
#1215 = FACE_OUTER_BOUND ( 'NONE', #4489, .T. ) ;
#1216 = AXIS2_PLACEMENT_3D ( 'NONE', #36940, #8992, #29784 ) ;
#1217 = CARTESIAN_POINT ( 'NONE',  ( 813.5763878283155464, -27.82724539060790292, -351.1614460488615350 ) ) ;
#1218 = CARTESIAN_POINT ( 'NONE',  ( -728.8365100919714905, 260.0000000000001705, -199.9999999999890861 ) ) ;
#1219 = ORIENTED_EDGE ( 'NONE', *, *, #41907, .T. ) ;
#1220 = CARTESIAN_POINT ( 'NONE',  ( 788.6739635108323228, -319.6454272087888739, -373.9316612368139090 ) ) ;
#1221 = CARTESIAN_POINT ( 'NONE',  ( 750.9282345327678740, -160.9181544815165807, 319.8311093483690115 ) ) ;
#1223 = CARTESIAN_POINT ( 'NONE',  ( 788.8264449731200330, -261.1800572038741848, -363.6646147819171233 ) ) ;
#1222 = DIRECTION ( 'NONE',  ( -1.000000000000000000, -0.000000000000000000, 0.000000000000000000 ) ) ;
#1224 = DIRECTION ( 'NONE',  ( -0.000000000000000000, -0.000000000000000000, -1.000000000000000000 ) ) ;
#1225 = CARTESIAN_POINT ( 'NONE',  ( 787.5531968255692163, -141.8272453906075157, -316.1348686366205811 ) ) ;
#1226 = EDGE_CURVE ( 'NONE', #32683, #45635, #5657, .T. ) ;
#1227 = CARTESIAN_POINT ( 'NONE',  ( 792.2312462859673587, -11.90732993114778182, 307.2067596250082602 ) ) ;
#1228 = DIRECTION ( 'NONE',  ( 0.000000000000000000, 0.000000000000000000, -1.000000000000000000 ) ) ;
#1229 = CARTESIAN_POINT ( 'NONE',  ( 815.0009284576459549, -6.351050835323991173, -338.7629533639073429 ) ) ;
#1230 = CARTESIAN_POINT ( 'NONE',  ( 758.8095938919644823, -344.0891481129648355, -311.6929314249762797 ) ) ;
#1231 = DIRECTION ( 'NONE',  ( 1.000000000000000000, 0.000000000000000000, 0.000000000000000000 ) ) ;
#1232 = CARTESIAN_POINT ( 'NONE',  ( 774.6858677611749044, -33.72551174932952733, 315.5713283507209894 ) ) ;
#1233 = CARTESIAN_POINT ( 'NONE',  ( 773.7305795820266212, -297.2817908451526137, 374.8230680027170365 ) ) ;
#1234 = CARTESIAN_POINT ( 'NONE',  ( 754.0944755984390895, -231.6237781080504874, -364.1009440267246760 ) ) ;
#1235 = AXIS2_PLACEMENT_3D ( 'NONE', #25558, #24866, #4321 ) ;
#1236 = CARTESIAN_POINT ( 'NONE',  ( 747.2067596250078623, -243.1800572038743269, 352.2312462859687230 ) ) ;
#1237 = CARTESIAN_POINT ( 'NONE',  ( 812.7932403749906598, 8.819942796124882634, -327.7687537140311633 ) ) ;
#1238 = AXIS2_PLACEMENT_3D ( 'NONE', #7481, #21783, #18105 ) ;
#1239 = EDGE_CURVE ( 'NONE', #18073, #20679, #43780, .T. ) ;
#1240 = LINE ( 'NONE', #4488, #19538 ) ;
#1241 = EDGE_LOOP ( 'NONE', ( #15487, #34240, #2964, #23570 ) ) ;
#1242 = CARTESIAN_POINT ( 'NONE',  ( 792.1044303154645831, -324.4527844766013231, 317.8323909638837677 ) ) ;
#1243 = AXIS2_PLACEMENT_3D ( 'NONE', #9404, #29728, #29961 ) ;
#1244 = CARTESIAN_POINT ( 'NONE',  ( 801.5560724626406000, -72.55451811788049099, 326.7756240680316182 ) ) ;
#1245 = CARTESIAN_POINT ( 'NONE',  ( 763.2154366446407039, -21.62377810805121570, -321.4292242960311228 ) ) ;
#1246 = VECTOR ( 'NONE', #42062, 1000.000000000000000 ) ;
#1247 = LINE ( 'NONE', #26404, #9266 ) ;
#1248 = CARTESIAN_POINT ( 'NONE',  ( 799.9999999999993179, 166.4563064324884465, 360.0000000000000000 ) ) ;
#1250 = CARTESIAN_POINT ( 'NONE',  ( 774.6858677611749044, -393.7255117493283478, 315.5713283507209894 ) ) ;
#1249 = CARTESIAN_POINT ( 'NONE',  ( 755.0488828828309806, -161.8055962898689870, 344.1219089521771934 ) ) ;
#1251 = ORIENTED_EDGE ( 'NONE', *, *, #3202, .T. ) ;
#1252 = AXIS2_PLACEMENT_3D ( 'NONE', #35298, #45241, #3675 ) ;
#1253 = CARTESIAN_POINT ( 'NONE',  ( 764.0069404352550464, -327.0783235625956991, -359.2566176426627180 ) ) ;
#1254 = CARTESIAN_POINT ( 'NONE',  ( 792.1044303154645831, -156.4527844766018916, 317.8323909638837677 ) ) ;
#1255 = CARTESIAN_POINT ( 'NONE',  ( 803.8556311672234642, -321.6237781080502600, -365.6418435158340117 ) ) ;
#1256 = CARTESIAN_POINT ( 'NONE',  ( 919.9999999999993179, 219.9999999999998863, 339.9999999999999432 ) ) ;
#1257 = CARTESIAN_POINT ( 'NONE',  ( 798.0661480581538854, -434.5328690171407970, 309.5768839229118043 ) ) ;
#1258 = ADVANCED_FACE ( 'NONE', ( #30594 ), #30141, .T. ) ;
#1259 = ORIENTED_EDGE ( 'NONE', *, *, #45039, .T. ) ;
#1260 = CARTESIAN_POINT ( 'NONE',  ( 804.6798772138708955, -375.7255117493283478, 334.6312213355107019 ) ) ;
#1261 = EDGE_CURVE ( 'NONE', #23899, #3360, #19287, .T. ) ;
#1262 = CARTESIAN_POINT ( 'NONE',  ( 789.9200121543843807, -73.98741447168741558, -317.0176451133914384 ) ) ;
#1263 = ORIENTED_EDGE ( 'NONE', *, *, #19291, .T. ) ;
#1264 = CARTESIAN_POINT ( 'NONE',  ( -208.8365100919714052, 240.0000000000001137, -199.9999999999926956 ) ) ;
#1265 = CARTESIAN_POINT ( 'NONE',  ( 787.4397851343537695, -189.7255117493290300, -374.2001403089903988 ) ) ;
#1266 = EDGE_CURVE ( 'NONE', #33715, #16430, #19508, .T. ) ;
#1267 = EDGE_LOOP ( 'NONE', ( #32695, #4959, #6707, #37329 ) ) ;
#1268 = CARTESIAN_POINT ( 'NONE',  ( 797.8594530101009923, -181.5436935675108430, -322.1405469898982119 ) ) ;
#1269 = ORIENTED_EDGE ( 'NONE', *, *, #27496, .T. ) ;
#1270 = AXIS2_PLACEMENT_3D ( 'NONE', #40692, #30517, #33770 ) ;
#1271 = CARTESIAN_POINT ( 'NONE',  ( 805.2837595273609850, -434.7363362996975980, -340.5290396650784714 ) ) ;
#1272 = CARTESIAN_POINT ( 'NONE',  ( 758.0580252608178853, -6.452784476602343666, 328.0187753319985404 ) ) ;
#1273 = CARTESIAN_POINT ( 'NONE',  ( 803.8651313633788504, -149.2601417444144261, 332.4468031744301015 ) ) ;
#1274 = AXIS2_PLACEMENT_3D ( 'NONE', #17291, #20745, #24904 ) ;
#1276 = DIRECTION ( 'NONE',  ( 1.000000000000000000, 0.000000000000000000, 0.000000000000000000 ) ) ;
#1275 = FACE_BOUND ( 'NONE', #36919, .T. ) ;
#1277 = VERTEX_POINT ( 'NONE', #26450 ) ;
#1278 = CARTESIAN_POINT ( 'NONE',  ( 755.1538015810308480, -446.1908817542429802, -343.0433043558613804 ) ) ;
#1279 = CARTESIAN_POINT ( 'NONE',  ( 919.9999999999993179, 219.9999999999998863, -360.0000000000000000 ) ) ;
#1280 = CARTESIAN_POINT ( 'NONE',  ( 813.5763878283155464, -219.8272453906073167, -351.1614460488615350 ) ) ;
#1281 = CARTESIAN_POINT ( 'NONE',  ( 814.2805881961230625, -73.64542720878957027, 331.2368401574024119 ) ) ;
#1283 = CARTESIAN_POINT ( 'NONE',  ( 454.7528517110261532, -8.550106180308601742E-14, 350.0000000000000000 ) ) ;
#1282 = CARTESIAN_POINT ( 'NONE',  ( 521.6730038022808458, -9.808315785437627339E-14, 339.9999999999999432 ) ) ;
#1284 = EDGE_CURVE ( 'NONE', #36701, #8042, #25367, .T. ) ;
#1285 = CARTESIAN_POINT ( 'NONE',  ( 770.0799878456142551, -325.9874144716865771, -362.9823548866085616 ) ) ;
#1286 = PLANE ( 'NONE',  #12170 ) ;
#1287 = CARTESIAN_POINT ( 'NONE',  ( 764.1737431748507561, -202.3726999360618777, -371.6461892240376415 ) ) ;
#1288 = CYLINDRICAL_SURFACE ( 'NONE', #20808, 2.749999999999863665 ) ;
#1289 = FACE_OUTER_BOUND ( 'NONE', #14899, .T. ) ;
#1290 = CARTESIAN_POINT ( 'NONE',  ( 804.8461984189677878, -410.1908817542430370, 336.9566956441385628 ) ) ;
#1291 = EDGE_CURVE ( 'NONE', #23098, #22606, #40548, .T. ) ;
#1292 = CARTESIAN_POINT ( 'NONE',  ( 813.1304606946831655, -257.9073299311469327, -352.3570229623691716 ) ) ;
#1293 = CARTESIAN_POINT ( 'NONE',  ( 776.9254006560222479, -236.1908817542436338, 314.8983024940802125 ) ) ;
#1294 = DIRECTION ( 'NONE',  ( -0.000000000000000000, -4.857225732735055920E-15, 1.000000000000000000 ) ) ;
#1295 = CARTESIAN_POINT ( 'NONE',  ( 767.8955696845333705, -24.45278447660229304, -362.1676090361162323 ) ) ;
#1296 = CARTESIAN_POINT ( 'NONE',  ( 773.7305795820266212, -177.2817908451528695, 374.8230680027170365 ) ) ;
#1297 = CARTESIAN_POINT ( 'NONE',  ( 805.9055244015594326, -123.6237781080508569, -315.8990559732753240 ) ) ;
#1298 = CARTESIAN_POINT ( 'NONE',  ( 747.2067596250078623, -171.1800572038745543, 352.2312462859687230 ) ) ;
#1299 = CARTESIAN_POINT ( 'NONE',  ( 772.4837098697144029, -383.3618753856921444, -374.5518280994205611 ) ) ;
#1300 = EDGE_CURVE ( 'NONE', #38426, #11372, #5435, .T. ) ;
#1301 = EDGE_CURVE ( 'NONE', #20106, #32443, #42354, .T. ) ;
#1302 = DIRECTION ( 'NONE',  ( 1.000000000000000000, 0.000000000000000000, 0.000000000000000000 ) ) ;
#1303 = DIRECTION ( 'NONE',  ( 0.000000000000000000, -1.000000000000000000, 0.000000000000000000 ) ) ;
#1304 = CARTESIAN_POINT ( 'NONE',  ( 801.9419747391806368, -210.4527844766016926, 351.9812246680014027 ) ) ;
#1305 = CARTESIAN_POINT ( 'NONE',  ( 755.3028492785439312, -39.28179084515331709, 335.9200461376539693 ) ) ;
#1306 = CARTESIAN_POINT ( 'NONE',  ( 801.9419747391806368, -378.4527844766011526, -351.9812246680014027 ) ) ;
#1307 = CARTESIAN_POINT ( 'NONE',  ( 764.1737431748507561, -10.37269993606250473, -371.6461892240376415 ) ) ;
#1308 = CARTESIAN_POINT ( 'NONE',  ( 1820.038553321469863, -407.8586036264140375, -201.9999999999998863 ) ) ;
#1309 = CARTESIAN_POINT ( 'NONE',  ( 810.1134526219336749, -32.53286901714208312, 357.8822607201570349 ) ) ;
#1310 = ORIENTED_EDGE ( 'NONE', *, *, #3849, .F. ) ;
#1311 = CARTESIAN_POINT ( 'NONE',  ( 803.2186876482843445, -175.9874144716871172, -350.0220218866286928 ) ) ;
#1312 = CARTESIAN_POINT ( 'NONE',  ( 803.4237431249931660, -15.18005720387504631, 331.2633955100225194 ) ) ;
#1313 = CARTESIAN_POINT ( 'NONE',  ( 764.3348316497523456, -214.7146871989597230, -308.6759233522265617 ) ) ;
#1314 = CARTESIAN_POINT ( 'NONE',  ( 788.7631598425961101, -361.4419599262319593, 305.7194118038759143 ) ) ;
#1315 = ORIENTED_EDGE ( 'NONE', *, *, #3538, .F. ) ;
#1316 = CARTESIAN_POINT ( 'NONE',  ( 747.3154664389472828, -427.9874144716862929, 326.4474001241230781 ) ) ;
#1317 = CARTESIAN_POINT ( 'NONE',  ( 778.2165204200184689, -142.8164208402382656, -364.9363028652563230 ) ) ;
#1318 = CARTESIAN_POINT ( 'NONE',  ( 804.6798772138708955, -327.7255117493285184, 334.6312213355107019 ) ) ;
#1319 = CARTESIAN_POINT ( 'NONE',  ( 772.4837098697144029, -95.36187538569294020, -374.5518280994205611 ) ) ;
#1320 = ORIENTED_EDGE ( 'NONE', *, *, #28389, .T. ) ;
#1321 = CARTESIAN_POINT ( 'NONE',  ( 773.4516893846965786, -19.64542720878974791, -315.8398074228977066 ) ) ;
#1322 = ORIENTED_EDGE ( 'NONE', *, *, #35586, .F. ) ;
#1323 = CARTESIAN_POINT ( 'NONE',  ( 802.9823548866075953, -313.0999726633342561, -330.0799878456151077 ) ) ;
#1325 = CARTESIAN_POINT ( 'NONE',  ( 755.3028492785439312, -375.2817908451523294, 335.9200461376539693 ) ) ;
#1324 = CARTESIAN_POINT ( 'NONE',  ( 788.7366044899766848, -59.90732993114762905, 316.5762568750059813 ) ) ;
#1326 = CARTESIAN_POINT ( 'NONE',  ( 774.6312213355099630, -311.3618753856922581, -364.6798772138717482 ) ) ;
#1328 = CARTESIAN_POINT ( 'NONE',  ( 815.1787889125755555, -318.8965053807775121, 343.7953271457877804 ) ) ;
#1327 = CARTESIAN_POINT ( 'NONE',  ( 745.0891759886404770, -412.2709662947829088, 342.4968714119734159 ) ) ;
#1329 = CARTESIAN_POINT ( 'NONE',  ( 801.9858362298568863, -99.07832356259642381, 312.7379699480935642 ) ) ;
#1330 = CARTESIAN_POINT ( 'NONE',  ( 790.9844846989617508, -286.3726999360617356, -317.2208543904092721 ) ) ;
#1331 = CARTESIAN_POINT ( 'NONE',  ( 794.9819416627830151, -300.9982390220559409, -319.9864689768909898 ) ) ;
#1332 = LINE ( 'NONE', #25597, #4420 ) ;
#1333 = CARTESIAN_POINT ( 'NONE',  ( 791.9812246680005501, -140.6346026584201070, -361.9419747391813189 ) ) ;
#1334 = CARTESIAN_POINT ( 'NONE',  ( 779.9999999999992042, -462.9681489794448339, -339.9999999999999432 ) ) ;
#1335 = CARTESIAN_POINT ( 'NONE',  ( 814.2001403089898304, -425.3618753856919170, 347.4397851343538264 ) ) ;
#1337 = CARTESIAN_POINT ( 'NONE',  ( -769.9999999999992042, 205.0000000000000568, -339.9999999999999432 ) ) ;
#1336 = CARTESIAN_POINT ( 'NONE',  ( 779.9999999999992042, -452.9681489794448339, -350.0000000000000000 ) ) ;
#1338 = ADVANCED_FACE ( 'NONE', ( #17665 ), #34740, .F. ) ;
#1339 = CARTESIAN_POINT ( 'NONE',  ( 781.2370466360911223, -68.73633629969867798, -304.9990715423533629 ) ) ;
#1340 = PLANE ( 'NONE',  #41833 ) ;
#1341 = DIRECTION ( 'NONE',  ( -0.000000000000000000, 1.000000000000000000, -0.000000000000000000 ) ) ;
#1342 = CARTESIAN_POINT ( 'NONE',  ( 754.7162404726377645, -302.7363362996979959, 339.4709603349214717 ) ) ;
#1343 =( REPRESENTATION_RELATIONSHIP ('NONE','NONE', #39835, #28884 ) REPRESENTATION_RELATIONSHIP_WITH_TRANSFORMATION ( #40122 )SHAPE_REPRESENTATION_RELATIONSHIP( ) );
#1344 = CARTESIAN_POINT ( 'NONE',  ( 785.3687786644884454, -155.3618753856927128, 315.3201227861279676 ) ) ;
#1345 = EDGE_LOOP ( 'NONE', ( #527, #16375 ) ) ;
#1346 = CARTESIAN_POINT ( 'NONE',  ( 749.2812353651451076, -150.4527844766018916, -323.2262854647983090 ) ) ;
#1347 = CARTESIAN_POINT ( 'NONE',  ( 804.9511171171677688, -341.8055962898683333, 335.8780910478229202 ) ) ;
#1348 = VECTOR ( 'NONE', #24622, 1000.000000000000000 ) ;
#1349 = CARTESIAN_POINT ( 'NONE',  ( -521.6730038022808458, 230.0000000000001421, -122.7905160835438068 ) ) ;
#1350 = CARTESIAN_POINT ( 'NONE',  ( 798.7617431975189675, -435.6237781080499190, -323.0428371773161871 ) ) ;
#1351 = CARTESIAN_POINT ( 'NONE',  ( 814.8207195650702488, -74.19088175424410281, 336.2433038121456548 ) ) ;
#1352 = CARTESIAN_POINT ( 'NONE',  ( 787.5162901302840055, -275.3618753856923149, -305.4481719005792684 ) ) ;
#1353 = CARTESIAN_POINT ( 'NONE',  ( 785.3687786644884454, -131.3618753856928834, 315.3201227861279676 ) ) ;
#1354 = ORIENTED_EDGE ( 'NONE', *, *, #44887, .F. ) ;
#1355 = CARTESIAN_POINT ( 'NONE',  ( 805.9055244015594326, -339.6237781080502600, -315.8990559732753240 ) ) ;
#1356 = CARTESIAN_POINT ( 'NONE',  ( 766.9102291470427417, -18.55451811788065797, 318.6633372737382501 ) ) ;
#1357 = CARTESIAN_POINT ( 'NONE',  ( 812.7932403749906598, -351.1800572038740142, -327.7687537140311633 ) ) ;
#1358 = LINE ( 'NONE', #15461, #15140 ) ;
#1359 = CARTESIAN_POINT ( 'NONE',  ( 765.8855110935204493, -382.1692326535045936, 319.0159684113471599 ) ) ;
#1360 = ORIENTED_EDGE ( 'NONE', *, *, #33421, .T. ) ;
#1361 = CARTESIAN_POINT ( 'NONE',  ( 784.0799538623451781, -83.80559628986920018, 364.6971507214555572 ) ) ;
#1362 = CARTESIAN_POINT ( 'NONE',  ( 759.7806653035534055, -414.9982390220555430, -324.8639956371180801 ) ) ;
#1363 = CARTESIAN_POINT ( 'NONE',  ( 813.2346286133761168, -125.2601417444145255, -328.9521613784389160 ) ) ;
#1364 = DIRECTION ( 'NONE',  ( -0.000000000000000000, 1.000000000000000000, -0.000000000000000000 ) ) ;
#1365 = CARTESIAN_POINT ( 'NONE',  ( 798.0661480581538854, -242.5328690171414507, 309.5768839229118043 ) ) ;
#1366 = CARTESIAN_POINT ( 'NONE',  ( 762.3223304703356007, -55.54369356751127640, 322.3223304703362828 ) ) ;
#1367 = ORIENTED_EDGE ( 'NONE', *, *, #16471, .T. ) ;
#1368 = CARTESIAN_POINT ( 'NONE',  ( 793.2243759319678702, -242.5328690171414507, -318.4439275373583200 ) ) ;
#1369 = CARTESIAN_POINT ( 'NONE',  ( 781.7834795799800531, -250.8164208402379245, 315.0636971347436202 ) ) ;
#1370 = CARTESIAN_POINT ( 'NONE',  ( 792.2269492836462632, -443.1233509495419298, -372.8191558162650949 ) ) ;
#1371 = CARTESIAN_POINT ( 'NONE',  ( 748.3538107759620743, -64.71468719896019195, -355.8262568251490165 ) ) ;
#1372 = DIRECTION ( 'NONE',  ( 0.000000000000000000, 0.000000000000000000, -1.000000000000000000 ) ) ;
#1373 = VERTEX_POINT ( 'NONE', #14187 ) ;
#1374 = VERTEX_POINT ( 'NONE', #10723 ) ;
#1375 = CARTESIAN_POINT ( 'NONE',  ( 814.8207195650702488, -386.1908817542432075, -336.2433038121456548 ) ) ;
#1376 = VECTOR ( 'NONE', #35836, 999.9999999999998863 ) ;
#1377 = CARTESIAN_POINT ( 'NONE',  ( 813.1304606946831655, -281.9073299311469327, 352.3570229623691716 ) ) ;
#1378 = CARTESIAN_POINT ( 'NONE',  ( 746.7653713866222915, -41.26014174441479554, 351.0478386215610271 ) ) ;
#1379 = CARTESIAN_POINT ( 'NONE',  ( 800.9840315886518738, -172.9181544815165239, -354.1144889064786412 ) ) ;
#1380 = CARTESIAN_POINT ( 'NONE',  ( 768.0187753319979720, -200.6346026584199365, -318.0580252608186242 ) ) ;
#1381 = CARTESIAN_POINT ( 'NONE',  ( 771.1735550268780344, -393.1800572038737869, -316.3353852180828198 ) ) ;
#1382 = VERTEX_POINT ( 'NONE', #27582 ) ;
#1383 = ORIENTED_EDGE ( 'NONE', *, *, #22701, .F. ) ;
#1384 = CARTESIAN_POINT ( 'NONE',  ( 772.5602148656447525, -321.7255117493286320, 305.7998596910095443 ) ) ;
#1385 = CARTESIAN_POINT ( 'NONE',  ( -521.6730038022808458, 240.0000000000001705, -122.7905160835438068 ) ) ;
#1386 = FACE_OUTER_BOUND ( 'NONE', #24531, .T. ) ;
#1387 = DIRECTION ( 'NONE',  ( -0.000000000000000000, 1.000000000000000000, -0.000000000000000000 ) ) ;
#1388 = CARTESIAN_POINT ( 'NONE',  ( 758.4439275373578084, -204.5545181178800931, 353.2243759319684386 ) ) ;
#1389 = CARTESIAN_POINT ( 'NONE',  ( 778.1981804954714335, -34.27096629478407408, 314.8072714833589885 ) ) ;
#1390 = VERTEX_POINT ( 'NONE', #6570 ) ;
#1391 = CARTESIAN_POINT ( 'NONE',  ( 750.9282345327678740, -424.9181544815158986, -319.8311093483690115 ) ) ;
#1392 = CARTESIAN_POINT ( 'NONE',  ( 745.4481719005789273, -27.72551174932954510, -347.5162901302853697 ) ) ;
#1393 = CARTESIAN_POINT ( 'NONE',  ( 758.6633372737375112, -212.5328690171415076, 326.9102291470432533 ) ) ;
#1394 = CARTESIAN_POINT ( 'NONE',  ( 803.6646147819161570, -401.9073299311463643, -348.8264449731210561 ) ) ;
#1395 = CARTESIAN_POINT ( 'NONE',  ( 755.3201227861273992, -3.725511749329622813, -345.3687786644892981 ) ) ;
#1396 = CARTESIAN_POINT ( 'NONE',  ( 814.9108240113580450, -448.2709662947827951, 337.5031285880265273 ) ) ;
#1397 = CARTESIAN_POINT ( 'NONE',  ( 989.9999999999992042, 249.9999999999998863, 350.0000000000000000 ) ) ;
#1398 = CARTESIAN_POINT ( 'NONE',  ( 758.4439275373578084, -252.5545181178799226, -353.2243759319684386 ) ) ;
#1399 = CARTESIAN_POINT ( 'NONE',  ( 777.4774526936600978, -154.2709662947836478, -304.7301800767027657 ) ) ;
#1400 = CARTESIAN_POINT ( 'NONE',  ( 767.7687537140311633, -47.90732993114767169, 372.7932403749916830 ) ) ;
#1401 = CARTESIAN_POINT ( 'NONE',  ( 754.9967657858570647, -121.5436935675110419, 365.0032342141425374 ) ) ;
#1402 = CARTESIAN_POINT ( 'NONE',  ( 762.3223304703356007, 16.45630643248849267, -322.3223304703362828 ) ) ;
#1403 = CARTESIAN_POINT ( 'NONE',  ( 1238.921997096861332, 240.0000000000000568, -244.9999999999999716 ) ) ;
#1404 = CIRCLE ( 'NONE', #34609, 30.00000000000008171 ) ;
#1405 = CARTESIAN_POINT ( 'NONE',  ( 778.7629533639073998, -392.7363362996977116, 375.0009284576466371 ) ) ;
#1406 = DIRECTION ( 'NONE',  ( 8.659560562354932858E-17, 0.7071067811865474617, -0.7071067811865474617 ) ) ;
#1407 = CARTESIAN_POINT ( 'NONE',  ( 812.7932403749906598, -351.1800572038740142, 327.7687537140311633 ) ) ;
#1408 = CARTESIAN_POINT ( 'NONE',  ( 754.8072714833581358, -316.8164208402377540, -338.1981804954720587 ) ) ;
#1409 = CARTESIAN_POINT ( 'NONE',  ( 794.1144889064781864, 13.83076734649413098, 360.9840315886528401 ) ) ;
#1410 = CARTESIAN_POINT ( 'NONE',  ( 809.0717654672305343, -100.9181544815167513, -360.1688906516309885 ) ) ;
#1411 = CARTESIAN_POINT ( 'NONE',  ( 789.9200121543843807, -121.9874144716872593, -317.0176451133914384 ) ) ;
#1412 = CARTESIAN_POINT ( 'NONE',  ( 808.7758568127978833, -148.1692326535053610, 320.0363995740631822 ) ) ;
#1413 = CARTESIAN_POINT ( 'NONE',  ( 762.1405469898973024, -433.5436935675100472, 357.8594530101016176 ) ) ;
#1414 = CARTESIAN_POINT ( 'NONE',  ( 802.1676090361156639, -14.63460265842049424, -327.8955696845344505 ) ) ;
#1415 = CARTESIAN_POINT ( 'NONE',  ( 784.0799538623451781, -131.8055962898690439, -364.6971507214555572 ) ) ;
#1416 = CARTESIAN_POINT ( 'NONE',  ( 794.9819416627830151, -132.9982390220564810, -319.9864689768909898 ) ) ;
#1417 = CARTESIAN_POINT ( 'NONE',  ( 800.0135310231082713, -134.0891481129655745, 325.0180583372163028 ) ) ;
#1418 = MANIFOLD_SOLID_BREP ( 'Mirror5[3]', #38730 ) ;
#1419 = CARTESIAN_POINT ( 'NONE',  ( 768.8385539511368734, 24.73985825558500551, -306.4236121716840557 ) ) ;
#1421 = CARTESIAN_POINT ( 'NONE',  ( 755.3201227861273992, -267.7255117493287457, 345.3687786644892981 ) ) ;
#1420 = CARTESIAN_POINT ( 'NONE',  ( 785.3687786644884454, -251.3618753856923149, 315.3201227861279676 ) ) ;
#1422 = CARTESIAN_POINT ( 'NONE',  ( 779.9999999999992042, 16.45630643248849267, 339.9999999999999432 ) ) ;
#1423 = ORIENTED_EDGE ( 'NONE', *, *, #13394, .F. ) ;
#1424 = CARTESIAN_POINT ( 'NONE',  ( 800.2193346964447755, -450.9982390220554294, 355.1360043628815788 ) ) ;
#1425 = ORIENTED_EDGE ( 'NONE', *, *, #20505, .T. ) ;
#1426 = CARTESIAN_POINT ( 'NONE',  ( 800.9747183278959710, -180.9982390220563389, 311.9810565676471583 ) ) ;
#1427 = CARTESIAN_POINT ( 'NONE',  ( 793.9708237608222134, -310.9181544815160123, 319.2295555964448681 ) ) ;
#1428 = CARTESIAN_POINT ( 'NONE',  ( 783.0433043558608688, -384.8965053807772847, 315.1538015810313027 ) ) ;
#1429 = VERTEX_POINT ( 'NONE', #2881 ) ;
#1430 = CARTESIAN_POINT ( 'NONE',  ( 766.9102291470427417, -90.55451811788041994, -318.6633372737382501 ) ) ;
#1431 = CARTESIAN_POINT ( 'NONE',  ( 771.2633955100217236, -287.9073299311468759, -363.4237431249939618 ) ) ;
#1432 = ORIENTED_EDGE ( 'NONE', *, *, #25271, .T. ) ;
#1433 = AXIS2_PLACEMENT_3D ( 'NONE', #27341, #16953, #45130 ) ;
#1434 = CARTESIAN_POINT ( 'NONE',  ( 803.6646147819161570, -377.9073299311466485, -348.8264449731210561 ) ) ;
#1435 = CARTESIAN_POINT ( 'NONE',  ( 764.8639956371174549, -32.08914811296588709, -319.7806653035542013 ) ) ;
#1436 = CARTESIAN_POINT ( 'NONE',  ( 765.8855110935204493, -262.1692326535049347, 319.0159684113471599 ) ) ;
#1437 = DIRECTION ( 'NONE',  ( 0.000000000000000000, 0.000000000000000000, 1.000000000000000000 ) ) ;
#1438 = CARTESIAN_POINT ( 'NONE',  ( 701.1634899080286232, 229.9999999999999147, -199.9999999999990337 ) ) ;
#1439 = CARTESIAN_POINT ( 'NONE',  ( 744.6391490659812007, -14.73633629969885384, -338.7502325331110455 ) ) ;
#1440 = DIRECTION ( 'NONE',  ( 0.000000000000000000, 0.000000000000000000, 1.000000000000000000 ) ) ;
#1441 = VERTEX_POINT ( 'NONE', #34968 ) ;
#1442 = CARTESIAN_POINT ( 'NONE',  ( 745.7194118038753459, -301.6454272087889308, -348.7631598425976449 ) ) ;
#1443 = CARTESIAN_POINT ( 'NONE',  ( 748.6759233522253680, -160.3726999360620482, 324.3348316497537098 ) ) ;
#1445 = CARTESIAN_POINT ( 'NONE',  ( 774.6312213355099630, -287.3618753856923718, -364.6798772138717482 ) ) ;
#1444 = CARTESIAN_POINT ( 'NONE',  ( 939.9999999999993179, -419.8175818341089780, 209.9999999999999716 ) ) ;
#1446 = CARTESIAN_POINT ( 'NONE',  ( 755.8894580844503253, -135.8272453906076009, -332.3691319403863531 ) ) ;
#1447 = CARTESIAN_POINT ( 'NONE',  ( 772.5602148656447525, -9.725511749329603717, 305.7998596910095443 ) ) ;
#1448 = DIRECTION ( 'NONE',  ( -1.880165489482579047E-16, -1.000000000000000000, -0.000000000000000000 ) ) ;
#1449 = CARTESIAN_POINT ( 'NONE',  ( 800.1688906516307043, -10.16923265350579442, -369.0717654672308186 ) ) ;
#1450 = CARTESIAN_POINT ( 'NONE',  ( 796.9462024416508257, -348.4527844766012095, -308.9653473494370246 ) ) ;
#1451 = CARTESIAN_POINT ( 'NONE',  ( 914.9999999999992042, 99.99999999999984368, -350.0000000000000000 ) ) ;
#1452 = CARTESIAN_POINT ( 'NONE',  ( 781.7834795799800531, -34.81642084023861372, 315.0636971347436202 ) ) ;
#1453 = CARTESIAN_POINT ( 'NONE',  ( 754.3581564841646241, -281.4636090269706870, 316.1443688327762516 ) ) ;
#1454 = CARTESIAN_POINT ( 'NONE',  ( 766.5853460496234675, -253.9874144716868329, -372.3518521366060554 ) ) ;
#1455 = CARTESIAN_POINT ( 'NONE',  ( 749.2812353651451076, -246.4527844766016074, 323.2262854647983090 ) ) ;
#1456 = CARTESIAN_POINT ( 'NONE',  ( 813.9316612368132837, -439.4419599262316751, -348.6739635108323228 ) ) ;
#1457 = DIRECTION ( 'NONE',  ( 0.000000000000000000, 1.000000000000000000, 0.000000000000000000 ) ) ;
#1458 = ORIENTED_EDGE ( 'NONE', *, *, #12287, .F. ) ;
#1459 = CARTESIAN_POINT ( 'NONE',  ( 762.3223304703356007, -367.5436935675102745, 322.3223304703362828 ) ) ;
#1460 = CARTESIAN_POINT ( 'NONE',  ( 755.1538015810308480, -134.1908817542439181, 343.0433043558613804 ) ) ;
#1461 = CARTESIAN_POINT ( 'NONE',  ( 801.3366627262608972, -32.53286901714208312, -353.0897708529566899 ) ) ;
#1462 = FACE_OUTER_BOUND ( 'NONE', #18383, .T. ) ;
#1463 = FACE_OUTER_BOUND ( 'NONE', #20948, .T. ) ;
#1464 = CARTESIAN_POINT ( 'NONE',  ( 754.8072714833581358, -388.8164208402374129, 338.1981804954720587 ) ) ;
#1465 = ORIENTED_EDGE ( 'NONE', *, *, #22138, .T. ) ;
#1466 = CARTESIAN_POINT ( 'NONE',  ( 803.2186876482843445, -319.9874144716866340, -350.0220218866286928 ) ) ;
#1467 = CARTESIAN_POINT ( 'NONE',  ( 774.6312213355099630, -143.3618753856927697, 364.6798772138717482 ) ) ;
#1468 = UNCERTAINTY_MEASURE_WITH_UNIT (LENGTH_MEASURE( 1.000000000000000082E-05 ), #40729, 'distance_accuracy_value', 'NONE');
#1469 = CARTESIAN_POINT ( 'NONE',  ( 754.0944755984390895, -327.6237781080502600, -364.1009440267246760 ) ) ;
#1470 = CARTESIAN_POINT ( 'NONE',  ( -769.9999999999992042, 240.0000000000000568, -319.9999999999999432 ) ) ;
#1471 = ORIENTED_EDGE ( 'NONE', *, *, #8622, .T. ) ;
#1472 = CARTESIAN_POINT ( 'NONE',  ( 758.0580252608178853, -366.4527844766012095, 328.0187753319985404 ) ) ;
#1473 = EDGE_LOOP ( 'NONE', ( #35327, #6545 ) ) ;
#1474 = CARTESIAN_POINT ( 'NONE',  ( 765.0180583372156207, -432.9982390220555999, 360.0135310231089534 ) ) ;
#1475 = EDGE_CURVE ( 'NONE', #11526, #30518, #11359, .T. ) ;
#1476 = CARTESIAN_POINT ( 'NONE',  ( 754.9967657858570647, -169.5436935675108430, -365.0032342141425374 ) ) ;
#1477 = CARTESIAN_POINT ( 'NONE',  ( 746.8695393053151292, -77.90732993114757221, 327.6429770376306578 ) ) ;
#1478 = ORIENTED_EDGE ( 'NONE', *, *, #31981, .T. ) ;
#1479 = CARTESIAN_POINT ( 'NONE',  ( 785.3141322388236176, -189.7255117493290300, -364.4286716492789537 ) ) ;
#1480 = ORIENTED_EDGE ( 'NONE', *, *, #43372, .T. ) ;
#1481 = CARTESIAN_POINT ( 'NONE',  ( 784.1219089521767955, -429.2817908451521021, -315.0488828828318333 ) ) ;
#1482 = CARTESIAN_POINT ( 'NONE',  ( 801.5560724626406000, -456.5545181178792404, 326.7756240680316182 ) ) ;
#1483 = CARTESIAN_POINT ( 'NONE',  ( 796.9462024416508257, -228.4527844766015789, 308.9653473494370246 ) ) ;
#1484 = CARTESIAN_POINT ( 'NONE',  ( 754.9735926884551418, -162.3510508353235196, 340.5236548041000333 ) ) ;
#1486 = CARTESIAN_POINT ( 'NONE',  ( 441.1634899080286232, 259.9999999999999432, -199.9999999999972431 ) ) ;
#1485 = DIRECTION ( 'NONE',  ( 0.000000000000000000, -1.000000000000000000, 0.000000000000000000 ) ) ;
#1487 = EDGE_CURVE ( 'NONE', #36764, #29494, #41917, .T. ) ;
#1488 = ORIENTED_EDGE ( 'NONE', *, *, #32844, .T. ) ;
#1489 = CARTESIAN_POINT ( 'NONE',  ( 775.8780910478218402, -441.2817908451521021, -364.9511171171680530 ) ) ;
#1490 = DIRECTION ( 'NONE',  ( 0.000000000000000000, 0.000000000000000000, -1.000000000000000000 ) ) ;
#1491 = CARTESIAN_POINT ( 'NONE',  ( 755.8990559732751535, -203.4636090269709996, -365.9055244015606831 ) ) ;
#1492 = CARTESIAN_POINT ( 'NONE',  ( 773.7305795820266212, -57.28179084515326736, 374.8230680027170365 ) ) ;
#1494 = CARTESIAN_POINT ( 'NONE',  ( 759.7806653035534055, -174.9982390220563673, -324.8639956371180801 ) ) ;
#1493 = DIRECTION ( 'NONE',  ( 0.000000000000000000, 0.000000000000000000, -1.000000000000000000 ) ) ;
#1495 = CARTESIAN_POINT ( 'NONE',  ( 765.8855110935204493, -310.1692326535048778, -319.0159684113471599 ) ) ;
#1496 = CARTESIAN_POINT ( 'NONE',  ( 791.7608162188021197, 205.0000000000000568, 339.9999999999999432 ) ) ;
#1497 = CARTESIAN_POINT ( 'NONE',  ( 812.3518521366052028, -217.0999726633345972, -326.5853460496235243 ) ) ;
#1498 = CARTESIAN_POINT ( 'NONE',  ( 989.9999999999992042, -414.5899773927342835, 209.9999999999999716 ) ) ;
#1499 = PLANE ( 'NONE',  #38589 ) ;
#1500 = CARTESIAN_POINT ( 'NONE',  ( 759.0159684113467620, -40.91815448151695023, -325.8855110935213020 ) ) ;
#1501 = CARTESIAN_POINT ( 'NONE',  ( 800.9840315886518738, -412.9181544815157281, 354.1144889064786412 ) ) ;
#1502 = CARTESIAN_POINT ( 'NONE',  ( 808.3070685750232087, -234.9982390220561683, -361.1904061080339829 ) ) ;
#1503 = CARTESIAN_POINT ( 'NONE',  ( 801.5560724626406000, -240.5545181178798941, 326.7756240680316182 ) ) ;
#1504 = DIRECTION ( 'NONE',  ( 0.000000000000000000, 1.000000000000000000, 0.000000000000000000 ) ) ;
#1505 = CARTESIAN_POINT ( 'NONE',  ( 755.3201227861273992, -27.72551174932954510, -345.3687786644892981 ) ) ;
#1506 = CARTESIAN_POINT ( 'NONE',  ( 804.1009440267234822, -167.4636090269711133, 314.0944755984392600 ) ) ;
#1508 = ADVANCED_FACE ( 'NONE', ( #20430, #38223 ), #24111, .T. ) ;
#1507 = EDGE_CURVE ( 'NONE', #45297, #13477, #40147, .T. ) ;
#1509 = CARTESIAN_POINT ( 'NONE',  ( 808.7758568127978833, -148.1692326535053610, -320.0363995740631822 ) ) ;
#1510 = CARTESIAN_POINT ( 'NONE',  ( 754.9967657858570647, -145.5436935675109851, 365.0032342141425374 ) ) ;
#1511 = CARTESIAN_POINT ( 'NONE',  ( 747.2067596250078623, -363.1800572038739006, -352.2312462859687230 ) ) ;
#1512 = DIRECTION ( 'NONE',  ( 1.000000000000000000, 0.000000000000000000, -0.000000000000000000 ) ) ;
#1513 = DIRECTION ( 'NONE',  ( -1.058954862565134068E-16, 0.6438296778008191223, 0.7651688349527137056 ) ) ;
#1514 = CARTESIAN_POINT ( 'NONE',  ( 781.7834795799800531, -250.8164208402379245, 315.0636971347436202 ) ) ;
#1515 = CARTESIAN_POINT ( 'NONE',  ( 769.9779781133707957, -19.09997266333520116, 316.7813123517150871 ) ) ;
#1516 = CARTESIAN_POINT ( 'NONE',  ( 803.6646147819161570, -377.9073299311466485, -348.8264449731210561 ) ) ;
#1517 = FACE_BOUND ( 'NONE', #4195, .T. ) ;
#1518 = CARTESIAN_POINT ( 'NONE',  ( 776.2046728542105711, 3.809118245755632959, -304.8212110874238761 ) ) ;
#1519 = DIRECTION ( 'NONE',  ( 0.000000000000000000, 1.000000000000000000, 3.700743415417198493E-16 ) ) ;
#1520 = CARTESIAN_POINT ( 'NONE',  ( 803.2186876482843445, -55.98741447168748664, 350.0220218866286928 ) ) ;
#1521 = EDGE_LOOP ( 'NONE', ( #973, #3985, #6124, #36419 ) ) ;
#1522 = CARTESIAN_POINT ( 'NONE',  ( 786.6156483768007774, -217.4419599262324141, -315.5913626894246136 ) ) ;
#1523 = CARTESIAN_POINT ( 'NONE',  ( 774.6312213355099630, -23.36187538569318889, 364.6798772138717482 ) ) ;
#1524 = CARTESIAN_POINT ( 'NONE',  ( 756.1443688327750579, -213.6237781080506011, -314.3581564841659315 ) ) ;
#1525 = DIRECTION ( 'NONE',  ( 1.000000000000000000, -0.000000000000000000, -0.000000000000000000 ) ) ;
#1526 = CARTESIAN_POINT ( 'NONE',  ( 746.7653713866222915, -329.2601417444138860, 351.0478386215610271 ) ) ;
#1527 = ORIENTED_EDGE ( 'NONE', *, *, #24375, .F. ) ;
#1528 = EDGE_CURVE ( 'NONE', #39743, #11556, #13743, .T. ) ;
#1529 = CARTESIAN_POINT ( 'NONE',  ( 759.9864689768902508, -338.0891481129649492, 354.9819416627836404 ) ) ;
#1530 = ADVANCED_FACE ( 'NONE', ( #14425 ), #42133, .F. ) ;
#1531 = CARTESIAN_POINT ( 'NONE',  ( 810.7187646348534145, -66.45278447660216159, -356.7737145352016341 ) ) ;
#1532 = CARTESIAN_POINT ( 'NONE',  ( 778.1981804954715471, -82.27096629478390355, -314.8072714833591021 ) ) ;
#1533 = EDGE_LOOP ( 'NONE', ( #21943, #37400, #33913, #3178 ) ) ;
#1534 = CARTESIAN_POINT ( 'NONE',  ( 805.2837595273609850, -2.736336299698892027, -340.5290396650784714 ) ) ;
#1535 = ORIENTED_EDGE ( 'NONE', *, *, #32375, .F. ) ;
#1536 = CARTESIAN_POINT ( 'NONE',  ( 772.4468031744293057, -321.8272453906070609, -363.8651313633793620 ) ) ;
#1538 = CARTESIAN_POINT ( 'NONE',  ( 757.4527132478984868, -376.3726999360614514, 329.1273215169538844 ) ) ;
#1537 = CARTESIAN_POINT ( 'NONE',  ( 768.0187753319979720, -56.63460265842036279, 318.0580252608186242 ) ) ;
#1539 = ADVANCED_FACE ( 'NONE', ( #27820 ), #3100, .T. ) ;
#1542 = CARTESIAN_POINT ( 'NONE',  ( 748.3538107759620743, -328.7146871989592682, 355.8262568251490165 ) ) ;
#1541 = CARTESIAN_POINT ( 'NONE',  ( 799.9999999999993179, 205.0000000000000568, 360.0000000000000000 ) ) ;
#1540 = CARTESIAN_POINT ( 'NONE',  ( 767.6429770376291799, -417.1800572038736732, 306.8695393053162093 ) ) ;
#1543 = ADVANCED_FACE ( 'NONE', ( #10261 ), #24338, .F. ) ;
#1544 = CARTESIAN_POINT ( 'NONE',  ( 756.1443688327750579, -93.62377810805098477, 314.3581564841659315 ) ) ;
#1545 = CARTESIAN_POINT ( 'NONE',  ( 755.5913626894240451, -325.6454272087888739, -346.6156483768012890 ) ) ;
#1546 = CARTESIAN_POINT ( 'NONE',  ( 762.1405469898971887, -313.5436935675102745, -357.8594530101015607 ) ) ;
#1547 = CARTESIAN_POINT ( 'NONE',  ( 768.0187753319979720, -152.6346026584200786, -318.0580252608186242 ) ) ;
#1548 = CARTESIAN_POINT ( 'NONE',  ( 811.0346526505616112, -422.6346026584192259, 323.0537975583477532 ) ) ;
#1550 = FACE_BOUND ( 'NONE', #35499, .T. ) ;
#1549 = CARTESIAN_POINT ( 'NONE',  ( 755.2512626584698410, 16.45630643248849267, 315.2512626584710915 ) ) ;
#1551 = CARTESIAN_POINT ( 'NONE',  ( 793.5525998758768083, -103.0999726633349525, -372.6845335610516941 ) ) ;
#1552 = CARTESIAN_POINT ( 'NONE',  ( 355.8971257818259915, 290.0000000000001137, -320.0000000000000568 ) ) ;
#1553 = PLANE ( 'NONE',  #16394 ) ;
#1554 = CARTESIAN_POINT ( 'NONE',  ( 766.9102291470427417, -282.5545181178798657, 318.6633372737382501 ) ) ;
#1555 = CARTESIAN_POINT ( 'NONE',  ( 759.7806653035534055, -174.9982390220563673, 324.8639956371180801 ) ) ;
#1556 = ORIENTED_EDGE ( 'NONE', *, *, #21278, .F. ) ;
#1557 = CARTESIAN_POINT ( 'NONE',  ( 745.0891759886404770, -124.2709662947837899, -342.4968714119734159 ) ) ;
#1558 = ADVANCED_FACE ( 'NONE', ( #21564 ), #18355, .F. ) ;
#1559 = DIRECTION ( 'NONE',  ( 1.000000000000000000, 0.000000000000000000, -0.000000000000000000 ) ) ;
#1560 = CARTESIAN_POINT ( 'NONE',  ( 748.6759233522253680, -88.37269993606226137, 324.3348316497537098 ) ) ;
#1561 = EDGE_CURVE ( 'NONE', #38354, #16465, #40038, .T. ) ;
#1562 = CARTESIAN_POINT ( 'NONE',  ( 814.9108240113580450, -256.2709662947834204, -337.5031285880265273 ) ) ;
#1563 = CARTESIAN_POINT ( 'NONE',  ( 812.7932403749906598, -447.1800572038736732, -327.7687537140311633 ) ) ;
#1564 = CARTESIAN_POINT ( 'NONE',  ( 801.9419747391806368, -114.4527844766020053, 351.9812246680014027 ) ) ;
#1565 = VECTOR ( 'NONE', #44163, 1000.000000000000000 ) ;
#1566 = CARTESIAN_POINT ( 'NONE',  ( 761.9338519418445230, -326.5328690171411381, -370.4231160770881957 ) ) ;
#1567 = CARTESIAN_POINT ( 'NONE',  ( 745.7998596910086917, -77.36187538569302546, -332.5602148656461168 ) ) ;
#1568 = CARTESIAN_POINT ( 'NONE',  ( 804.1105419155481968, -27.82724539060790292, 347.6308680596136469 ) ) ;
#1569 = CARTESIAN_POINT ( 'NONE',  ( 804.7487373415286811, -355.5436935675103882, -364.7487373415288516 ) ) ;
#1570 = FACE_BOUND ( 'NONE', #43424, .T. ) ;
#1571 = CARTESIAN_POINT ( 'NONE',  ( 793.2243759319678702, -386.5328690171409676, 318.4439275373583200 ) ) ;
#1572 = ORIENTED_EDGE ( 'NONE', *, *, #41017, .T. ) ;
#1573 = CARTESIAN_POINT ( 'NONE',  ( 805.1016975059191054, -78.89650538077832209, 343.0745993439771837 ) ) ;
#1574 = CARTESIAN_POINT ( 'NONE',  ( 805.9055244015594326, -123.6237781080508569, -315.8990559732753240 ) ) ;
#1575 = CYLINDRICAL_SURFACE ( 'NONE', #28444, 2.749999999999835687 ) ;
#1576 = CARTESIAN_POINT ( 'NONE',  ( 781.2497674668890113, -252.3510508353232353, 375.3608509340180603 ) ) ;
#1577 = CARTESIAN_POINT ( 'NONE',  ( 754.8072714833583632, -52.81642084023856398, 338.1981804954721156 ) ) ;
#1578 = EDGE_CURVE ( 'NONE', #27745, #12435, #3971, .T. ) ;
#1579 = CARTESIAN_POINT ( 'NONE',  ( 790.8726784830453198, -250.7146871989595809, -362.5472867521010585 ) ) ;
#1580 = CARTESIAN_POINT ( 'NONE',  ( 804.6798772138708955, -231.7255117493288310, 334.6312213355107019 ) ) ;
#1581 = EDGE_CURVE ( 'NONE', #44771, #12718, #29778, .T. ) ;
#1582 = CARTESIAN_POINT ( 'NONE',  ( 752.4576283171824116, -429.0783235625953580, -317.7880784355627952 ) ) ;
#1583 = CARTESIAN_POINT ( 'NONE',  ( 801.9858362298568863, -75.07832356259649487, -312.7379699480935642 ) ) ;
#1584 = DIRECTION ( 'NONE',  ( 0.000000000000000000, -1.000000000000000000, 0.000000000000000000 ) ) ;
#1585 = VERTEX_POINT ( 'NONE', #4019 ) ;
#1586 = EDGE_LOOP ( 'NONE', ( #29834, #5171 ) ) ;
#1587 = CARTESIAN_POINT ( 'NONE',  ( 802.2119215644370342, -366.0090635724250774, -367.5423716828165084 ) ) ;
#1588 = CARTESIAN_POINT ( 'NONE',  ( 774.6858677611749044, -225.7255117493289163, -315.5713283507209894 ) ) ;
#1589 = ADVANCED_FACE ( 'NONE', ( #18120 ), #7960, .F. ) ;
#1590 = CARTESIAN_POINT ( 'NONE',  ( 744.7301800767020268, -316.8164208402377540, 337.4774526936615189 ) ) ;
#1591 = CARTESIAN_POINT ( 'NONE',  ( 807.5423716828161105, -33.07832356259662987, 362.2119215644372048 ) ) ;
#1592 = CARTESIAN_POINT ( 'NONE',  ( 800.9840315886518738, -220.9181544815164102, -354.1144889064786412 ) ) ;
#1593 = CARTESIAN_POINT ( 'NONE',  ( 791.9812246680005501, -188.6346026584199365, -361.9419747391813189 ) ) ;
#1594 = AXIS2_PLACEMENT_3D ( 'NONE', #10655, #18050, #497 ) ;
#1595 = CARTESIAN_POINT ( 'NONE',  ( 804.4286716492782716, -377.3618753856920875, -345.3141322388244703 ) ) ;
#1596 = ORIENTED_EDGE ( 'NONE', *, *, #2120, .T. ) ;
#1597 = CARTESIAN_POINT ( 'NONE',  ( 757.8323909638827445, -218.6346026584197944, 352.1044303154654358 ) ) ;
#1598 = CARTESIAN_POINT ( 'NONE',  ( 788.8264449731200330, -117.1800572038746964, -363.6646147819171233 ) ) ;
#1599 = EDGE_LOOP ( 'NONE', ( #39442, #9325, #33134, #32362 ) ) ;
#1600 = CARTESIAN_POINT ( 'NONE',  ( 759.0252816721024374, -336.9982390220558273, 368.0189434323527280 ) ) ;
#1601 = DIRECTION ( 'NONE',  ( 0.000000000000000000, 0.7651688349527167032, -0.6438296778008156807 ) ) ;
#1602 = CARTESIAN_POINT ( 'NONE',  ( 805.0264073115434940, -366.3510508353228374, 339.4763451958999099 ) ) ;
#1603 = PLANE ( 'NONE',  #28511 ) ;
#1604 = LINE ( 'NONE', #25652, #280 ) ;
#1605 = CARTESIAN_POINT ( 'NONE',  ( 769.0155153010367712, -202.3726999360618777, 362.7791456095907279 ) ) ;
#1606 = CARTESIAN_POINT ( 'NONE',  ( 785.3141322388236176, -69.72551174932942786, 364.4286716492789537 ) ) ;
#1607 = ORIENTED_EDGE ( 'NONE', *, *, #1291, .F. ) ;
#1608 = CARTESIAN_POINT ( 'NONE',  ( 802.2119215644370342, -462.0090635724247932, -367.5423716828165084 ) ) ;
#1609 = CARTESIAN_POINT ( 'NONE',  ( 751.9810565676468741, -26.08914811296592262, -360.9747183278973921 ) ) ;
#1610 = CARTESIAN_POINT ( 'NONE',  ( 779.4709603349208464, -216.3510508353233490, 314.7162404726379918 ) ) ;
#1611 = CARTESIAN_POINT ( 'NONE',  ( 758.0580252608178853, -414.4527844766010389, -328.0187753319985404 ) ) ;
#1612 = CARTESIAN_POINT ( 'NONE',  ( 785.3141322388236176, -21.72551174932956641, -364.4286716492789537 ) ) ;
#1613 = CARTESIAN_POINT ( 'NONE',  ( 745.4481719005789273, -435.7255117493282341, 347.5162901302853129 ) ) ;
#1614 = DIRECTION ( 'NONE',  ( 0.000000000000000000, 0.000000000000000000, 1.000000000000000000 ) ) ;
#1615 = CARTESIAN_POINT ( 'NONE',  ( 804.1105419155481968, -267.8272453906071746, -347.6308680596136469 ) ) ;
#1616 = CARTESIAN_POINT ( 'NONE',  ( 792.2312462859673587, -155.9073299311473306, -307.2067596250082602 ) ) ;
#1617 = CARTESIAN_POINT ( 'NONE',  ( 792.2312462859673587, -35.90732993114770011, 307.2067596250082602 ) ) ;
#1618 = CARTESIAN_POINT ( 'NONE',  ( 814.2001403089898304, -137.3618753856928265, 347.4397851343538264 ) ) ;
#1619 = CARTESIAN_POINT ( 'NONE',  ( 768.1267186599862953, 16.45630643248851044, -317.8138973628999224 ) ) ;
#1620 = FILL_AREA_STYLE_COLOUR ( '', #18819 ) ;
#1621 = DIRECTION ( 'NONE',  ( 0.9164815115825496461, 0.1263042864341401839, 0.3796167358741286413 ) ) ;
#1622 = CARTESIAN_POINT ( 'NONE',  ( 792.2312462859673587, -371.9073299311465917, 307.2067596250082602 ) ) ;
#1623 = CARTESIAN_POINT ( 'NONE',  ( 764.8639956371174549, -320.0891481129648355, -319.7806653035542013 ) ) ;
#1624 = CARTESIAN_POINT ( 'NONE',  ( 764.0069404352550464, 8.921676437403235127, 359.2566176426627180 ) ) ;
#1625 = CARTESIAN_POINT ( 'NONE',  ( 748.6759233522253680, -112.3726999360621761, -324.3348316497537098 ) ) ;
#1626 = CARTESIAN_POINT ( 'NONE',  ( 799.4546378042377910, -129.0783235625963243, -356.1575198192848006 ) ) ;
#1627 = CARTESIAN_POINT ( 'NONE',  ( 805.9055244015594326, -147.6237781080508285, 315.8990559732753240 ) ) ;
#1628 = CARTESIAN_POINT ( 'NONE',  ( 764.8639956371174549, -440.0891481129645513, 319.7806653035542581 ) ) ;
#1629 = CARTESIAN_POINT ( 'NONE',  ( 803.4237431249931660, -39.18005720387496638, -331.2633955100225194 ) ) ;
#1630 = CARTESIAN_POINT ( 'NONE',  ( 793.2243759319678702, -146.5328690171417350, -318.4439275373583200 ) ) ;
#1631 = CARTESIAN_POINT ( 'NONE',  ( 774.6858677611749044, -129.7255117493292289, -315.5713283507209894 ) ) ;
#1632 = CARTESIAN_POINT ( 'NONE',  ( 797.8594530101008786, -133.5436935675110135, 322.1405469898980982 ) ) ;
#1633 = CARTESIAN_POINT ( 'NONE',  ( 790.8726784830453198, -442.7146871989589840, -362.5472867521010585 ) ) ;
#1635 = CARTESIAN_POINT ( 'NONE',  ( 755.3201227861273992, -243.7255117493288310, 345.3687786644892981 ) ) ;
#1634 = CARTESIAN_POINT ( 'NONE',  ( 774.6858677611749044, -273.7255117493288026, 315.5713283507209894 ) ) ;
#1636 = CARTESIAN_POINT ( 'NONE',  ( 1238.921997096861332, 430.0000000000002842, -244.9999999999999716 ) ) ;
#1637 = VERTEX_POINT ( 'NONE', #36337 ) ;
#1638 = CARTESIAN_POINT ( 'NONE',  ( 797.8594530101008786, -445.5436935675098766, 322.1405469898980982 ) ) ;
#1639 = CARTESIAN_POINT ( 'NONE',  ( 746.4236121716829757, -279.8272453906071746, -328.8385539511384650 ) ) ;
#1640 = ORIENTED_EDGE ( 'NONE', *, *, #30606, .T. ) ;
#1641 = CARTESIAN_POINT ( 'NONE',  ( 0.000000000000000000, 0.000000000000000000, 0.000000000000000000 ) ) ;
#1642 = CARTESIAN_POINT ( 'NONE',  ( 808.0189434323515343, -206.0891481129653471, 319.0252816721025511 ) ) ;
#1643 = CARTESIAN_POINT ( 'NONE',  ( 802.5472867521000353, -292.3726999360616219, 350.8726784830461156 ) ) ;
#1644 = CARTESIAN_POINT ( 'NONE',  ( 801.3366627262608972, -392.5328690171409107, 353.0897708529566899 ) ) ;
#1645 = ORIENTED_EDGE ( 'NONE', *, *, #20048, .T. ) ;
#1646 = CARTESIAN_POINT ( 'NONE',  ( 758.4439275373578084, -132.5545181178802920, -353.2243759319684386 ) ) ;
#1647 = VECTOR ( 'NONE', #23247, 1000.000000000000000 ) ;
#1648 = VERTEX_POINT ( 'NONE', #28962 ) ;
#1649 = CARTESIAN_POINT ( 'NONE',  ( 803.6646147819161570, -401.9073299311463643, -348.8264449731210561 ) ) ;
#1650 = CARTESIAN_POINT ( 'NONE',  ( 800.2193346964447755, -90.99823902205663728, -355.1360043628815788 ) ) ;
#1651 = CARTESIAN_POINT ( 'NONE',  ( 766.7756240680305382, -278.5328690171412518, 361.5560724626415663 ) ) ;
#1652 = CARTESIAN_POINT ( 'NONE',  ( 772.4999999999993179, -462.9681489794448339, 369.0473750965555837 ) ) ;
#1653 = CARTESIAN_POINT ( 'NONE',  ( -858.8365100919713768, 240.0000000000002274, -197.2499999999882903 ) ) ;
#1654 = CARTESIAN_POINT ( 'NONE',  ( 814.2805881961230625, -1.645427208789804308, -331.2368401574024119 ) ) ;
#1655 = LINE ( 'NONE', #33102, #38693 ) ;
#1656 = VERTEX_POINT ( 'NONE', #25720 ) ;
#1657 = CARTESIAN_POINT ( 'NONE',  ( 745.7194118038753459, -325.6454272087888739, -348.7631598425976449 ) ) ;
#1658 = CIRCLE ( 'NONE', #5350, 2.749999999999919176 ) ;
#1660 = CARTESIAN_POINT ( 'NONE',  ( 803.4237431249931660, -279.1800572038741848, -331.2633955100225194 ) ) ;
#1659 = CARTESIAN_POINT ( 'NONE',  ( 779.9999999999992042, -462.9681489794448339, -339.9999999999999432 ) ) ;
#1661 = DIRECTION ( 'NONE',  ( 0.000000000000000000, 0.000000000000000000, 1.000000000000000000 ) ) ;
#1662 = CARTESIAN_POINT ( 'NONE',  ( 769.0155153010367712, -154.3726999360620198, -362.7791456095907279 ) ) ;
#1663 = CARTESIAN_POINT ( 'NONE',  ( 754.9967657858570647, -25.54369356751136877, 365.0032342141425374 ) ) ;
#1664 = CARTESIAN_POINT ( 'NONE',  ( 989.9999999999992042, 62.85347435602256638, -357.4246812887967053 ) ) ;
#1665 = CARTESIAN_POINT ( 'NONE',  ( 763.2262854647970016, -344.6346026584195101, -309.2812353651462445 ) ) ;
#1666 = CARTESIAN_POINT ( 'NONE',  ( 805.1927285166397041, -40.81642084023859951, 341.8018195045277707 ) ) ;
#1667 = CARTESIAN_POINT ( 'NONE',  ( 807.2620300519052989, -288.0090635724252479, 318.0141637701419768 ) ) ;
#1668 = CARTESIAN_POINT ( 'NONE',  ( 772.5602148656447525, -249.7255117493288594, 305.7998596910095443 ) ) ;
#1669 = CARTESIAN_POINT ( 'NONE',  ( 783.7566961878529810, -432.8965053807771142, -305.1792804349288417 ) ) ;
#1670 = CARTESIAN_POINT ( 'NONE',  ( 989.9999999999992042, 50.81038600091411439, 217.3872392842761769 ) ) ;
#1671 = DIRECTION ( 'NONE',  ( 1.892425610156518354E-16, 1.000000000000000000, -0.000000000000000000 ) ) ;
#1672 = CARTESIAN_POINT ( 'NONE',  ( 758.0580252608178853, -342.4527844766013231, 328.0187753319985404 ) ) ;
#1673 = AXIS2_PLACEMENT_3D ( 'NONE', #6623, #14021, #14713 ) ;
#1674 = CARTESIAN_POINT ( 'NONE',  ( 773.4516893846965786, -115.6454272087894424, 315.8398074228977066 ) ) ;
#1675 = CARTESIAN_POINT ( 'NONE',  ( 800.7704444035546203, -28.16923265350574468, -326.0291762391768771 ) ) ;
#1676 = PRODUCT_DEFINITION_FORMATION_WITH_SPECIFIED_SOURCE ( 'ANY', '', #9267, .NOT_KNOWN. ) ;
#1677 = DIRECTION ( 'NONE',  ( -0.000000000000000000, -0.000000000000000000, 1.000000000000000000 ) ) ;
#1678 = CARTESIAN_POINT ( 'NONE',  ( 187.1337867209877857, -422.8782571739196783, -207.4246812887968190 ) ) ;
#1679 = CARTESIAN_POINT ( 'NONE',  ( 800.2193346964447755, -378.9982390220555999, 355.1360043628815788 ) ) ;
#1680 = ORIENTED_EDGE ( 'NONE', *, *, #36506, .F. ) ;
#1681 = CARTESIAN_POINT ( 'NONE',  ( 756.7813123517142913, -331.9874144716865203, -329.9779781133712504 ) ) ;
#1682 = CARTESIAN_POINT ( 'NONE',  ( 754.8072714833581358, -148.8164208402382656, 338.1981804954720587 ) ) ;
#1683 = ADVANCED_FACE ( 'NONE', ( #32198 ), #25251, .F. ) ;
#1684 = CARTESIAN_POINT ( 'NONE',  ( 793.4146539503750546, -313.9874144716866908, -307.6481478633938877 ) ) ;
#1685 = VERTEX_POINT ( 'NONE', #28739 ) ;
#1686 = CARTESIAN_POINT ( 'NONE',  ( 762.3223304703356007, -367.5436935675102745, 322.3223304703362828 ) ) ;
#1687 = ORIENTED_EDGE ( 'NONE', *, *, #6335, .T. ) ;
#1688 = DIRECTION ( 'NONE',  ( 1.000000000000000000, 0.000000000000000000, 0.000000000000000000 ) ) ;
#1689 = CARTESIAN_POINT ( 'NONE',  ( 777.5031285880264704, -166.8164208402382087, -374.9108240113588408 ) ) ;
#1690 = CARTESIAN_POINT ( 'NONE',  ( 796.9462024416508257, -84.45278447660207632, 308.9653473494370246 ) ) ;
#1691 = VERTEX_POINT ( 'NONE', #560 ) ;
#1692 = CARTESIAN_POINT ( 'NONE',  ( 804.4286716492782716, -161.3618753856927697, -345.3141322388244703 ) ) ;
#1693 = ORIENTED_EDGE ( 'NONE', *, *, #19596, .T. ) ;
#1694 = CARTESIAN_POINT ( 'NONE',  ( 760.7433823573367135, -420.0090635724249069, -355.9930595647440441 ) ) ;
#1695 = CARTESIAN_POINT ( 'NONE',  ( 744.7301800767019131, -268.8164208402378108, 337.4774526936615757 ) ) ;
#1696 = CARTESIAN_POINT ( 'NONE',  ( 805.1016975059191054, -150.8965053807781089, 343.0745993439771837 ) ) ;
#1699 = CARTESIAN_POINT ( 'NONE',  ( 788.7631598425961101, -409.4419599262317320, 305.7194118038759143 ) ) ;
#1698 = CYLINDRICAL_SURFACE ( 'NONE', #43242, 24.99999999999991118 ) ;
#1697 = CARTESIAN_POINT ( 'NONE',  ( 999.5857864376259840, 249.9999999999998863, -360.0000000000000000 ) ) ;
#1700 = ORIENTED_EDGE ( 'NONE', *, *, #30911, .T. ) ;
#1701 = CARTESIAN_POINT ( 'NONE',  ( 790.0220218866281812, -439.0999726633339719, -363.2186876482849129 ) ) ;
#1702 = DIRECTION ( 'NONE',  ( 1.000000000000000000, 0.000000000000000000, 0.000000000000000000 ) ) ;
#1703 = AXIS2_PLACEMENT_3D ( 'NONE', #5254, #19345, #33429 ) ;
#1704 = CARTESIAN_POINT ( 'NONE',  ( 802.2119215644370342, -198.0090635724255606, -367.5423716828165084 ) ) ;
#1705 = CIRCLE ( 'NONE', #44413, 12.00000000000001066 ) ;
#1706 = CARTESIAN_POINT ( 'NONE',  ( 813.5763878283155464, -51.82724539060782121, 351.1614460488615350 ) ) ;
#1708 = CARTESIAN_POINT ( 'NONE',  ( 792.1044303154645831, -180.4527844766017211, -317.8323909638837677 ) ) ;
#1707 = DIRECTION ( 'NONE',  ( 0.000000000000000000, 0.000000000000000000, 1.000000000000000000 ) ) ;
#1709 = CARTESIAN_POINT ( 'NONE',  ( 754.9735926884551418, -378.3510508353227806, -340.5236548041000333 ) ) ;
#1710 = CYLINDRICAL_SURFACE ( 'NONE', #21162, 9.999999999999982236 ) ;
#1711 = CARTESIAN_POINT ( 'NONE',  ( 745.1792804349281596, -230.1908817542436338, -343.7566961878542884 ) ) ;
#1712 = CARTESIAN_POINT ( 'NONE',  ( 799.9999999999993179, -462.9681489794448339, -362.3606797749978909 ) ) ;
#1713 = DIRECTION ( 'NONE',  ( 0.000000000000000000, 0.000000000000000000, 1.000000000000000000 ) ) ;
#1714 = CARTESIAN_POINT ( 'NONE',  ( 772.4468031744293057, -57.82724539060780700, -363.8651313633793620 ) ) ;
#1715 = CARTESIAN_POINT ( 'NONE',  ( 786.5483106153019435, -391.6454272087885897, 364.1601925771022366 ) ) ;
#1716 = CARTESIAN_POINT ( 'NONE',  ( 796.9462024416508257, -252.4527844766015789, -308.9653473494370246 ) ) ;
#1717 = CARTESIAN_POINT ( 'NONE',  ( 805.2837595273609850, -242.7363362996980811, 340.5290396650784714 ) ) ;
#1718 = CARTESIAN_POINT ( 'NONE',  ( 773.4999999999993179, -110.5936016518799221, 750.6326042729449455 ) ) ;
#1719 = CARTESIAN_POINT ( 'NONE',  ( 759.9999999999992042, 166.4563064324884465, 319.9999999999999432 ) ) ;
#1720 = CARTESIAN_POINT ( 'NONE',  ( 785.3687786644884454, -35.36187538569316047, -315.3201227861279676 ) ) ;
#1721 = CARTESIAN_POINT ( 'NONE',  ( 804.1009440267234822, -191.4636090269709996, 314.0944755984392600 ) ) ;
#1722 = CARTESIAN_POINT ( 'NONE',  ( 754.0944755984390895, -135.6237781080508853, -364.1009440267246760 ) ) ;
#1723 = CARTESIAN_POINT ( 'NONE',  ( 751.6929314249748586, -150.9982390220563957, 318.8095938919659034 ) ) ;
#1724 = CARTESIAN_POINT ( 'NONE',  ( 777.4774526936600978, -370.2709662947831362, -304.7301800767027657 ) ) ;
#1725 = CARTESIAN_POINT ( 'NONE',  ( 789.9999999999992042, 205.0000000000000568, -339.9999999999999432 ) ) ;
#1726 = CARTESIAN_POINT ( 'NONE',  ( 756.3353852180819104, -245.9073299311469896, 331.1735550268788302 ) ) ;
#1727 = CARTESIAN_POINT ( 'NONE',  ( 790.0220218866281812, -31.09997266333516919, 363.2186876482849129 ) ) ;
#1728 = CARTESIAN_POINT ( 'NONE',  ( 805.1927285166397041, -376.8164208402375834, -341.8018195045277707 ) ) ;
#1729 =( BOUNDED_CURVE ( )  B_SPLINE_CURVE ( 3, ( #32757, #8061, #36212, #40382 ),
 .UNSPECIFIED., .F., .T. ) 
 B_SPLINE_CURVE_WITH_KNOTS ( ( 4, 4 ),
 ( 4.712388980384689674, 6.283185307179586232 ),
 .UNSPECIFIED. ) 
 CURVE ( )  GEOMETRIC_REPRESENTATION_ITEM ( )  RATIONAL_B_SPLINE_CURVE ( ( 1.000000000000000000, 0.8047378541243649375, 0.8047378541243649375, 1.000000000000000000 ) ) 
 REPRESENTATION_ITEM ( '' )  );
#1730 = CARTESIAN_POINT ( 'NONE',  ( 181.1634899080285948, 258.0939999999999941, -199.9999999999953957 ) ) ;
#1731 = CARTESIAN_POINT ( 'NONE',  ( 772.5602148656447525, -441.7255117493282910, -305.7998596910095443 ) ) ;
#1732 = CARTESIAN_POINT ( 'NONE',  ( 772.4999999999993179, -512.9681489794448908, -339.9999999999999432 ) ) ;
#1733 = CARTESIAN_POINT ( 'NONE',  ( 803.8651313633788504, -77.26014174441466764, 332.4468031744301015 ) ) ;
#1734 = ORIENTED_EDGE ( 'NONE', *, *, #8319, .T. ) ;
#1735 = EDGE_CURVE ( 'NONE', #2122, #26522, #22240, .T. ) ;
#1736 = CARTESIAN_POINT ( 'NONE',  ( 758.6633372737375112, -212.5328690171415076, -326.9102291470432533 ) ) ;
#1737 = AXIS2_PLACEMENT_3D ( 'NONE', #29256, #18625, #39664 ) ;
#1738 = CARTESIAN_POINT ( 'NONE',  ( 767.8955696845333705, -48.45278447660219712, 362.1676090361162323 ) ) ;
#1739 = COLOUR_RGB ( '',0.7921568627450980005, 0.8196078431372548767, 0.9333333333333333481 ) ;
#1740 = CARTESIAN_POINT ( 'NONE',  ( 754.0944755984390895, -231.6237781080504874, -364.1009440267246760 ) ) ;
#1741 = CARTESIAN_POINT ( 'NONE',  ( 779.9999999999992042, 126.4563064324884465, -329.9999999999999432 ) ) ;
#1742 = CARTESIAN_POINT ( 'NONE',  ( 793.4146539503750546, -361.9874144716864635, 307.6481478633938877 ) ) ;
#1743 = ORIENTED_EDGE ( 'NONE', *, *, #15407, .F. ) ;
#1744 = CARTESIAN_POINT ( 'NONE',  ( 757.8323909638827445, -146.6346026584200217, -352.1044303154654358 ) ) ;
#1745 = CARTESIAN_POINT ( 'NONE',  ( 794.9819416627830151, -348.9982390220558273, 319.9864689768909898 ) ) ;
#1746 = CARTESIAN_POINT ( 'NONE',  ( 745.0891759886404770, -76.27096629478394618, -342.4968714119734159 ) ) ;
#1747 = CARTESIAN_POINT ( 'NONE',  ( 764.8639956371174549, -56.08914811296581604, -319.7806653035542581 ) ) ;
#1748 = ORIENTED_EDGE ( 'NONE', *, *, #16779, .F. ) ;
#1749 = CARTESIAN_POINT ( 'NONE',  ( 801.5560724626406000, -0.5545181178807169209, -326.7756240680316182 ) ) ;
#1750 = CARTESIAN_POINT ( 'NONE',  ( 769.9779781133707957, -307.0999726633343130, -316.7813123517150871 ) ) ;
#1751 = AXIS2_PLACEMENT_3D ( 'NONE', #40538, #8887, #9347 ) ;
#1753 = CARTESIAN_POINT ( 'NONE',  ( 760.7433823573367135, -372.0090635724250205, 355.9930595647440441 ) ) ;
#1752 = CARTESIAN_POINT ( 'NONE',  ( 794.9819416627830151, -108.9982390220565804, 319.9864689768909898 ) ) ;
#1756 = CARTESIAN_POINT ( 'NONE',  ( 781.2497674668890113, -324.3510508353229511, 375.3608509340180603 ) ) ;
#1755 = DIRECTION ( 'NONE',  ( 0.000000000000000000, 0.7372773368101328550, -0.6755902076156506952 ) ) ;
#1754 = CARTESIAN_POINT ( 'NONE',  ( 745.0891759886404770, -436.2709662947827951, 342.4968714119734159 ) ) ;
#1757 = CARTESIAN_POINT ( 'NONE',  ( 764.3348316497523456, -94.71468719896007826, 308.6759233522265617 ) ) ;
#1758 = CARTESIAN_POINT ( 'NONE',  ( 801.5560724626406000, -336.5545181178796952, -326.7756240680316182 ) ) ;
#1759 = CARTESIAN_POINT ( 'NONE',  ( 767.8955696845333705, -336.4527844766012095, -362.1676090361162323 ) ) ;
#1760 = CARTESIAN_POINT ( 'NONE',  ( 759.9864689768902508, -146.0891481129655176, -354.9819416627836404 ) ) ;
#1761 = CARTESIAN_POINT ( 'NONE',  ( 748.9653473494363425, -434.6346026584190554, 356.9462024416521331 ) ) ;
#1763 = DIRECTION ( 'NONE',  ( -1.000000000000000000, -0.000000000000000000, -0.000000000000000000 ) ) ;
#1762 = CARTESIAN_POINT ( 'NONE',  ( 782.7696130847263021, 18.14353250567099707, 310.1281195208451322 ) ) ;
#1764 = CARTESIAN_POINT ( 'NONE',  ( 768.9521613784389729, -129.8272453906075725, -373.2346286133773106 ) ) ;
#1765 = CARTESIAN_POINT ( 'NONE',  ( 779.9999999999992042, -462.9681489794448339, 370.0000000000000568 ) ) ;
#1766 = CYLINDRICAL_SURFACE ( 'NONE', #37801, 2.749999999999835687 ) ;
#1767 = CARTESIAN_POINT ( 'NONE',  ( 761.4292242960306112, -281.4636090269706870, 323.2154366446414429 ) ) ;
#1768 = CARTESIAN_POINT ( 'NONE',  ( 781.7834795799800531, -178.8164208402381519, 315.0636971347436202 ) ) ;
#1769 = VERTEX_POINT ( 'NONE', #11404 ) ;
#1770 = CARTESIAN_POINT ( 'NONE',  ( 773.7305795820266212, -273.2817908451526137, 374.8230680027170365 ) ) ;
#1771 = AXIS2_PLACEMENT_3D ( 'NONE', #16689, #8846, #40278 ) ;
#1772 = CARTESIAN_POINT ( 'NONE',  ( 759.0252816721024374, -144.9982390220564525, -368.0189434323527280 ) ) ;
#1773 = LINE ( 'NONE', #45441, #7634 ) ;
#1774 = CARTESIAN_POINT ( 'NONE',  ( 757.7880784355613741, -66.00906357242595845, 312.4576283171834916 ) ) ;
#1775 = CARTESIAN_POINT ( 'NONE',  ( 796.7737145352015204, -260.6346026584197375, -370.7187646348536987 ) ) ;
#1776 = EDGE_CURVE ( 'NONE', #14297, #8747, #14884, .T. ) ;
#1777 = CARTESIAN_POINT ( 'NONE',  ( 793.3938497862117174, -453.0432664090020580, -372.3358127763067955 ) ) ;
#1778 = CARTESIAN_POINT ( 'NONE',  ( 755.0636971347428243, -148.2709662947837330, 341.7834795799807353 ) ) ;
#1779 = ORIENTED_EDGE ( 'NONE', *, *, #1261, .T. ) ;
#1780 = CARTESIAN_POINT ( 'NONE',  ( 776.2433038121456548, -348.8965053807774552, -374.8207195650711014 ) ) ;
#1781 = CARTESIAN_POINT ( 'NONE',  ( 787.5162901302840055, -83.36187538569296862, -305.4481719005792684 ) ) ;
#1782 = AXIS2_PLACEMENT_3D ( 'NONE', #9208, #19373, #33692 ) ;
#1783 = CARTESIAN_POINT ( 'NONE',  ( 799.2566176426618085, -0.009063572426172561425, 324.0069404352559559 ) ) ;
#1784 = CARTESIAN_POINT ( 'NONE',  ( 811.0346526505616112, -350.6346026584192828, -323.0537975583477532 ) ) ;
#1785 = DIRECTION ( 'NONE',  ( 1.000000000000000000, 0.000000000000000000, -0.000000000000000000 ) ) ;
#1786 = CARTESIAN_POINT ( 'NONE',  ( 790.8726784830453198, -394.7146871989591546, 362.5472867521010585 ) ) ;
#1787 = ORIENTED_EDGE ( 'NONE', *, *, #3181, .F. ) ;
#1788 = EDGE_CURVE ( 'NONE', #28471, #16704, #1035, .T. ) ;
#1789 = EDGE_CURVE ( 'NONE', #18281, #21321, #6935, .T. ) ;
#1790 = VECTOR ( 'NONE', #5422, 1000.000000000000000 ) ;
#1791 = CARTESIAN_POINT ( 'NONE',  ( 791.1614460488616487, -131.2601417444144829, -373.5763878283158874 ) ) ;
#1792 = CARTESIAN_POINT ( 'NONE',  ( 181.1634899080285948, 258.0939999999999941, -193.8809999999953959 ) ) ;
#1793 = CARTESIAN_POINT ( 'NONE',  ( 800.1688906516307043, -250.1692326535050199, 369.0717654672308186 ) ) ;
#1794 = CARTESIAN_POINT ( 'NONE',  ( 794.9819416627830151, -84.99823902205663728, 319.9864689768909898 ) ) ;
#1795 = ORIENTED_EDGE ( 'NONE', *, *, #40528, .F. ) ;
#1796 = CARTESIAN_POINT ( 'NONE',  ( 779.4709603349208464, -0.3510508353240099355, -314.7162404726379918 ) ) ;
#1797 = CARTESIAN_POINT ( 'NONE',  ( 774.6312213355099630, -239.3618753856924570, 364.6798772138717482 ) ) ;
#1798 = VECTOR ( 'NONE', #38745, 1000.000000000000000 ) ;
#1799 = CARTESIAN_POINT ( 'NONE',  ( 781.2497674668890113, -420.3510508353225532, -375.3608509340180603 ) ) ;
#1800 = DIRECTION ( 'NONE',  ( 0.000000000000000000, 0.3826834323650836756, 0.9238795325112892920 ) ) ;
#1801 = AXIS2_PLACEMENT_3D ( 'NONE', #17086, #35085, #42250 ) ;
#1802 = EDGE_CURVE ( 'NONE', #5430, #41897, #11642, .T. ) ;
#1803 = ORIENTED_EDGE ( 'NONE', *, *, #30300, .T. ) ;
#1804 = EDGE_LOOP ( 'NONE', ( #9462, #35099, #17743, #26253, #8483, #37145 ) ) ;
#1805 = CARTESIAN_POINT ( 'NONE',  ( 802.2119215644370342, -390.0090635724249069, -367.5423716828165084 ) ) ;
#1806 = AXIS2_PLACEMENT_3D ( 'NONE', #7030, #17662, #3576 ) ;
#1807 = EDGE_CURVE ( 'NONE', #23028, #44488, #4925, .T. ) ;
#1808 = CARTESIAN_POINT ( 'NONE',  ( 804.4286716492782716, -233.3618753856925423, -345.3141322388244703 ) ) ;
#1809 = CARTESIAN_POINT ( 'NONE',  ( 767.6429770376291799, -321.1800572038740711, 306.8695393053162093 ) ) ;
#1810 = CARTESIAN_POINT ( 'NONE',  ( 751.2241431872005251, -16.16923265350578021, 359.9636004259367610 ) ) ;
#1811 = CARTESIAN_POINT ( 'NONE',  ( 760.7433823573367135, -228.0090635724254753, -355.9930595647440441 ) ) ;
#1812 = CARTESIAN_POINT ( 'NONE',  ( 767.8955696845333705, -216.4527844766016926, -362.1676090361162323 ) ) ;
#1813 = VERTEX_POINT ( 'NONE', #33115 ) ;
#1814 = CARTESIAN_POINT ( 'NONE',  ( 788.8264449731200330, -213.1800572038743553, 363.6646147819171233 ) ) ;
#1815 = CARTESIAN_POINT ( 'NONE',  ( 767.8955696845333705, -96.45278447660203369, -362.1676090361162323 ) ) ;
#1816 = ORIENTED_EDGE ( 'NONE', *, *, #41907, .F. ) ;
#1817 = CARTESIAN_POINT ( 'NONE',  ( 744.7301800767019131, -316.8164208402377540, 337.4774526936615757 ) ) ;
#1818 = AXIS2_PLACEMENT_3D ( 'NONE', #5730, #9193, #2253 ) ;
#1819 = DIRECTION ( 'NONE',  ( -2.750100768424433062E-32, 1.672022627447525240E-16, -1.000000000000000000 ) ) ;
#1820 = LINE ( 'NONE', #42339, #29283 ) ;
#1821 = DIRECTION ( 'NONE',  ( 8.659560562354884787E-17, 0.7071067811865513475, -0.7071067811865435759 ) ) ;
#1822 = AXIS2_PLACEMENT_3D ( 'NONE', #15835, #9132, #36861 ) ;
#1823 = CARTESIAN_POINT ( 'NONE',  ( 776.9254006560222479, -188.1908817542437760, 314.8983024940802125 ) ) ;
#1824 = CARTESIAN_POINT ( 'NONE',  ( 797.6776695296629214, -91.54369356751116982, 357.6776695296636603 ) ) ;
#1825 = ORIENTED_EDGE ( 'NONE', *, *, #4000, .F. ) ;
#1826 = CARTESIAN_POINT ( 'NONE',  ( 807.2620300519052989, -456.0090635724247932, -318.0141637701419768 ) ) ;
#1827 = CARTESIAN_POINT ( 'NONE',  ( 792.3570229623691148, -45.18005720387493795, -373.1304606946836770 ) ) ;
#1828 = CARTESIAN_POINT ( 'NONE',  ( 805.1016975059191054, -246.8965053807777679, 343.0745993439771837 ) ) ;
#1829 = CARTESIAN_POINT ( 'NONE',  ( 778.1981804954714335, -394.2709662947827951, -314.8072714833589885 ) ) ;
#1830 = CARTESIAN_POINT ( 'NONE',  ( 788.7366044899766848, -11.90732993114778182, -316.5762568750059813 ) ) ;
#1831 = ADVANCED_FACE ( 'NONE', ( #32886 ), #35889, .F. ) ;
#1832 = CARTESIAN_POINT ( 'NONE',  ( 767.6429770376289525, -441.1800572038735027, 306.8695393053162093 ) ) ;
#1833 = CARTESIAN_POINT ( 'NONE',  ( -786.4999999999993179, -365.3551492539851893, -8.132432514707076621 ) ) ;
#1834 = CARTESIAN_POINT ( 'NONE',  ( 755.5913626894240451, -277.6454272087889308, -346.6156483768012890 ) ) ;
#1835 = CARTESIAN_POINT ( 'NONE',  ( 767.6429770376289525, -177.1800572038744690, -306.8695393053162093 ) ) ;
#1836 = EDGE_CURVE ( 'NONE', #1585, #820, #32766, .T. ) ;
#1837 = AXIS2_PLACEMENT_3D ( 'NONE', #10668, #24752, #17142 ) ;
#1838 = CARTESIAN_POINT ( 'NONE',  ( 777.4774526936600978, -34.27096629478407408, 304.7301800767027657 ) ) ;
#1839 = CARTESIAN_POINT ( 'NONE',  ( 745.4481719005789273, -147.7255117493291152, 347.5162901302853129 ) ) ;
#1840 = DIRECTION ( 'NONE',  ( 0.000000000000000000, -1.000000000000000000, 0.000000000000000000 ) ) ;
#1841 = AXIS2_PLACEMENT_3D ( 'NONE', #25140, #18248, #891 ) ;
#1842 = FACE_OUTER_BOUND ( 'NONE', #3408, .T. ) ;
#1843 = AXIS2_PLACEMENT_3D ( 'NONE', #23538, #17085, #9694 ) ;
#1844 = CARTESIAN_POINT ( 'NONE',  ( 879.9999999999992042, 99.99999999999984368, -350.0000000000000000 ) ) ;
#1845 = CARTESIAN_POINT ( 'NONE',  ( 792.2312462859673587, -347.9073299311467053, 307.2067596250082602 ) ) ;
#1846 = EDGE_CURVE ( 'NONE', #22430, #39622, #19023, .T. ) ;
#1847 = CARTESIAN_POINT ( 'NONE',  ( 804.6798772138708955, -351.7255117493284047, -334.6312213355107019 ) ) ;
#1848 = EDGE_CURVE ( 'NONE', #24881, #7749, #17997, .T. ) ;
#1849 = CARTESIAN_POINT ( 'NONE',  ( 760.5453621957607311, 2.921676437403253779, 323.8424801807151425 ) ) ;
#1850 = CARTESIAN_POINT ( 'NONE',  ( 749.5768839229115201, -84.55451811788046257, -358.0661480581553064 ) ) ;
#1851 = CARTESIAN_POINT ( 'NONE',  ( 760.5453621957607311, -117.0783235625963528, -323.8424801807151425 ) ) ;
#1852 = CARTESIAN_POINT ( 'NONE',  ( 783.7566961878529810, -120.8965053807781800, 305.1792804349288417 ) ) ;
#1853 = CARTESIAN_POINT ( 'NONE',  ( 756.3353852180820240, -437.9073299311464211, 331.1735550268787733 ) ) ;
#1854 = AXIS2_PLACEMENT_3D ( 'NONE', #40565, #2202, #36645 ) ;
#1855 = CARTESIAN_POINT ( 'NONE',  ( 774.6858677611749044, -33.72551174932952733, -315.5713283507209894 ) ) ;
#1856 = CARTESIAN_POINT ( 'NONE',  ( 802.7791456095903868, -124.7146871989599930, -329.0155153010375102 ) ) ;
#1857 = CARTESIAN_POINT ( 'NONE',  ( 781.7834795799800531, -130.8164208402383224, -315.0636971347436202 ) ) ;
#1858 = CARTESIAN_POINT ( 'NONE',  ( 774.6312213355099630, -143.3618753856927697, 364.6798772138717482 ) ) ;
#1859 = VECTOR ( 'NONE', #34701, 1000.000000000000000 ) ;
#1860 = CARTESIAN_POINT ( 'NONE',  ( 760.5453621957607311, -429.0783235625953580, -323.8424801807151425 ) ) ;
#1862 = CARTESIAN_POINT ( 'NONE',  ( 803.6646147819162707, -257.9073299311469327, 348.8264449731211130 ) ) ;
#1861 = CARTESIAN_POINT ( 'NONE',  ( 771.1735550268778070, -297.1800572038740711, 316.3353852180827630 ) ) ;
#1863 = DIRECTION ( 'NONE',  ( 0.000000000000000000, 0.000000000000000000, 1.000000000000000000 ) ) ;
#1864 = ORIENTED_EDGE ( 'NONE', *, *, #14216, .T. ) ;
#1865 = CARTESIAN_POINT ( 'NONE',  ( 784.0799538623451781, 12.19440371013049784, 364.6971507214555572 ) ) ;
#1866 = CARTESIAN_POINT ( 'NONE',  ( 783.7953271457878373, -272.1908817542434917, -375.1787889125761239 ) ) ;
#1867 = ORIENTED_EDGE ( 'NONE', *, *, #39030, .T. ) ;
#1868 = DIRECTION ( 'NONE',  ( 1.000000000000000000, 0.000000000000000000, 0.000000000000000000 ) ) ;
#1869 = CARTESIAN_POINT ( 'NONE',  ( 808.3070685750232087, -234.9982390220561683, 361.1904061080339829 ) ) ;
#1870 = CARTESIAN_POINT ( 'NONE',  ( 796.9571628226829034, -311.4636090269706870, 321.2382568024804641 ) ) ;
#1871 = CARTESIAN_POINT ( 'NONE',  ( 763.2154366446407039, -405.6237781080500326, 321.4292242960311228 ) ) ;
#1872 = EDGE_LOOP ( 'NONE', ( #17747, #14797 ) ) ;
#1873 = CARTESIAN_POINT ( 'NONE',  ( 761.4292242960306112, -113.4636090269712554, -323.2154366446414429 ) ) ;
#1874 = CARTESIAN_POINT ( 'NONE',  ( 764.8639956371174549, -104.0891481129656881, -319.7806653035542013 ) ) ;
#1875 = CARTESIAN_POINT ( 'NONE',  ( 800.2193346964446619, -282.9982390220559409, -355.1360043628816925 ) ) ;
#1876 = ORIENTED_EDGE ( 'NONE', *, *, #25151, .T. ) ;
#1877 = CARTESIAN_POINT ( 'NONE',  ( 804.6798772138708955, -423.7255117493281205, -334.6312213355107019 ) ) ;
#1878 = CARTESIAN_POINT ( 'NONE',  ( 788.8264449731200330, -69.18005720387488111, -363.6646147819171233 ) ) ;
#1879 = CARTESIAN_POINT ( 'NONE',  ( 787.6308680596127942, -299.2601417444139997, 364.1105419155492768 ) ) ;
#1880 = DIRECTION ( 'NONE',  ( 0.000000000000000000, -1.000000000000000000, 0.000000000000000000 ) ) ;
#1881 = AXIS2_PLACEMENT_3D ( 'NONE', #11229, #39189, #39876 ) ;
#1882 = CARTESIAN_POINT ( 'NONE',  ( 772.4999999999993179, -462.9681489794447202, 270.0000000000000568 ) ) ;
#1883 = FACE_OUTER_BOUND ( 'NONE', #18472, .T. ) ;
#1884 = ORIENTED_EDGE ( 'NONE', *, *, #10316, .T. ) ;
#1885 = CARTESIAN_POINT ( 'NONE',  ( 809.0717654672305343, -340.9181544815160123, -360.1688906516309885 ) ) ;
#1886 = CARTESIAN_POINT ( 'NONE',  ( 749.5768839229115201, -204.5545181178800931, 358.0661480581553064 ) ) ;
#1887=STYLED_ITEM('',(#45765),#31946);
#1889 = CARTESIAN_POINT ( 'NONE',  ( 778.1981804954714335, -298.2709662947830793, -314.8072714833589885 ) ) ;
#1888 = DIRECTION ( 'NONE',  ( 0.000000000000000000, 0.3826834323650836756, 0.9238795325112892920 ) ) ;
#1890 = EDGE_CURVE ( 'NONE', #10697, #34810, #20967, .T. ) ;
#1891 = CYLINDRICAL_SURFACE ( 'NONE', #26649, 2.749999999999863665 ) ;
#1892 = CARTESIAN_POINT ( 'NONE',  ( 776.9254006560222479, -140.1908817542438896, -314.8983024940802125 ) ) ;
#1893 = VECTOR ( 'NONE', #35927, 1000.000000000000114 ) ;
#1894 = CARTESIAN_POINT ( 'NONE',  ( 758.8095938919642549, -32.08914811296588709, 311.6929314249763365 ) ) ;
#1895 = DIRECTION ( 'NONE',  ( 0.000000000000000000, 0.000000000000000000, 1.000000000000000000 ) ) ;
#1896 = CARTESIAN_POINT ( 'NONE',  ( 808.0189434323515343, -398.0891481129647218, -319.0252816721025511 ) ) ;
#1897 = CARTESIAN_POINT ( 'NONE',  ( 781.8018195045266339, -46.27096629478404566, 365.1927285166406705 ) ) ;
#1898 = CARTESIAN_POINT ( 'NONE',  ( 786.2694204179717872, -309.2817908451525568, 305.1769319972829067 ) ) ;
#1899 = CARTESIAN_POINT ( 'NONE',  ( 796.9462024416508257, -252.4527844766015789, 308.9653473494370246 ) ) ;
#1900 = CARTESIAN_POINT ( 'NONE',  ( 814.5518280994195948, -15.72551174932958951, -332.4837098697145734 ) ) ;
#1901 = ADVANCED_FACE ( 'NONE', ( #34213 ), #44393, .F. ) ;
#1902 = FACE_BOUND ( 'NONE', #43260, .T. ) ;
#1903 = CARTESIAN_POINT ( 'NONE',  ( 51.16348990802859475, 260.0000000000000568, -191.9749999999945089 ) ) ;
#1904 = CARTESIAN_POINT ( 'NONE',  ( 800.0135310231082713, -350.0891481129648923, 325.0180583372163028 ) ) ;
#1905 = CARTESIAN_POINT ( 'NONE',  ( 796.1575198192839480, -126.0090635724257737, 359.4546378042384163 ) ) ;
#1906 = CARTESIAN_POINT ( 'NONE',  ( 804.9511171171677688, -5.805596289869448867, -335.8780910478229202 ) ) ;
#1907 = AXIS2_PLACEMENT_3D ( 'NONE', #37509, #40532, #8881 ) ;
#1908 = LINE ( 'NONE', #16016, #40236 ) ;
#1909 = FACE_OUTER_BOUND ( 'NONE', #17632, .T. ) ;
#1910 = CARTESIAN_POINT ( 'NONE',  ( 781.2497674668890113, -132.3510508353235764, 375.3608509340180603 ) ) ;
#1911 = CARTESIAN_POINT ( 'NONE',  ( 759.9864689768902508, -410.0891481129647218, 354.9819416627836404 ) ) ;
#1912 = EDGE_LOOP ( 'NONE', ( #2855, #11798 ) ) ;
#1913 = CARTESIAN_POINT ( 'NONE',  ( 805.1927285166397041, -40.81642084023859951, -341.8018195045277707 ) ) ;
#1914 = AXIS2_PLACEMENT_3D ( 'NONE', #1279, #25296, #17927 ) ;
#1915 = CARTESIAN_POINT ( 'NONE',  ( 802.7791456095903868, -316.7146871989593819, -329.0155153010375102 ) ) ;
#1917 = CARTESIAN_POINT ( 'NONE',  ( 778.2165204200184689, -142.8164208402382656, 364.9363028652563230 ) ) ;
#1916 = CARTESIAN_POINT ( 'NONE',  ( 804.9363028652555840, -160.2709662947836762, 338.2165204200192079 ) ) ;
#1918 = UNCERTAINTY_MEASURE_WITH_UNIT (LENGTH_MEASURE( 1.000000000000000082E-05 ), #28708, 'distance_accuracy_value', 'NONE');
#1919 = CARTESIAN_POINT ( 'NONE',  ( 771.2368401574024119, -325.4419599262320162, -374.2805881961240857 ) ) ;
#1920 = DIRECTION ( 'NONE',  ( 1.000000000000000000, 0.000000000000000000, 0.000000000000000000 ) ) ;
#1921 = ORIENTED_EDGE ( 'NONE', *, *, #37141, .F. ) ;
#1922 = CARTESIAN_POINT ( 'NONE',  ( 768.0187753319979720, -344.6346026584195101, 318.0580252608186242 ) ) ;
#1923 = VECTOR ( 'NONE', #5270, 1000.000000000000114 ) ;
#1924 = ORIENTED_EDGE ( 'NONE', *, *, #9522, .F. ) ;
#1925 =( NAMED_UNIT ( * ) SI_UNIT ( $, .STERADIAN. ) SOLID_ANGLE_UNIT ( ) );
#1926 = AXIS2_PLACEMENT_3D ( 'NONE', #2058, #12918, #37160 ) ;
#1927 = CARTESIAN_POINT ( 'NONE',  ( 763.0537975583475827, -192.4527844766016926, -371.0346526505627480 ) ) ;
#1928 = CARTESIAN_POINT ( 'NONE',  ( 749.2812353651451076, -126.4527844766019626, 323.2262854647983090 ) ) ;
#1929 = EDGE_LOOP ( 'NONE', ( #4719, #16342 ) ) ;
#1930 = CARTESIAN_POINT ( 'NONE',  ( 767.8955696845334842, -168.4527844766018347, -362.1676090361161755 ) ) ;
#1931 = VERTEX_POINT ( 'NONE', #26828 ) ;
#1932 = CARTESIAN_POINT ( 'NONE',  ( 785.3687786644884454, 12.63812461430668321, -315.3201227861279676 ) ) ;
#1933 = CARTESIAN_POINT ( 'NONE',  ( 815.2698199232961542, -256.8164208402379245, 342.5225473063383106 ) ) ;
#1934 = CARTESIAN_POINT ( 'NONE',  ( 804.1601925771018387, -175.4419599262325562, 346.5483106153029098 ) ) ;
#1936 = CARTESIAN_POINT ( 'NONE',  ( 571.1634899080285095, 259.9999999999999432, -191.9749999999982037 ) ) ;
#1935 = DIRECTION ( 'NONE',  ( 0.000000000000000000, 0.000000000000000000, 1.000000000000000000 ) ) ;
#1937 = MANIFOLD_SOLID_BREP ( '<Slot>-<Boss-Extrude21>', #29843 ) ;
#1938 = ORIENTED_EDGE ( 'NONE', *, *, #17991, .F. ) ;
#1939 = CARTESIAN_POINT ( 'NONE',  ( 787.5531968255692163, -429.8272453906067199, -316.1348686366205811 ) ) ;
#1940 = DIRECTION ( 'NONE',  ( 0.000000000000000000, 0.000000000000000000, -1.000000000000000000 ) ) ;
#1941 = ORIENTED_EDGE ( 'NONE', *, *, #25313, .F. ) ;
#1942 = CARTESIAN_POINT ( 'NONE',  ( 764.1737431748507561, -226.3726999360617924, -371.6461892240376415 ) ) ;
#1943 = CARTESIAN_POINT ( 'NONE',  ( 797.8822607201568644, -102.5545181178804057, 370.1134526219340160 ) ) ;
#1944 = CIRCLE ( 'NONE', #7884, 10.00000000000000888 ) ;
#1946 = CARTESIAN_POINT ( 'NONE',  ( 756.5762568750052424, -195.1800572038744974, -348.7366044899774238 ) ) ;
#1945 = DIRECTION ( 'NONE',  ( -1.000000000000000000, -0.000000000000000000, -0.000000000000000000 ) ) ;
#1947 = CARTESIAN_POINT ( 'NONE',  ( 802.7791456095903868, -364.7146871989592114, -329.0155153010375102 ) ) ;
#1948 = CARTESIAN_POINT ( 'NONE',  ( -190.7583438952259485, 394.6698570112193920, -274.9999999999999432 ) ) ;
#1949 = CARTESIAN_POINT ( 'NONE',  ( 754.3581564841646241, -233.4636090269708575, -316.1443688327762516 ) ) ;
#1950 = LINE ( 'NONE', #5881, #31862 ) ;
#1951 = CARTESIAN_POINT ( 'NONE',  ( 999.9999999999992042, -600.0000000000001137, 359.0000000000000000 ) ) ;
#1952 = CARTESIAN_POINT ( 'NONE',  ( 786.5483106153019435, -55.64542720878963422, -364.1601925771022366 ) ) ;
#1953 = AXIS2_PLACEMENT_3D ( 'NONE', #25021, #7703, #5081 ) ;
#1954 = CARTESIAN_POINT ( 'NONE',  ( 784.1219089521767955, -429.2817908451521021, 315.0488828828318333 ) ) ;
#1955 = EDGE_CURVE ( 'NONE', #29157, #346, #26860, .T. ) ;
#1956 = CARTESIAN_POINT ( 'NONE',  ( 792.2312462859673587, -251.9073299311470748, -307.2067596250082602 ) ) ;
#1957 = CARTESIAN_POINT ( 'NONE',  ( 793.0897708529556667, -246.5545181178799510, 361.3366627262616362 ) ) ;
#1958 = DIRECTION ( 'NONE',  ( 0.000000000000000000, -1.000000000000000000, 0.000000000000000000 ) ) ;
#1959 = DIRECTION ( 'NONE',  ( 0.000000000000000000, -0.3826834323650836756, -0.9238795325112892920 ) ) ;
#1960 = CARTESIAN_POINT ( 'NONE',  ( 778.1981804954714335, -58.27096629478398171, -314.8072714833589885 ) ) ;
#1961 = CIRCLE ( 'NONE', #14553, 4.999999999999982236 ) ;
#1962 = CARTESIAN_POINT ( 'NONE',  ( 771.3260364891663130, -163.6454272087893003, 306.0683387631859773 ) ) ;
#1963 = CARTESIAN_POINT ( 'NONE',  ( 744.9990715423526808, -138.3510508353236048, -341.2370466360926002 ) ) ;
#1964 = CARTESIAN_POINT ( 'NONE',  ( 804.7487373415286811, -163.5436935675109567, 364.7487373415288516 ) ) ;
#1965 = CARTESIAN_POINT ( 'NONE',  ( 754.9967657858570647, -385.5436935675102745, -365.0032342141425374 ) ) ;
#1966 = VECTOR ( 'NONE', #876, 1000.000000000000000 ) ;
#1967 = DIRECTION ( 'NONE',  ( -0.000000000000000000, 1.000000000000000000, -0.000000000000000000 ) ) ;
#1968 = CARTESIAN_POINT ( 'NONE',  ( 804.4286716492782716, -257.3618753856924286, 345.3141322388244703 ) ) ;
#1969 = CARTESIAN_POINT ( 'NONE',  ( 763.0428371773158460, -11.46360902697159290, 358.7617431975195359 ) ) ;
#1970 = CARTESIAN_POINT ( 'NONE',  ( 781.8018195045266339, -406.2709662947829088, -365.1927285166406705 ) ) ;
#1971 = DIRECTION ( 'NONE',  ( 0.000000000000000000, 0.000000000000000000, 1.000000000000000000 ) ) ;
#1972 = CARTESIAN_POINT ( 'NONE',  ( 793.3938497862117174, -453.0432664090020012, -372.3358127763067955 ) ) ;
#1973 = CARTESIAN_POINT ( 'NONE',  ( 1820.038553321469863, -418.3138125091624602, -201.9999999999998863 ) ) ;
#1974 = CARTESIAN_POINT ( 'NONE',  ( 775.9200461376533440, -71.80559628986922860, 315.3028492785443291 ) ) ;
#1975 = ORIENTED_EDGE ( 'NONE', *, *, #8593, .F. ) ;
#1976 = CARTESIAN_POINT ( 'NONE',  ( 765.8855110935204493, -214.1692326535052189, -319.0159684113471599 ) ) ;
#1977 = CARTESIAN_POINT ( 'NONE',  ( 759.7806653035534055, -126.9982390220565094, -324.8639956371180801 ) ) ;
#1978 = CARTESIAN_POINT ( 'NONE',  ( 788.7366044899766848, -59.90732993114762905, 316.5762568750059813 ) ) ;
#1979 = CARTESIAN_POINT ( 'NONE',  ( 746.7653713866222915, -209.2601417444142839, -351.0478386215610271 ) ) ;
#1980 = CARTESIAN_POINT ( 'NONE',  ( 744.9990715423526808, -378.3510508353227806, 341.2370466360926002 ) ) ;
#1981 = ORIENTED_EDGE ( 'NONE', *, *, #5195, .T. ) ;
#1982 = AXIS2_PLACEMENT_3D ( 'NONE', #35770, #7151, #28373 ) ;
#1983 = CARTESIAN_POINT ( 'NONE',  ( 772.5602148656447525, 14.27448825067031812, 305.7998596910095443 ) ) ;
#1984 = CARTESIAN_POINT ( 'NONE',  ( 803.4237431249931660, -159.1800572038746111, -331.2633955100225194 ) ) ;
#1985 = CARTESIAN_POINT ( 'NONE',  ( 791.9812246680005501, -356.6346026584193964, 361.9419747391813189 ) ) ;
#1986 = AXIS2_PLACEMENT_3D ( 'NONE', #13107, #16800, #33423 ) ;
#1987 = CARTESIAN_POINT ( 'NONE',  ( 808.0189434323515343, -86.08914811296573077, -319.0252816721025511 ) ) ;
#1988 = CARTESIAN_POINT ( 'NONE',  ( 788.7366044899766848, -83.90732993114754379, -316.5762568750059813 ) ) ;
#1989 = ORIENTED_EDGE ( 'NONE', *, *, #19944, .T. ) ;
#1990 = CARTESIAN_POINT ( 'NONE',  ( 793.9708237608222134, -22.91815448151701062, -319.2295555964448681 ) ) ;
#1991 = AXIS2_PLACEMENT_3D ( 'NONE', #31297, #3813, #21817 ) ;
#1992 = ORIENTED_EDGE ( 'NONE', *, *, #34285, .F. ) ;
#1993 = CARTESIAN_POINT ( 'NONE',  ( 786.5483106153019435, -343.6454272087887603, -364.1601925771022366 ) ) ;
#1995 = CARTESIAN_POINT ( 'NONE',  ( 775.8780910478218402, -393.2817908451522726, 364.9511171171680530 ) ) ;
#1994 = CARTESIAN_POINT ( 'NONE',  ( 756.3353852180819104, -77.90732993114757221, 331.1735550268788302 ) ) ;
#1996 = CIRCLE ( 'NONE', #10121, 9.999999999999982236 ) ;
#1999 = CARTESIAN_POINT ( 'NONE',  ( 801.9858362298568863, -315.0783235625957559, 312.7379699480935642 ) ) ;
#1998 = DIRECTION ( 'NONE',  ( 1.000000000000000000, 0.000000000000000000, -0.000000000000000000 ) ) ;
#1997 = CARTESIAN_POINT ( 'NONE',  ( 805.0032342141413437, -445.5436935675099335, 314.9967657858572352 ) ) ;
#2000 = CARTESIAN_POINT ( 'NONE',  ( 796.9571628226829034, -335.4636090269705733, -321.2382568024804641 ) ) ;
#2001 = CARTESIAN_POINT ( 'NONE',  ( 764.8639956371174549, -320.0891481129648355, -319.7806653035542013 ) ) ;
#2002 = CARTESIAN_POINT ( 'NONE',  ( 774.6312213355099630, -143.3618753856927697, -364.6798772138717482 ) ) ;
#2003 = CARTESIAN_POINT ( 'NONE',  ( 744.6391490659812007, -14.73633629969885384, 338.7502325331110455 ) ) ;
#2005 = LINE ( 'NONE', #36893, #4197 ) ;
#2004 = DIRECTION ( 'NONE',  ( 0.000000000000000000, 1.000000000000000000, 1.110223024625155554E-15 ) ) ;
#2006 = CARTESIAN_POINT ( 'NONE',  ( 784.0799538623451781, -275.8055962898685038, -364.6971507214555572 ) ) ;
#2007 = CARTESIAN_POINT ( 'NONE',  ( 752.7379699480933368, -108.0090635724258448, -361.9858362298580232 ) ) ;
#2008 = CARTESIAN_POINT ( 'NONE',  ( -28.63011601220122415, -501.1515549466498669, -368.0974687824633520 ) ) ;
#2009 = PLANE ( 'NONE',  #5339 ) ;
#2010 = CARTESIAN_POINT ( 'NONE',  ( 798.5707757039680246, -293.4636090269707438, 356.7845633553585003 ) ) ;
#2011 = CARTESIAN_POINT ( 'NONE',  ( 778.1981804954714335, -178.2709662947835625, 314.8072714833589885 ) ) ;
#2012 = ORIENTED_EDGE ( 'NONE', *, *, #14906, .F. ) ;
#2013 = CARTESIAN_POINT ( 'NONE',  ( 804.1009440267234822, -263.4636090269708006, 314.0944755984392600 ) ) ;
#2014 = CARTESIAN_POINT ( 'NONE',  ( 810.7187646348534145, -138.4527844766019200, -356.7737145352016341 ) ) ;
#2015 = DIRECTION ( 'NONE',  ( 1.892425610156518354E-16, 1.000000000000000000, -0.000000000000000000 ) ) ;
#2016 = CARTESIAN_POINT ( 'NONE',  ( 809.0717654672305343, -76.91815448151683654, 360.1688906516309885 ) ) ;
#2018 = VECTOR ( 'NONE', #9854, 1000.000000000000000 ) ;
#2017 = CARTESIAN_POINT ( 'NONE',  ( 815.2698199232961542, -256.8164208402379245, -342.5225473063383106 ) ) ;
#2019 = CARTESIAN_POINT ( 'NONE',  ( 779.9999999999992042, 16.45630643248849267, 339.9999999999999432 ) ) ;
#2020 = CARTESIAN_POINT ( 'NONE',  ( 805.1927285166397041, -160.8164208402382371, 341.8018195045277707 ) ) ;
#2021 = ORIENTED_EDGE ( 'NONE', *, *, #18268, .F. ) ;
#2022 = CARTESIAN_POINT ( 'NONE',  ( 749.8865473780648472, -332.5328690171411381, -322.1177392798429082 ) ) ;
#2023 = AXIS2_PLACEMENT_3D ( 'NONE', #40515, #8866, #22932 ) ;
#2024 = CARTESIAN_POINT ( 'NONE',  ( 744.7301800767019131, -100.8164208402383792, -337.4774526936615757 ) ) ;
#2025 = CARTESIAN_POINT ( 'NONE',  ( 796.9571628226829034, -23.46360902697155026, 321.2382568024804641 ) ) ;
#2026 = CARTESIAN_POINT ( 'NONE',  ( 763.2262854647970016, -368.6346026584193964, -309.2812353651462445 ) ) ;
#2027 = DIRECTION ( 'NONE',  ( 0.000000000000000000, 0.000000000000000000, 1.000000000000000000 ) ) ;
#2028 = CARTESIAN_POINT ( 'NONE',  ( 794.1144889064781864, -418.1692326535044799, 360.9840315886528401 ) ) ;
#2029 = ORIENTED_EDGE ( 'NONE', *, *, #37278, .F. ) ;
#2030 = ADVANCED_FACE ( 'NONE', ( #37471 ), #16221, .F. ) ;
#2031 = CARTESIAN_POINT ( 'NONE',  ( 766.5853460496234675, -109.9874144716873019, -372.3518521366060554 ) ) ;
#2032 = LINE ( 'NONE', #16126, #38083 ) ;
#2033 = CARTESIAN_POINT ( 'NONE',  ( 795.6651683502461765, -226.7146871989596661, 371.3240766477733814 ) ) ;
#2034 = CARTESIAN_POINT ( 'NONE',  ( 762.1405469898973024, -73.54369356751121245, 357.8594530101016176 ) ) ;
#2035 = ORIENTED_EDGE ( 'NONE', *, *, #26712, .F. ) ;
#2036 = VERTEX_POINT ( 'NONE', #19918 ) ;
#2037 = CARTESIAN_POINT ( 'NONE',  ( 761.2382568024794409, -15.62377810805123524, -356.9571628226838129 ) ) ;
#2038 = CARTESIAN_POINT ( 'NONE',  ( 762.1405469898971887, -265.5436935675106156, 357.8594530101015607 ) ) ;
#2039 = CARTESIAN_POINT ( 'NONE',  ( 744.9990715423526808, -426.3510508353226669, -341.2370466360926002 ) ) ;
#2040 = FACE_OUTER_BOUND ( 'NONE', #4448, .T. ) ;
#2041 = ORIENTED_EDGE ( 'NONE', *, *, #11895, .F. ) ;
#2042 = ORIENTED_EDGE ( 'NONE', *, *, #43308, .F. ) ;
#2043 = CARTESIAN_POINT ( 'NONE',  ( 757.7880784355613741, -378.0090635724250774, -312.4576283171834916 ) ) ;
#2044 = CARTESIAN_POINT ( 'NONE',  ( 805.1927285166397041, -232.8164208402379245, -341.8018195045277707 ) ) ;
#2046 = CARTESIAN_POINT ( 'NONE',  ( 781.2497674668890113, -228.3510508353232922, 375.3608509340180603 ) ) ;
#2045 = CARTESIAN_POINT ( 'NONE',  ( 748.9653473494365699, -338.6346026584195101, 356.9462024416520762 ) ) ;
#2047 = ADVANCED_FACE ( 'NONE', ( #2347 ), #8632, .F. ) ;
#2048 = CARTESIAN_POINT ( 'NONE',  ( 761.9338519418445230, -38.53286901714206891, 370.4231160770881957 ) ) ;
#2049 = CARTESIAN_POINT ( 'NONE',  ( 786.5483106153019435, -223.6454272087891013, -364.1601925771022366 ) ) ;
#2050 = CARTESIAN_POINT ( 'NONE',  ( 781.7834795799800531, -226.8164208402380098, -315.0636971347436202 ) ) ;
#2051 = CARTESIAN_POINT ( 'NONE',  ( 781.7834795799800531, -418.8164208402374129, -315.0636971347436202 ) ) ;
#2052 = ORIENTED_EDGE ( 'NONE', *, *, #41702, .T. ) ;
#2053 = CARTESIAN_POINT ( 'NONE',  ( 803.6646147819161570, -209.9073299311470748, 348.8264449731210561 ) ) ;
#2054 = CARTESIAN_POINT ( 'NONE',  ( 788.8264449731200330, -93.18005720387481006, -363.6646147819171233 ) ) ;
#2055 = ORIENTED_EDGE ( 'NONE', *, *, #24398, .F. ) ;
#2056 = AXIS2_PLACEMENT_3D ( 'NONE', #19204, #36975, #15306 ) ;
#2057 = CARTESIAN_POINT ( 'NONE',  ( 758.8095938919642549, -320.0891481129648355, 311.6929314249763365 ) ) ;
#2058 = CARTESIAN_POINT ( 'NONE',  ( -786.4999999999993179, -512.9681489794448908, -339.9999999999999432 ) ) ;
#2059 = FACE_BOUND ( 'NONE', #7636, .T. ) ;
#2060 = CARTESIAN_POINT ( 'NONE',  ( 51.16348990802859475, 260.0000000000000568, -208.0249999999945203 ) ) ;
#2061 = EDGE_CURVE ( 'NONE', #2904, #27191, #30531, .T. ) ;
#2062 = CARTESIAN_POINT ( 'NONE',  ( 754.7162404726377645, -182.7363362996983369, 339.4709603349214717 ) ) ;
#2063 = CARTESIAN_POINT ( 'NONE',  ( 759.9864689768902508, -74.08914811296577341, 354.9819416627836404 ) ) ;
#2064 = VERTEX_POINT ( 'NONE', #22914 ) ;
#2065 = CARTESIAN_POINT ( 'NONE',  ( 809.0717654672305343, -460.9181544815156713, -360.1688906516309885 ) ) ;
#2066 = CARTESIAN_POINT ( 'NONE',  ( 763.0537975583476964, -24.45278447660228949, -371.0346526505628617 ) ) ;
#2067 = CARTESIAN_POINT ( 'NONE',  ( 804.9511171171677688, -269.8055962898686175, 335.8780910478229202 ) ) ;
#2068 = CARTESIAN_POINT ( 'NONE',  ( 804.6798772138708955, -399.7255117493283478, -334.6312213355107019 ) ) ;
#2069 = CARTESIAN_POINT ( 'NONE',  ( 795.1360043628808398, 3.910851887033986785, -360.2193346964456282 ) ) ;
#2070 = CARTESIAN_POINT ( 'NONE',  ( 755.2512626584698410, -415.5436935675102177, 315.2512626584710915 ) ) ;
#2071 = DIRECTION ( 'NONE',  ( -0.000000000000000000, 1.000000000000000000, -0.000000000000000000 ) ) ;
#2072 = CARTESIAN_POINT ( 'NONE',  ( 802.5472867521000353, -292.3726999360616219, -350.8726784830461156 ) ) ;
#2073 = CARTESIAN_POINT ( 'NONE',  ( 746.8695393053150156, -149.9073299311473875, -327.6429770376306010 ) ) ;
#2074 = CARTESIAN_POINT ( 'NONE',  ( 787.4397851343537695, -69.72551174932942786, 374.2001403089903988 ) ) ;
#2075 = CARTESIAN_POINT ( 'NONE',  ( 744.7301800767019131, -148.8164208402382656, 337.4774526936615757 ) ) ;
#2076 = CARTESIAN_POINT ( 'NONE',  ( 772.1467562141141343, 16.45630643248850689, -315.9110025235851253 ) ) ;
#2077 = DIRECTION ( 'NONE',  ( 0.000000000000000000, 0.000000000000000000, -1.000000000000000000 ) ) ;
#2078 = EDGE_CURVE ( 'NONE', #27436, #32644, #12994, .T. ) ;
#2079 = EDGE_CURVE ( 'NONE', #40848, #12356, #33501, .T. ) ;
#2080 = DIRECTION ( 'NONE',  ( 1.000000000000000000, 0.000000000000000000, 0.000000000000000000 ) ) ;
#2081 = CARTESIAN_POINT ( 'NONE',  ( 800.9747183278959710, -396.9982390220556567, 311.9810565676471583 ) ) ;
#2082 = CARTESIAN_POINT ( 'NONE',  ( 796.9462024416508257, -12.45278447660232324, 308.9653473494370246 ) ) ;
#2083 = CARTESIAN_POINT ( 'NONE',  ( 756.3353852180819104, -365.9073299311465917, -331.1735550268788302 ) ) ;
#2084 = CARTESIAN_POINT ( 'NONE',  ( 775.9200461376533440, 24.19440371013046231, 315.3028492785443291 ) ) ;
#2085 = ADVANCED_FACE ( 'NONE', ( #40494 ), #20136, .T. ) ;
#2086 = CARTESIAN_POINT ( 'NONE',  ( 755.8990559732751535, -107.4636090269713122, -365.9055244015606831 ) ) ;
#2087 = CARTESIAN_POINT ( 'NONE',  ( 763.2154366446407039, -165.6237781080507716, -321.4292242960311228 ) ) ;
#2088 = CARTESIAN_POINT ( 'NONE',  ( 813.9316612368132837, -151.4419599262326415, 348.6739635108323228 ) ) ;
#2089 = DIRECTION ( 'NONE',  ( -1.000000000000000000, 0.000000000000000000, 0.000000000000000000 ) ) ;
#2090 = AXIS2_PLACEMENT_3D ( 'NONE', #42506, #28870, #17797 ) ;
#2091 = CARTESIAN_POINT ( 'NONE',  ( 812.6845335610512393, -175.9874144716871172, 353.5525998758768651 ) ) ;
#2092 = CARTESIAN_POINT ( 'NONE',  ( 795.1360043628807261, -44.08914811296584446, -360.2193346964456282 ) ) ;
#2093 = CARTESIAN_POINT ( 'NONE',  ( 801.3366627262608972, -176.5328690171416213, -353.0897708529566899 ) ) ;
#2094 = CARTESIAN_POINT ( 'NONE',  ( 788.8264449731200330, -141.1800572038746395, -363.6646147819171233 ) ) ;
#2095 = CARTESIAN_POINT ( 'NONE',  ( 754.8072714833581358, -148.8164208402382656, 338.1981804954720587 ) ) ;
#2096 = CARTESIAN_POINT ( 'NONE',  ( 804.1601925771018387, -439.4419599262316751, -346.5483106153029098 ) ) ;
#2097 = CARTESIAN_POINT ( 'NONE',  ( 756.3353852180820240, -293.9073299311468759, 331.1735550268787733 ) ) ;
#2098 = FACE_OUTER_BOUND ( 'NONE', #12227, .T. ) ;
#2099 = VERTEX_POINT ( 'NONE', #40706 ) ;
#2100 = CARTESIAN_POINT ( 'NONE',  ( 763.2154366446407039, 26.37622189194863509, 321.4292242960311228 ) ) ;
#2101 = CARTESIAN_POINT ( 'NONE',  ( 781.2370466360911223, -260.7363362996981095, -304.9990715423533629 ) ) ;
#2102 = EDGE_CURVE ( 'NONE', #21705, #35766, #8461, .T. ) ;
#2103 = VERTEX_POINT ( 'NONE', #5150 ) ;
#2104 = DIRECTION ( 'NONE',  ( 0.000000000000000000, 0.000000000000000000, 1.000000000000000000 ) ) ;
#2105 = CARTESIAN_POINT ( 'NONE',  ( 747.2067596250078623, -219.1800572038744122, 352.2312462859687230 ) ) ;
#2106 = EDGE_CURVE ( 'NONE', #10247, #12793, #44588, .T. ) ;
#2107 = CARTESIAN_POINT ( 'NONE',  ( 796.1575198192839480, -294.0090635724253048, 359.4546378042384163 ) ) ;
#2108 = CARTESIAN_POINT ( 'NONE',  ( 794.1144889064781864, -394.1692326535045368, 360.9840315886528401 ) ) ;
#2109 = ORIENTED_EDGE ( 'NONE', *, *, #27219, .T. ) ;
#2110 = CARTESIAN_POINT ( 'NONE',  ( 804.8461984189677878, -122.1908817542439749, -336.9566956441385628 ) ) ;
#2111 = CARTESIAN_POINT ( 'NONE',  ( 757.8323909638827445, -98.63460265842024910, -352.1044303154654358 ) ) ;
#2112 = CARTESIAN_POINT ( 'NONE',  ( 800.0135310231082713, -278.0891481129651197, -325.0180583372163028 ) ) ;
#2113 = ORIENTED_EDGE ( 'NONE', *, *, #11760, .T. ) ;
#2114 = CARTESIAN_POINT ( 'NONE',  ( 800.0135310231082713, -422.0891481129647218, -325.0180583372163028 ) ) ;
#2115 = CARTESIAN_POINT ( 'NONE',  ( 759.7806653035534055, -78.99823902205662307, -324.8639956371180801 ) ) ;
#2116 = CARTESIAN_POINT ( 'NONE',  ( 772.3691319403857278, -311.2601417444139429, 315.8894580844506663 ) ) ;
#2117 = EDGE_CURVE ( 'NONE', #32983, #10586, #6970, .T. ) ;
#2118 = DIRECTION ( 'NONE',  ( 0.000000000000000000, 0.000000000000000000, -1.000000000000000000 ) ) ;
#2119 = LINE ( 'NONE', #11845, #11580 ) ;
#2120 = EDGE_CURVE ( 'NONE', #38502, #44613, #35364, .T. ) ;
#2121 = CARTESIAN_POINT ( 'NONE',  ( 809.9999999999993179, -512.9681489794448908, -329.9999999999999432 ) ) ;
#2122 = VERTEX_POINT ( 'NONE', #30995 ) ;
#2123 = CARTESIAN_POINT ( 'NONE',  ( 752.7379699480933368, -348.0090635724251342, -361.9858362298580232 ) ) ;
#2124 = CARTESIAN_POINT ( 'NONE',  ( 750.9282345327678740, -208.9181544815164102, 319.8311093483690115 ) ) ;
#2125 = CIRCLE ( 'NONE', #8059, 20.00000000000004619 ) ;
#2126 = CARTESIAN_POINT ( 'NONE',  ( 785.3687786644884454, -299.3618753856922581, -315.3201227861279676 ) ) ;
#2127 = FACE_OUTER_BOUND ( 'NONE', #44437, .T. ) ;
#2128 = CARTESIAN_POINT ( 'NONE',  ( 780.5236548040995785, -188.7363362996983085, -314.9735926884559944 ) ) ;
#2129 = CARTESIAN_POINT ( 'NONE',  ( 767.7687537140311633, -47.90732993114767169, 372.7932403749916830 ) ) ;
#2130 = DIRECTION ( 'NONE',  ( -0.000000000000000000, -0.6438296778008192334, 0.7651688349527135946 ) ) ;
#2131 = CARTESIAN_POINT ( 'NONE',  ( 751.6929314249750860, -366.9982390220557136, -318.8095938919659034 ) ) ;
#2132 = CARTESIAN_POINT ( 'NONE',  ( 792.1044303154645831, -60.45278447660215448, 317.8323909638837677 ) ) ;
#2133 = CARTESIAN_POINT ( 'NONE',  ( 747.6481478633932056, -325.0999726633342561, 353.4146539503763620 ) ) ;
#2134 = ADVANCED_FACE ( 'NONE', ( #45556 ), #45093, .F. ) ;
#2135 = CARTESIAN_POINT ( 'NONE',  ( 745.0891759886404770, -268.2709662947833067, 342.4968714119734159 ) ) ;
#2136 = CARTESIAN_POINT ( 'NONE',  ( 772.5602148656447525, -33.72551174932952733, -305.7998596910095443 ) ) ;
#2137 = CARTESIAN_POINT ( 'NONE',  ( 768.0187753319979720, -248.6346026584197659, -318.0580252608186242 ) ) ;
#2138 = DIRECTION ( 'NONE',  ( -1.000000000000000000, 0.000000000000000000, -0.000000000000000000 ) ) ;
#2139 = CARTESIAN_POINT ( 'NONE',  ( 757.8323909638827445, -362.6346026584194533, 352.1044303154654358 ) ) ;
#2140 = CARTESIAN_POINT ( 'NONE',  ( 757.4527132478984868, -112.3726999360621761, 329.1273215169538844 ) ) ;
#2141 = CARTESIAN_POINT ( 'NONE',  ( 754.8983024940795303, -42.89650538077842157, -336.9254006560228163 ) ) ;
#2142 = CARTESIAN_POINT ( 'NONE',  ( 746.0683387631852383, -43.44195992623296831, 331.3260364891676204 ) ) ;
#2143 = CARTESIAN_POINT ( 'NONE',  ( 755.3201227861273992, -387.7255117493284047, 345.3687786644892981 ) ) ;
#2144 = CARTESIAN_POINT ( 'NONE',  ( 769.9999999999992042, 178.9475563372491251, 320.0000000000000000 ) ) ;
#2145 = CARTESIAN_POINT ( 'NONE',  ( 799.9999999999993179, -512.9681489794448908, 339.9999999999999432 ) ) ;
#2146 = CARTESIAN_POINT ( 'NONE',  ( 762.3223304703356007, -391.5436935675101608, 322.3223304703362828 ) ) ;
#2147 = ORIENTED_EDGE ( 'NONE', *, *, #33217, .T. ) ;
#2148 = CARTESIAN_POINT ( 'NONE',  ( 793.2243759319678702, -338.5328690171411381, -318.4439275373583200 ) ) ;
#2150 = CARTESIAN_POINT ( 'NONE',  ( 759.9864689768902508, -146.0891481129655176, 354.9819416627836404 ) ) ;
#2149 = CARTESIAN_POINT ( 'NONE',  ( 805.1927285166397041, -208.8164208402380666, 341.8018195045277707 ) ) ;
#2151 = CARTESIAN_POINT ( 'NONE',  ( 791.1614460488616487, -347.2601417444138860, -373.5763878283158874 ) ) ;
#2152 = CARTESIAN_POINT ( 'NONE',  ( 180.7583438952258348, 394.6698570112193920, -274.9999999999999432 ) ) ;
#2153 = ORIENTED_EDGE ( 'NONE', *, *, #42791, .T. ) ;
#2154 = CARTESIAN_POINT ( 'NONE',  ( 785.3687786644884454, -371.3618753856919739, 315.3201227861279676 ) ) ;
#2155 = AXIS2_PLACEMENT_3D ( 'NONE', #9924, #17090, #45047 ) ;
#2156 = ADVANCED_FACE ( 'NONE', ( #6514 ), #3046, .F. ) ;
#2157 = ORIENTED_EDGE ( 'NONE', *, *, #14016, .F. ) ;
#2158 = CARTESIAN_POINT ( 'NONE',  ( 792.3570229623688874, -213.1800572038743553, -373.1304606946836202 ) ) ;
#2159 = CARTESIAN_POINT ( 'NONE',  ( 801.1904061080338124, -116.0891481129656313, 368.3070685750236066 ) ) ;
#2160 = EDGE_CURVE ( 'NONE', #33957, #338, #42375, .T. ) ;
#2161 = ORIENTED_EDGE ( 'NONE', *, *, #35912, .F. ) ;
#2162 = CARTESIAN_POINT ( 'NONE',  ( 802.1676090361155502, -182.6346026584199649, -327.8955696845344505 ) ) ;
#2163 = EDGE_LOOP ( 'NONE', ( #2260, #40842 ) ) ;
#2164 = CARTESIAN_POINT ( 'NONE',  ( 755.0636971347428243, -340.2709662947831362, -341.7834795799807353 ) ) ;
#2165 = CARTESIAN_POINT ( 'NONE',  ( 774.6858677611749044, 14.27448825067031812, -315.5713283507209894 ) ) ;
#2166 = CARTESIAN_POINT ( 'NONE',  ( 754.9967657858570647, -265.5436935675106156, 365.0032342141425374 ) ) ;
#2167 = CARTESIAN_POINT ( 'NONE',  ( 759.2295555964440155, -184.1692326535052757, 353.9708237608231229 ) ) ;
#2169 = PLANE ( 'NONE',  #26255 ) ;
#2168 = DIRECTION ( 'NONE',  ( -0.000000000000000000, -0.000000000000000000, 1.000000000000000000 ) ) ;
#2170 = CARTESIAN_POINT ( 'NONE',  ( 791.7608162188021197, 178.9475563372491251, -360.0000000000000000 ) ) ;
#2171 = VERTEX_POINT ( 'NONE', #27982 ) ;
#2172 = CARTESIAN_POINT ( 'NONE',  ( 804.4086373105744769, -433.6454272087884760, -333.3843516231986541 ) ) ;
#2173 = FACE_OUTER_BOUND ( 'NONE', #43522, .T. ) ;
#2174 = FACE_OUTER_BOUND ( 'NONE', #8874, .T. ) ;
#2175 = EDGE_LOOP ( 'NONE', ( #2685, #9652 ) ) ;
#2176 = CARTESIAN_POINT ( 'NONE',  ( 793.5525998758768083, -223.0999726633346256, -372.6845335610516941 ) ) ;
#2177 = CARTESIAN_POINT ( 'NONE',  ( 810.4231160770870019, -96.55451811788039151, 321.9338519418446936 ) ) ;
#2179 = CARTESIAN_POINT ( 'NONE',  ( 768.0187753319979720, -200.6346026584199365, -318.0580252608186242 ) ) ;
#2178 = CARTESIAN_POINT ( 'NONE',  ( 265.7583438952258916, 430.0000000000002842, -244.9999999999999716 ) ) ;
#2180 = CARTESIAN_POINT ( 'NONE',  ( 801.3366627262608972, -368.5328690171409676, -353.0897708529566899 ) ) ;
#2181 = DIRECTION ( 'NONE',  ( 5.551115123125783688E-16, -1.000000000000000000, 0.000000000000000000 ) ) ;
#2182 = CARTESIAN_POINT ( 'NONE',  ( 746.4236121716829757, -207.8272453906073451, -328.8385539511384650 ) ) ;
#2183 = DIRECTION ( 'NONE',  ( 0.000000000000000000, 0.000000000000000000, 1.000000000000000000 ) ) ;
#2184 = DIRECTION ( 'NONE',  ( 0.000000000000000000, 0.000000000000000000, 1.000000000000000000 ) ) ;
#2185 = CARTESIAN_POINT ( 'NONE',  ( 787.5531968255692163, -93.82724539060770041, -316.1348686366205811 ) ) ;
#2186 = CARTESIAN_POINT ( 'NONE',  ( 759.0159684113467620, -424.9181544815158986, 325.8855110935213020 ) ) ;
#2187 = DIRECTION ( 'NONE',  ( 1.892425610156518354E-16, 1.000000000000000000, -0.000000000000000000 ) ) ;
#2188 = CARTESIAN_POINT ( 'NONE',  ( 764.0069404352550464, -423.0783235625953580, -359.2566176426627180 ) ) ;
#2189 = CARTESIAN_POINT ( 'NONE',  ( 745.4481719005789273, -267.7255117493287457, -347.5162901302853697 ) ) ;
#2190 = DIRECTION ( 'NONE',  ( -1.000000000000000000, -0.000000000000000000, -0.000000000000000000 ) ) ;
#2191 = LINE ( 'NONE', #16283, #28287 ) ;
#2192 = CARTESIAN_POINT ( 'NONE',  ( 804.6798772138708955, -39.72551174932951312, -334.6312213355107019 ) ) ;
#2193 = CARTESIAN_POINT ( 'NONE',  ( 744.6391490659812007, -230.7363362996981664, 338.7502325331110455 ) ) ;
#2194 = CARTESIAN_POINT ( 'NONE',  ( 748.3538107759620743, -160.7146871989598651, -355.8262568251490165 ) ) ;
#2195 = CARTESIAN_POINT ( 'NONE',  ( 813.1304606946830518, -137.9073299311473875, 352.3570229623690580 ) ) ;
#2196 = CARTESIAN_POINT ( 'NONE',  ( 767.6429770376289525, -393.1800572038737300, -306.8695393053162093 ) ) ;
#2197 = LINE ( 'NONE', #41236, #38683 ) ;
#2198 = CARTESIAN_POINT ( 'NONE',  ( 765.0180583372156207, -264.9982390220561115, 360.0135310231089534 ) ) ;
#2199 = CARTESIAN_POINT ( 'NONE',  ( 802.9823548866075953, -49.09997266333511590, 330.0799878456151077 ) ) ;
#2200 = CARTESIAN_POINT ( 'NONE',  ( 768.0187753319979720, -392.6346026584193396, -318.0580252608186242 ) ) ;
#2201 = CARTESIAN_POINT ( 'NONE',  ( 914.9999999999992042, 99.99999999999984368, 360.0000000000000000 ) ) ;
#2202 = DIRECTION ( 'NONE',  ( 0.000000000000000000, 0.000000000000000000, -1.000000000000000000 ) ) ;
#2203 = CARTESIAN_POINT ( 'NONE',  ( 784.0799538623451781, -83.80559628986920018, 364.6971507214555572 ) ) ;
#2204 = VERTEX_POINT ( 'NONE', #42077 ) ;
#2205 =( REPRESENTATION_RELATIONSHIP ('NONE','NONE', #39835, #28408 ) REPRESENTATION_RELATIONSHIP_WITH_TRANSFORMATION ( #25586 )SHAPE_REPRESENTATION_RELATIONSHIP( ) );
#2206 = CARTESIAN_POINT ( 'NONE',  ( 801.3366627262608972, -224.5328690171415076, -353.0897708529566899 ) ) ;
#2207 = CARTESIAN_POINT ( 'NONE',  ( 778.1981804954714335, -130.2709662947837899, -314.8072714833589885 ) ) ;
#2208 = CARTESIAN_POINT ( 'NONE',  ( 771.2633955100217236, -47.90732993114767169, 363.4237431249939618 ) ) ;
#2209 = CARTESIAN_POINT ( 'NONE',  ( 798.0661480581538854, -242.5328690171414507, -309.5768839229118043 ) ) ;
#2210 = LINE ( 'NONE', #33395, #10574 ) ;
#2211 = CARTESIAN_POINT ( 'NONE',  ( 776.2433038121456548, -396.8965053807772847, 374.8207195650711014 ) ) ;
#2212 = ORIENTED_EDGE ( 'NONE', *, *, #10099, .F. ) ;
#2213 = CARTESIAN_POINT ( 'NONE',  ( 778.1981804954714335, -178.2709662947835625, -314.8072714833589885 ) ) ;
#2214 = CARTESIAN_POINT ( 'NONE',  ( 800.2193346964447755, -378.9982390220555999, 355.1360043628815788 ) ) ;
#2215 = CARTESIAN_POINT ( 'NONE',  ( 792.3570229623688874, -93.18005720387481006, -373.1304606946836202 ) ) ;
#2216 = CARTESIAN_POINT ( 'NONE',  ( 801.9419747391806368, -66.45278447660216159, -351.9812246680014027 ) ) ;
#2217 = ORIENTED_EDGE ( 'NONE', *, *, #15681, .F. ) ;
#2218 = CARTESIAN_POINT ( 'NONE',  ( 798.5707757039680246, -5.463609026971610660, -356.7845633553585003 ) ) ;
#2219 = ORIENTED_EDGE ( 'NONE', *, *, #36874, .F. ) ;
#2220 = CARTESIAN_POINT ( 'NONE',  ( 802.5472867521000353, -340.3726999360615082, -350.8726784830461156 ) ) ;
#2222 = CARTESIAN_POINT ( 'NONE',  ( 790.9844846989617508, -406.3726999360612808, 317.2208543904092721 ) ) ;
#2221 = CARTESIAN_POINT ( 'NONE',  ( 794.9819416627830151, -84.99823902205663728, 319.9864689768909898 ) ) ;
#2225 = CARTESIAN_POINT ( 'NONE',  ( 756.1443688327750579, -309.6237781080502600, 314.3581564841659315 ) ) ;
#2224 = CARTESIAN_POINT ( 'NONE',  ( 879.9999999999992042, 249.9999999999998295, 199.9999999999999716 ) ) ;
#2223 = CARTESIAN_POINT ( 'NONE',  ( 813.1304606946831655, -425.9073299311463643, 352.3570229623691716 ) ) ;
#2226 = CARTESIAN_POINT ( 'NONE',  ( 793.9708237608222134, -310.9181544815160123, -319.2295555964448681 ) ) ;
#2227 = CARTESIAN_POINT ( 'NONE',  ( 791.9812246680005501, -308.6346026584195670, -361.9419747391813189 ) ) ;
#2228 = CARTESIAN_POINT ( 'NONE',  ( 811.3240766477731540, -148.3726999360620198, -355.6651683502462902 ) ) ;
#2229 = CARTESIAN_POINT ( 'NONE',  ( 811.3240766477731540, -4.372699936062523385, 355.6651683502462902 ) ) ;
#2231 = PLANE ( 'NONE',  #41075 ) ;
#2230 = DIRECTION ( 'NONE',  ( 0.7071067811857625340, 0.000000000000000000, 0.7071067811873326114 ) ) ;
#2232 = CARTESIAN_POINT ( 'NONE',  ( 756.7813123517142913, -259.9874144716869182, -329.9779781133712504 ) ) ;
#2233 = CARTESIAN_POINT ( 'NONE',  ( 745.1792804349281596, -110.1908817542440033, -343.7566961878542884 ) ) ;
#2234 = LINE ( 'NONE', #3629, #42598 ) ;
#2235 = CARTESIAN_POINT ( 'NONE',  ( 311.1634899080286232, 229.9999999999999716, -199.9999999999963336 ) ) ;
#2236 = CARTESIAN_POINT ( 'NONE',  ( 804.4086373105744769, -337.6454272087888171, 333.3843516231986541 ) ) ;
#2237 = CARTESIAN_POINT ( 'NONE',  ( 778.2165204200184689, -190.8164208402381234, 364.9363028652563230 ) ) ;
#2238 = ORIENTED_EDGE ( 'NONE', *, *, #32386, .T. ) ;
#2239 = CARTESIAN_POINT ( 'NONE',  ( 745.7194118038753459, -301.6454272087889308, 348.7631598425976449 ) ) ;
#2240 = CARTESIAN_POINT ( 'NONE',  ( 787.5162901302840055, -179.3618753856927128, -305.4481719005793252 ) ) ;
#2241 = DIRECTION ( 'NONE',  ( -1.000000000000000000, -0.000000000000000000, -0.000000000000000000 ) ) ;
#2242 = CARTESIAN_POINT ( 'NONE',  ( 814.8207195650702488, -122.1908817542439749, 336.2433038121456548 ) ) ;
#2243 = CARTESIAN_POINT ( 'NONE',  ( 744.7301800767019131, -316.8164208402377540, -337.4774526936615757 ) ) ;
#2244 = FACE_BOUND ( 'NONE', #18507, .T. ) ;
#2245 = PRODUCT ( 'Fixed Blade Support Base', 'Fixed Blade Support Base', '', ( #30746 ) ) ;
#2246 = CARTESIAN_POINT ( 'NONE',  ( 781.7834795799800531, -154.8164208402382371, 315.0636971347436202 ) ) ;
#2247 = ORIENTED_EDGE ( 'NONE', *, *, #26936, .F. ) ;
#2248 = CARTESIAN_POINT ( 'NONE',  ( 793.5525998758768083, -391.0999726633340288, 372.6845335610516941 ) ) ;
#2249 = CARTESIAN_POINT ( 'NONE',  ( 759.8311093483677041, -358.1692326535047641, -310.9282345327691814 ) ) ;
#2250 = CARTESIAN_POINT ( 'NONE',  ( 814.5518280994195948, -87.72551174932937101, -332.4837098697145734 ) ) ;
#2251 = CARTESIAN_POINT ( 'NONE',  ( 769.0155153010367712, -34.37269993606243901, 362.7791456095907279 ) ) ;
#2252 = CARTESIAN_POINT ( 'NONE',  ( 751.6929314249748586, -390.9982390220557136, -318.8095938919659034 ) ) ;
#2253 = DIRECTION ( 'NONE',  ( 1.000000000000000000, 0.000000000000000000, 0.000000000000000000 ) ) ;
#2254 = CARTESIAN_POINT ( 'NONE',  ( 805.1016975059191054, -438.8965053807771710, 343.0745993439771837 ) ) ;
#2255 = VERTEX_POINT ( 'NONE', #13451 ) ;
#2256 = CARTESIAN_POINT ( 'NONE',  ( 768.8385539511368734, -119.2601417444145397, -306.4236121716840557 ) ) ;
#2257 = CARTESIAN_POINT ( 'NONE',  ( -28.63011601220122415, -857.0166862835568509, -63.94525337997358605 ) ) ;
#2258 = CARTESIAN_POINT ( 'NONE',  ( 771.2368401574024119, -277.4419599262322436, 374.2805881961240857 ) ) ;
#2259 = CARTESIAN_POINT ( 'NONE',  ( 804.4286716492782716, -89.36187538569299704, 345.3141322388244703 ) ) ;
#2260 = ORIENTED_EDGE ( 'NONE', *, *, #28130, .F. ) ;
#2261 = CARTESIAN_POINT ( 'NONE',  ( 803.6646147819161570, -281.9073299311468759, 348.8264449731210561 ) ) ;
#2262 = CARTESIAN_POINT ( 'NONE',  ( 746.0683387631852383, -427.4419599262317888, -331.3260364891676204 ) ) ;
#2263 = DIRECTION ( 'NONE',  ( -1.880165489482579047E-16, -1.000000000000000000, -0.000000000000000000 ) ) ;
#2264 = ORIENTED_EDGE ( 'NONE', *, *, #37278, .T. ) ;
#2265 = ORIENTED_EDGE ( 'NONE', *, *, #28091, .F. ) ;
#2266 = CARTESIAN_POINT ( 'NONE',  ( 781.2370466360911223, -380.7363362996977116, -304.9990715423533629 ) ) ;
#2267 = CARTESIAN_POINT ( 'NONE',  ( 755.0636971347428243, -244.2709662947834204, -341.7834795799807353 ) ) ;
#2269 = CARTESIAN_POINT ( 'NONE',  ( 744.9990715423526808, -210.3510508353233490, 341.2370466360926002 ) ) ;
#2268 = CARTESIAN_POINT ( 'NONE',  ( 758.8095938919644823, -320.0891481129648923, 311.6929314249762797 ) ) ;
#2270 = CARTESIAN_POINT ( 'NONE',  ( 798.5707757039680246, -221.4636090269709428, -356.7845633553585003 ) ) ;
#2271 = CARTESIAN_POINT ( 'NONE',  ( 759.7806653035534055, -222.9982390220561399, -324.8639956371180801 ) ) ;
#2272 = CARTESIAN_POINT ( 'NONE',  ( 781.8018195045267476, -430.2709662947827383, -365.1927285166407273 ) ) ;
#2273 = VERTEX_POINT ( 'NONE', #44865 ) ;
#2274 = CARTESIAN_POINT ( 'NONE',  ( 768.0187753319979720, -200.6346026584199365, 318.0580252608186242 ) ) ;
#2275 = CARTESIAN_POINT ( 'NONE',  ( 765.0180583372156207, -96.99823902205660886, -360.0135310231089534 ) ) ;
#2276 = ORIENTED_EDGE ( 'NONE', *, *, #36789, .T. ) ;
#2277 = CARTESIAN_POINT ( 'NONE',  ( 751.9810565676468741, -362.0891481129648923, 360.9747183278973921 ) ) ;
#2278 = CARTESIAN_POINT ( 'NONE',  ( 781.3877698825695006, 18.31902617013176027, -309.9999999999999432 ) ) ;
#2279 = CARTESIAN_POINT ( 'NONE',  ( 989.9999999999992042, -590.0000000000001137, 360.0000000000000000 ) ) ;
#2280 = CYLINDRICAL_SURFACE ( 'NONE', #12795, 10.00000000000000888 ) ;
#2281 = CARTESIAN_POINT ( 'NONE',  ( 796.1575198192839480, -222.0090635724254184, 359.4546378042384163 ) ) ;
#2282 = CARTESIAN_POINT ( 'NONE',  ( 803.6646147819161570, -89.90732993114750116, 348.8264449731210561 ) ) ;
#2283 = ORIENTED_EDGE ( 'NONE', *, *, #14859, .F. ) ;
#2284 = CARTESIAN_POINT ( 'NONE',  ( 757.7880784355613741, -450.0090635724248500, -312.4576283171834916 ) ) ;
#2285 = CARTESIAN_POINT ( 'NONE',  ( 814.2001403089898304, -41.36187538569314626, -347.4397851343538264 ) ) ;
#2286 = CARTESIAN_POINT ( 'NONE',  ( 759.2295555964440155, -256.1692326535049915, 353.9708237608231229 ) ) ;
#2287 = CARTESIAN_POINT ( 'NONE',  ( 764.8639956371174549, -440.0891481129644944, -319.7806653035542013 ) ) ;
#2288 = CARTESIAN_POINT ( 'NONE',  ( 756.5762568750052424, -51.18005720387493085, -348.7366044899774238 ) ) ;
#2289 = SHAPE_REPRESENTATION ( 'MirrorTreadle Extension Return Springs', ( #26858 ), #27503 ) ;
#2290 = CARTESIAN_POINT ( 'NONE',  ( 777.4774526936600978, -442.2709662947826814, 304.7301800767027657 ) ) ;
#2291 = LINE ( 'NONE', #22859, #8243 ) ;
#2292 = CARTESIAN_POINT ( 'NONE',  ( 804.6971507214547046, -291.2817908451525000, -344.0799538623459739 ) ) ;
#2293 = CARTESIAN_POINT ( 'NONE',  ( 772.5602148656447525, -177.7255117493290868, -305.7998596910095443 ) ) ;
#2294 = CARTESIAN_POINT ( 'NONE',  ( 754.9967657858570647, -73.54369356751118403, 365.0032342141425374 ) ) ;
#2295 = CARTESIAN_POINT ( 'NONE',  ( 800.9747183278959710, -156.9982390220564241, 311.9810565676471583 ) ) ;
#2296 = DIRECTION ( 'NONE',  ( 0.000000000000000000, 0.000000000000000000, -1.000000000000000000 ) ) ;
#2297 = CARTESIAN_POINT ( 'NONE',  ( 779.9999999999992042, -462.9681489794448339, -309.9999999999998863 ) ) ;
#2298 = CARTESIAN_POINT ( 'NONE',  ( 808.7758568127978833, -244.1692326535050768, -320.0363995740631822 ) ) ;
#2299 = CARTESIAN_POINT ( 'NONE',  ( 805.6418435158337843, -413.4636090269704027, 363.8556311672236916 ) ) ;
#2300 = DIRECTION ( 'NONE',  ( 1.000000000000000000, 0.000000000000000000, 0.000000000000000000 ) ) ;
#2301 = CARTESIAN_POINT ( 'NONE',  ( 745.4481719005789273, -411.7255117493282910, 347.5162901302853129 ) ) ;
#2302 = CARTESIAN_POINT ( 'NONE',  ( 745.7998596910086917, -29.36187538569318178, 332.5602148656461168 ) ) ;
#2303 = CARTESIAN_POINT ( 'NONE',  ( 768.0187753319979720, -368.6346026584193964, -318.0580252608186242 ) ) ;
#2304 = CARTESIAN_POINT ( 'NONE',  ( 803.8651313633788504, -5.260141744414903897, 332.4468031744301015 ) ) ;
#2305 = CARTESIAN_POINT ( 'NONE',  ( 757.7880784355613741, -90.00906357242590161, -312.4576283171834916 ) ) ;
#2306 = CARTESIAN_POINT ( 'NONE',  ( 764.0069404352550464, -159.0783235625962391, -359.2566176426627180 ) ) ;
#2307 = CARTESIAN_POINT ( 'NONE',  ( 758.0141637701419768, -159.0783235625962391, 367.2620300519063790 ) ) ;
#2308 = PLANE ( 'NONE',  #27667 ) ;
#2309 = ORIENTED_EDGE ( 'NONE', *, *, #15175, .T. ) ;
#2310 = CARTESIAN_POINT ( 'NONE',  ( 755.3201227861273992, -51.72551174932946338, -345.3687786644892981 ) ) ;
#2311 = CARTESIAN_POINT ( 'NONE',  ( 783.0433043558608688, -168.8965053807780237, -315.1538015810313027 ) ) ;
#2312 = CARTESIAN_POINT ( 'NONE',  ( 792.1044303154645831, -180.4527844766017211, 317.8323909638837677 ) ) ;
#2313 = EDGE_CURVE ( 'NONE', #30501, #26595, #11394, .T. ) ;
#2314 = CARTESIAN_POINT ( 'NONE',  ( 786.2056067578752163, -11.80559628986942577, -374.4686193811670023 ) ) ;
#2315 = CARTESIAN_POINT ( 'NONE',  ( 755.0636971347428243, -292.2709662947831930, 341.7834795799807353 ) ) ;
#2316 =( GEOMETRIC_REPRESENTATION_CONTEXT ( 3 ) GLOBAL_UNCERTAINTY_ASSIGNED_CONTEXT ( ( #45060 ) ) GLOBAL_UNIT_ASSIGNED_CONTEXT ( ( #37692, #10198, #13223 ) ) REPRESENTATION_CONTEXT ( 'NONE', 'WORKASPACE' ) );
#2317 = DIRECTION ( 'NONE',  ( 0.000000000000000000, -0.000000000000000000, 1.000000000000000000 ) ) ;
#2318 = EDGE_LOOP ( 'NONE', ( #31488, #3719, #20337, #11430 ) ) ;
#2319 = CARTESIAN_POINT ( 'NONE',  ( 756.1348686366196716, -17.26014174441486659, 347.5531968255698416 ) ) ;
#2320 = CARTESIAN_POINT ( 'NONE',  ( 745.1792804349281596, -278.1908817542434917, -343.7566961878542884 ) ) ;
#2321 = ORIENTED_EDGE ( 'NONE', *, *, #12855, .F. ) ;
#2322 = CARTESIAN_POINT ( 'NONE',  ( 0.000000000000000000, 0.000000000000000000, 0.000000000000000000 ) ) ;
#2323 = CARTESIAN_POINT ( 'NONE',  ( 792.3570229623691148, -237.1800572038742985, 373.1304606946836770 ) ) ;
#2324 = CARTESIAN_POINT ( 'NONE',  ( 805.2837595273609850, -290.7363362996980527, 340.5290396650784714 ) ) ;
#2325 = CARTESIAN_POINT ( 'NONE',  ( 760.5453621957607311, -405.0783235625954148, 323.8424801807151425 ) ) ;
#2326 = ORIENTED_EDGE ( 'NONE', *, *, #36268, .T. ) ;
#2327 = CARTESIAN_POINT ( 'NONE',  ( 757.4527132478984868, -112.3726999360621761, -329.1273215169538844 ) ) ;
#2328 = CARTESIAN_POINT ( 'NONE',  ( 774.6858677611749044, -129.7255117493292289, -315.5713283507209894 ) ) ;
#2329 = CARTESIAN_POINT ( 'NONE',  ( 803.4237431249931660, -327.1800572038741279, -331.2633955100225194 ) ) ;
#2330 = ORIENTED_EDGE ( 'NONE', *, *, #36798, .F. ) ;
#2331 = CARTESIAN_POINT ( 'NONE',  ( 759.7806653035534055, -438.9982390220553157, -324.8639956371180801 ) ) ;
#2332 = CARTESIAN_POINT ( 'NONE',  ( 761.2382568024794409, -303.6237781080503169, 356.9571628226838129 ) ) ;
#2333 = CARTESIAN_POINT ( 'NONE',  ( 793.4839952031973098, -454.3310370489100478, 372.1249834419284639 ) ) ;
#2334 = DIRECTION ( 'NONE',  ( 1.000000000000000000, -1.880165489482579047E-16, -0.000000000000000000 ) ) ;
#2335 = CARTESIAN_POINT ( 'NONE',  ( 784.1219089521767955, -117.2817908451530684, 315.0488828828318333 ) ) ;
#2336 = CARTESIAN_POINT ( 'NONE',  ( 781.7834795799800531, 13.18357915976123174, 315.0636971347436202 ) ) ;
#2337 = ORIENTED_EDGE ( 'NONE', *, *, #26661, .T. ) ;
#2338 = CARTESIAN_POINT ( 'NONE',  ( 764.1737431748507561, -346.3726999360614514, -371.6461892240376415 ) ) ;
#2339 = CARTESIAN_POINT ( 'NONE',  ( 781.2370466360911223, -188.7363362996983085, 304.9990715423533629 ) ) ;
#2340 = CARTESIAN_POINT ( 'NONE',  ( 762.3223304703356007, -319.5436935675104451, -322.3223304703362828 ) ) ;
#2341 = FILL_AREA_STYLE_COLOUR ( '', #10435 ) ;
#2342 = CARTESIAN_POINT ( 'NONE',  ( 802.9823548866075953, -193.0999726633346256, -330.0799878456151077 ) ) ;
#2343 = CARTESIAN_POINT ( 'NONE',  ( 777.4774526936600978, -58.27096629478398171, 304.7301800767027657 ) ) ;
#2344 = AXIS2_PLACEMENT_3D ( 'NONE', #37289, #19743, #2183 ) ;
#2345 = DIRECTION ( 'NONE',  ( 1.000000000000000000, 0.000000000000000000, 0.000000000000000000 ) ) ;
#2346 = CARTESIAN_POINT ( 'NONE',  ( 808.3070685750232087, -378.9982390220557136, -361.1904061080339829 ) ) ;
#2347 = FACE_OUTER_BOUND ( 'NONE', #400, .T. ) ;
#2348 = EDGE_CURVE ( 'NONE', #15471, #14853, #35138, .T. ) ;
#2349 = CARTESIAN_POINT ( 'NONE',  ( 811.3240766477731540, -316.3726999360615082, 355.6651683502462902 ) ) ;
#2350 = DIRECTION ( 'NONE',  ( -0.000000000000000000, 1.000000000000000000, -0.000000000000000000 ) ) ;
#2351 = CARTESIAN_POINT ( 'NONE',  ( 811.0346526505616112, -302.6346026584196238, 323.0537975583477532 ) ) ;
#2352 = CARTESIAN_POINT ( 'NONE',  ( 796.9462024416508257, -36.45278447660223975, -308.9653473494370246 ) ) ;
#2353 = CARTESIAN_POINT ( 'NONE',  ( 757.8323909638827445, -242.6346026584197659, -352.1044303154654358 ) ) ;
#2354 = ADVANCED_FACE ( 'NONE', ( #17137 ), #31220, .T. ) ;
#2355 = DIRECTION ( 'NONE',  ( 0.000000000000000000, 0.000000000000000000, 1.000000000000000000 ) ) ;
#2356 = CARTESIAN_POINT ( 'NONE',  ( 792.1044303154645831, -348.4527844766012663, 317.8323909638837677 ) ) ;
#2357 = CARTESIAN_POINT ( 'NONE',  ( 793.0897708529556667, -126.5545181178803205, 361.3366627262616362 ) ) ;
#2358 = CARTESIAN_POINT ( 'NONE',  ( 773.3843516231979720, -61.44195992623291147, -364.4086373105754433 ) ) ;
#2359 = CARTESIAN_POINT ( 'NONE',  ( 776.2433038121456548, -60.89650538077837894, 374.8207195650711014 ) ) ;
#2360 = CARTESIAN_POINT ( 'NONE',  ( 803.6646147819162707, -353.9073299311467053, 348.8264449731211130 ) ) ;
#2361 = CARTESIAN_POINT ( 'NONE',  ( 814.5518280994195948, 8.274488250670337663, 332.4837098697145166 ) ) ;
#2362 = CYLINDRICAL_SURFACE ( 'NONE', #32139, 2.749999999999863665 ) ;
#2363 = CARTESIAN_POINT ( 'NONE',  ( 798.0661480581538854, -146.5328690171417350, 309.5768839229118043 ) ) ;
#2364 = CARTESIAN_POINT ( 'NONE',  ( 781.7834795799800531, -442.8164208402372992, 315.0636971347436202 ) ) ;
#2365 = ORIENTED_EDGE ( 'NONE', *, *, #4735, .T. ) ;
#2366 = EDGE_CURVE ( 'NONE', #13298, #42174, #13677, .T. ) ;
#2367 = EDGE_CURVE ( 'NONE', #2677, #39212, #37185, .T. ) ;
#2368 = CARTESIAN_POINT ( 'NONE',  ( 763.2154366446407039, -381.6237781080500326, -321.4292242960311228 ) ) ;
#2370 = CARTESIAN_POINT ( 'NONE',  ( 764.8639956371174549, -176.0891481129654039, 319.7806653035542581 ) ) ;
#2369 = CARTESIAN_POINT ( 'NONE',  ( 765.0180583372156207, -192.9982390220562820, 360.0135310231089534 ) ) ;
#2371 = AXIS2_PLACEMENT_3D ( 'NONE', #8273, #12193, #22338 ) ;
#2372 = CARTESIAN_POINT ( 'NONE',  ( 800.1688906516307043, -370.1692326535045936, -369.0717654672308186 ) ) ;
#2373 = DIRECTION ( 'NONE',  ( 1.000000000000000000, 0.000000000000000000, -0.000000000000000000 ) ) ;
#2374 = ORIENTED_EDGE ( 'NONE', *, *, #14579, .T. ) ;
#2375 = CARTESIAN_POINT ( 'NONE',  ( 762.3223304703356007, -391.5436935675101608, 322.3223304703362828 ) ) ;
#2376 = ORIENTED_EDGE ( 'NONE', *, *, #18681, .F. ) ;
#2377 = CARTESIAN_POINT ( 'NONE',  ( 801.1904061080336987, -212.0891481129652902, -368.3070685750235498 ) ) ;
#2378 = CARTESIAN_POINT ( 'NONE',  ( 808.3070685750232087, -114.9982390220565378, 361.1904061080339829 ) ) ;
#2379 = EDGE_LOOP ( 'NONE', ( #8972, #28124, #19949, #21029, #42065, #14516 ) ) ;
#2380 = CARTESIAN_POINT ( 'NONE',  ( 781.7834795799800531, -202.8164208402380950, -315.0636971347436202 ) ) ;
#2381 = EDGE_LOOP ( 'NONE', ( #23102, #23854, #14000, #2217, #1867, #3901, #27773, #25609, #12738, #13022, #39635, #33451 ) ) ;
#2382 = ADVANCED_FACE ( 'NONE', ( #23813 ), #13228, .F. ) ;
#2383 = CARTESIAN_POINT ( 'NONE',  ( 755.5713283507202505, -341.3618753856922012, -334.6858677611754729 ) ) ;
#2384 = CARTESIAN_POINT ( 'NONE',  ( 762.3223304703356007, 16.45630643248849267, -322.3223304703362828 ) ) ;
#2385 = ADVANCED_FACE ( 'NONE', ( #10426 ), #27305, .T. ) ;
#2386 = CARTESIAN_POINT ( 'NONE',  ( 751.9810565676468741, -242.0891481129652618, 360.9747183278973921 ) ) ;
#2387 = CARTESIAN_POINT ( 'NONE',  ( 803.2186876482843445, -199.9874144716870603, 350.0220218866286928 ) ) ;
#2389 = CARTESIAN_POINT ( 'NONE',  ( 939.9999999999993179, -590.0000000000001137, -209.9999999999999716 ) ) ;
#2388 = CARTESIAN_POINT ( 'NONE',  ( 786.4999999999993179, -512.9681489794448908, -339.9999999999999432 ) ) ;
#2390 = CARTESIAN_POINT ( 'NONE',  ( -200.7583438952258916, 294.6698570112193920, -274.9999999999999432 ) ) ;
#2391 = EDGE_LOOP ( 'NONE', ( #6090, #18144, #8044, #23562 ) ) ;
#2392 = CARTESIAN_POINT ( 'NONE',  ( 757.4527132478984868, -448.3726999360611103, -329.1273215169538844 ) ) ;
#2393 = DIRECTION ( 'NONE',  ( 0.000000000000000000, 0.000000000000000000, 1.000000000000000000 ) ) ;
#2394 = CARTESIAN_POINT ( 'NONE',  ( -769.9999999999992042, 205.0000000000000568, -350.0000000000000000 ) ) ;
#2395 = EDGE_CURVE ( 'NONE', #10343, #38198, #15093, .T. ) ;
#2396 = EDGE_LOOP ( 'NONE', ( #22146, #5273, #24875, #15758, #2484, #37091 ) ) ;
#2397 = CARTESIAN_POINT ( 'NONE',  ( 810.4231160770870019, -240.5545181178798941, -321.9338519418446936 ) ) ;
#2398 = CARTESIAN_POINT ( 'NONE',  ( 766.4474001241216001, -91.09997266333496668, 307.3154664389482491 ) ) ;
#2400 = CARTESIAN_POINT ( 'NONE',  ( 764.8639956371174549, -200.0891481129653187, -319.7806653035542013 ) ) ;
#2399 = DIRECTION ( 'NONE',  ( -1.000000000000000000, 0.000000000000000000, 0.000000000000000000 ) ) ;
#2401 = CARTESIAN_POINT ( 'NONE',  ( 759.2295555964440155, -376.1692326535046504, -353.9708237608231229 ) ) ;
#2402 = CARTESIAN_POINT ( 'NONE',  ( 776.2046728542105711, -212.1908817542436623, -304.8212110874238761 ) ) ;
#2403 = FACE_OUTER_BOUND ( 'NONE', #14861, .T. ) ;
#2404 = CARTESIAN_POINT ( 'NONE',  ( 999.5857864376259840, 249.9999999999998863, 199.9999999999999432 ) ) ;
#2405 = CARTESIAN_POINT ( 'NONE',  ( 761.4292242960306112, -65.46360902697142592, -323.2154366446414429 ) ) ;
#2406 = CARTESIAN_POINT ( 'NONE',  ( 802.5472867521000353, -436.3726999360612240, 350.8726784830461156 ) ) ;
#2407 = VECTOR ( 'NONE', #30135, 1000.000000000000000 ) ;
#2408 = CARTESIAN_POINT ( 'NONE',  ( -66.63011601220125613, -359.5698779088871788, -26.28906389436294688 ) ) ;
#2409 = CARTESIAN_POINT ( 'NONE',  ( 758.6633372737375112, -428.5328690171409107, -326.9102291470432533 ) ) ;
#2410 = CARTESIAN_POINT ( 'NONE',  ( 801.1904061080338124, -260.0891481129650629, -368.3070685750236066 ) ) ;
#2411 = EDGE_CURVE ( 'NONE', #29177, #25389, #27757, .T. ) ;
#2412 = CARTESIAN_POINT ( 'NONE',  ( -728.8365100919714905, 230.0000000000001705, -199.9999999999890861 ) ) ;
#2413 = DIRECTION ( 'NONE',  ( 1.000000000000000000, -0.000000000000000000, -0.000000000000000000 ) ) ;
#2414 = CARTESIAN_POINT ( 'NONE',  ( 764.8639956371174549, -32.08914811296588709, -319.7806653035542013 ) ) ;
#2415 = EDGE_CURVE ( 'NONE', #35075, #33515, #40175, .T. ) ;
#2416 = CARTESIAN_POINT ( 'NONE',  ( 814.4686193811664907, -219.2817908451527558, 346.2056067578752732 ) ) ;
#2417 = CARTESIAN_POINT ( 'NONE',  ( 791.1614460488616487, -179.2601417444143692, -373.5763878283158874 ) ) ;
#2418 = CARTESIAN_POINT ( 'NONE',  ( 805.0032342141412300, -181.5436935675108145, 314.9967657858571783 ) ) ;
#2419 = CARTESIAN_POINT ( 'NONE',  ( 749.2812353651451076, -414.4527844766010389, -323.2262854647983090 ) ) ;
#2420 = LINE ( 'NONE', #16757, #28339 ) ;
#2421 = EDGE_CURVE ( 'NONE', #28819, #1277, #39, .T. ) ;
#2422 = CARTESIAN_POINT ( 'NONE',  ( 758.0580252608178853, -270.4527844766014937, 328.0187753319985404 ) ) ;
#2423 = CARTESIAN_POINT ( 'NONE',  ( 755.8894580844503253, -63.82724539060779279, 332.3691319403863531 ) ) ;
#2424 = CARTESIAN_POINT ( 'NONE',  ( 756.5762568750052424, -411.1800572038738437, -348.7366044899774238 ) ) ;
#2425 = FACE_OUTER_BOUND ( 'NONE', #15070, .T. ) ;
#2426 = CARTESIAN_POINT ( 'NONE',  ( -26.63011601220122060, -544.8427095258973623, -369.9999999999999432 ) ) ;
#2428 = CARTESIAN_POINT ( 'NONE',  ( 778.2165204200184689, -334.8164208402376403, 364.9363028652563230 ) ) ;
#2427 = CARTESIAN_POINT ( 'NONE',  ( 766.7756240680305382, -86.53286901714194812, 361.5560724626415663 ) ) ;
#2429 = ORIENTED_EDGE ( 'NONE', *, *, #24599, .T. ) ;
#2430 = EDGE_CURVE ( 'NONE', #24420, #41138, #3963, .T. ) ;
#2431 = CARTESIAN_POINT ( 'NONE',  ( 775.9200461376533440, -239.8055962898687028, -315.3028492785443291 ) ) ;
#2432 = CARTESIAN_POINT ( 'NONE',  ( 791.9812246680005501, -44.63460265842040542, 361.9419747391813189 ) ) ;
#2433 = CARTESIAN_POINT ( 'NONE',  ( 791.1614460488616487, -251.2601417444141134, -373.5763878283158874 ) ) ;
#2434 = CARTESIAN_POINT ( 'NONE',  ( 799.9999999999993179, 205.0000000000000568, -319.9999999999999432 ) ) ;
#2435 = CARTESIAN_POINT ( 'NONE',  ( 768.8385539511368734, -383.2601417444137155, 306.4236121716840557 ) ) ;
#2436 = ORIENTED_EDGE ( 'NONE', *, *, #569, .F. ) ;
#2437 = CARTESIAN_POINT ( 'NONE',  ( 778.1981804954714335, -274.2709662947833067, 314.8072714833589885 ) ) ;
#2438 = CARTESIAN_POINT ( 'NONE',  ( 793.9861285913068514, -442.9180389616178672, 372.1637643035757606 ) ) ;
#2439 = CARTESIAN_POINT ( 'NONE',  ( 785.3141322388236176, -189.7255117493290300, -364.4286716492789537 ) ) ;
#2440 = CARTESIAN_POINT ( 'NONE',  ( 788.8264449731200330, -357.1800572038739006, 363.6646147819171233 ) ) ;
#2441 = CARTESIAN_POINT ( 'NONE',  ( 763.2262854647970016, -128.6346026584201354, -309.2812353651462445 ) ) ;
#2442 = CIRCLE ( 'NONE', #9836, 9.999999999999980460 ) ;
#2443 = CARTESIAN_POINT ( 'NONE',  ( 774.6312213355098493, -95.36187538569296862, -364.6798772138717482 ) ) ;
#2444 = ORIENTED_EDGE ( 'NONE', *, *, #21048, .F. ) ;
#2445 = CARTESIAN_POINT ( 'NONE',  ( 772.4468031744293057, -33.82724539060788516, -363.8651313633793620 ) ) ;
#2446 = AXIS2_PLACEMENT_3D ( 'NONE', #7933, #30274, #1868 ) ;
#2447 = CARTESIAN_POINT ( 'NONE',  ( 758.4439275373578084, -372.5545181178796383, -353.2243759319684386 ) ) ;
#2449 = CARTESIAN_POINT ( 'NONE',  ( 769.0155153010367712, -418.3726999360612808, 362.7791456095907279 ) ) ;
#2448 = CARTESIAN_POINT ( 'NONE',  ( 765.0180583372156207, -96.99823902205660886, 360.0135310231089534 ) ) ;
#2450 = CARTESIAN_POINT ( 'NONE',  ( 755.0488828828309806, -89.80559628986918597, 344.1219089521771934 ) ) ;
#2453 = CARTESIAN_POINT ( 'NONE',  ( 805.9055244015594326, -363.6237781080502032, 315.8990559732753240 ) ) ;
#2452 = CYLINDRICAL_SURFACE ( 'NONE', #33609, 2.749999999999835687 ) ;
#2451 = CARTESIAN_POINT ( 'NONE',  ( 784.4999999999993179, -544.8427095258973623, -369.9999999999999432 ) ) ;
#2454 = CARTESIAN_POINT ( 'NONE',  ( 775.8780910478218402, -369.2817908451523294, -364.9511171171680530 ) ) ;
#2455 = CARTESIAN_POINT ( 'NONE',  ( 791.9812246680005501, -332.6346026584195101, -361.9419747391813189 ) ) ;
#2456 = CARTESIAN_POINT ( 'NONE',  ( 797.8822607201568644, -150.5545181178802352, -370.1134526219340160 ) ) ;
#2457 = CARTESIAN_POINT ( 'NONE',  ( 804.7487373415286811, -451.5436935675099903, 364.7487373415288516 ) ) ;
#2458 = CIRCLE ( 'NONE', #980, 2.749999999999919176 ) ;
#2460 = CARTESIAN_POINT ( 'NONE',  ( 773.4999999999993179, -513.1383975375929367, -369.9999999999999432 ) ) ;
#2459 = CARTESIAN_POINT ( 'NONE',  ( -598.8365100919716042, 256.5000000000001705, -193.8809999999899674 ) ) ;
#2461 = CARTESIAN_POINT ( 'NONE',  ( 763.2154366446407039, -261.6237781080504305, -321.4292242960311228 ) ) ;
#2462 = CARTESIAN_POINT ( 'NONE',  ( 791.0478386215596629, -117.8272453906076151, -306.7653713866226326 ) ) ;
#2463 = LINE ( 'NONE', #29964, #24876 ) ;
#2464 = CARTESIAN_POINT ( 'NONE',  ( 571.1634899080285095, 259.9999999999999432, -197.2499999999982947 ) ) ;
#2465 = CARTESIAN_POINT ( 'NONE',  ( 796.1575198192839480, -318.0090635724251911, 359.4546378042384163 ) ) ;
#2466 = ORIENTED_EDGE ( 'NONE', *, *, #29751, .T. ) ;
#2467 = CARTESIAN_POINT ( 'NONE',  ( 804.1009440267234822, -287.4636090269708575, 314.0944755984392600 ) ) ;
#2468 = CARTESIAN_POINT ( 'NONE',  ( 745.0891759886404770, -172.2709662947836478, -342.4968714119734159 ) ) ;
#2469 = CYLINDRICAL_SURFACE ( 'NONE', #21640, 2.749999999999835687 ) ;
#2470 = CARTESIAN_POINT ( 'NONE',  ( 795.8262568251477660, -94.37269993606224716, 308.3538107759623585 ) ) ;
#2471 = CARTESIAN_POINT ( 'NONE',  ( 745.0891759886404770, -316.2709662947832499, -342.4968714119734159 ) ) ;
#2472 = DIRECTION ( 'NONE',  ( -1.000000000000000000, -0.000000000000000000, -0.000000000000000000 ) ) ;
#2473 = LINE ( 'NONE', #38499, #1348 ) ;
#2474 = CARTESIAN_POINT ( 'NONE',  ( 795.1360043628807261, -140.0891481129654892, 360.2193346964456282 ) ) ;
#2475 = AXIS2_PLACEMENT_3D ( 'NONE', #835, #35477, #7779 ) ;
#2476 = ORIENTED_EDGE ( 'NONE', *, *, #21855, .F. ) ;
#2477 = CARTESIAN_POINT ( 'NONE',  ( 762.1177392798416577, -426.5545181178794678, 309.8865473780659272 ) ) ;
#2478 = CARTESIAN_POINT ( 'NONE',  ( 745.1769319972822814, -377.8055962898682765, -346.2694204179732083 ) ) ;
#2479 = CARTESIAN_POINT ( 'NONE',  ( 814.5518280994195948, -111.7255117493293000, -332.4837098697145734 ) ) ;
#2480 = CARTESIAN_POINT ( 'NONE',  ( 772.4468031744293057, -57.82724539060780700, 363.8651313633793620 ) ) ;
#2481 = CARTESIAN_POINT ( 'NONE',  ( 751.9810565676468741, -386.0891481129647786, -360.9747183278973921 ) ) ;
#2482 = FACE_OUTER_BOUND ( 'NONE', #43857, .T. ) ;
#2483 = CARTESIAN_POINT ( 'NONE',  ( 778.7502325331095108, 23.64894916467591912, 304.6391490659818828 ) ) ;
#2484 = ORIENTED_EDGE ( 'NONE', *, *, #4345, .T. ) ;
#2485 = CARTESIAN_POINT ( 'NONE',  ( 778.7502325331095108, -144.3510508353235764, -304.6391490659818828 ) ) ;
#2486 = DIRECTION ( 'NONE',  ( 0.000000000000000000, 0.000000000000000000, 1.000000000000000000 ) ) ;
#2487 = CARTESIAN_POINT ( 'NONE',  ( 801.9858362298568863, -291.0783235625957559, 312.7379699480935642 ) ) ;
#2488 = CARTESIAN_POINT ( 'NONE',  ( 795.1360043628808398, -92.08914811296570235, 360.2193346964456282 ) ) ;
#2489 = ORIENTED_EDGE ( 'NONE', *, *, #9146, .F. ) ;
#2490 = AXIS2_PLACEMENT_3D ( 'NONE', #11634, #39134, #42812 ) ;
#2491 = CARTESIAN_POINT ( 'NONE',  ( 800.7704444035546203, -4.169232653505813069, -326.0291762391768771 ) ) ;
#2492 = CARTESIAN_POINT ( 'NONE',  ( 800.2193346964447755, -258.9982390220561115, 355.1360043628815788 ) ) ;
#2493 = CARTESIAN_POINT ( 'NONE',  ( 814.2001403089898304, 6.638124614306706306, -347.4397851343538264 ) ) ;
#2494 = LINE ( 'NONE', #37839, #35001 ) ;
#2495 = VERTEX_POINT ( 'NONE', #18057 ) ;
#2496 = ORIENTED_EDGE ( 'NONE', *, *, #15984, .F. ) ;
#2497 = CARTESIAN_POINT ( 'NONE',  ( 797.8594530101008786, -181.5436935675108145, -322.1405469898980982 ) ) ;
#2498 = CARTESIAN_POINT ( 'NONE',  ( 745.1792804349281596, -422.1908817542430370, -343.7566961878542884 ) ) ;
#2500 = CARTESIAN_POINT ( 'NONE',  ( 805.9055244015594326, -267.6237781080504305, 315.8990559732753240 ) ) ;
#2499 = CARTESIAN_POINT ( 'NONE',  ( 763.0537975583476964, -336.4527844766012663, 371.0346526505628617 ) ) ;
#2501 = CARTESIAN_POINT ( 'NONE',  ( 766.9102291470427417, -234.5545181178799794, -318.6633372737382501 ) ) ;
#2502 = CARTESIAN_POINT ( 'NONE',  ( 755.3201227861273992, -219.7255117493289447, -345.3687786644892981 ) ) ;
#2503 = AXIS2_PLACEMENT_3D ( 'NONE', #20702, #6847, #3401 ) ;
#2504 = CARTESIAN_POINT ( 'NONE',  ( 754.8072714833583632, -412.8164208402373561, -338.1981804954721156 ) ) ;
#2505 = AXIS2_PLACEMENT_3D ( 'NONE', #7274, #13509, #10484 ) ;
#2506 = CARTESIAN_POINT ( 'NONE',  ( 756.3353852180819104, -221.9073299311470464, 331.1735550268788302 ) ) ;
#2507 = ORIENTED_EDGE ( 'NONE', *, *, #20142, .T. ) ;
#2508 = CARTESIAN_POINT ( 'NONE',  ( 755.2512626584698410, -343.5436935675103314, 315.2512626584710915 ) ) ;
#2509 = LINE ( 'NONE', #26322, #33659 ) ;
#2510 = CARTESIAN_POINT ( 'NONE',  ( 802.2119215644370342, -6.009063572426154742, -367.5423716828165084 ) ) ;
#2511 = CARTESIAN_POINT ( 'NONE',  ( 792.8389451398237497, 16.45630643248849978, 314.6345231965543121 ) ) ;
#2512 = CARTESIAN_POINT ( 'NONE',  ( 799.9999999999993179, 205.0000000000000568, -255.0000000000000000 ) ) ;
#2513 = CARTESIAN_POINT ( 'NONE',  ( 799.2566176426618085, -240.0090635724253900, 324.0069404352559559 ) ) ;
#2514 = CARTESIAN_POINT ( 'NONE',  ( 759.7806653035534055, -78.99823902205662307, 324.8639956371180801 ) ) ;
#2515 = ORIENTED_EDGE ( 'NONE', *, *, #33217, .F. ) ;
#2516 = CARTESIAN_POINT ( 'NONE',  ( 810.4231160770870019, -432.5545181178793541, -321.9338519418446936 ) ) ;
#2517 = CARTESIAN_POINT ( 'NONE',  ( 767.7687537140311633, -71.90732993114760063, -372.7932403749916830 ) ) ;
#2518 = CARTESIAN_POINT ( 'NONE',  ( 770.0799878456142551, -253.9874144716868329, 362.9823548866085616 ) ) ;
#2519 = CARTESIAN_POINT ( 'NONE',  ( 803.4237431249931660, -423.1800572038737300, -331.2633955100225194 ) ) ;
#2520 = CARTESIAN_POINT ( 'NONE',  ( 803.6646147819162707, -41.90732993114767879, -348.8264449731211130 ) ) ;
#2521 = VECTOR ( 'NONE', #28121, 1000.000000000000000 ) ;
#2522 = CARTESIAN_POINT ( 'NONE',  ( 781.2370466360911223, -20.73633629969883430, 304.9990715423533629 ) ) ;
#2523 = CARTESIAN_POINT ( 'NONE',  ( -858.8365100919713768, 260.0000000000002274, -202.7499999999880345 ) ) ;
#2524 = CARTESIAN_POINT ( 'NONE',  ( 758.4439275373578084, -276.5545181178798657, -353.2243759319684386 ) ) ;
#2525 = CARTESIAN_POINT ( 'NONE',  ( 810.7187646348534145, -210.4527844766016926, -356.7737145352016341 ) ) ;
#2526 = AXIS2_PLACEMENT_3D ( 'NONE', #30837, #37766, #6115 ) ;
#2527 = CARTESIAN_POINT ( 'NONE',  ( 777.4774526936600978, -82.27096629478388934, 304.7301800767027657 ) ) ;
#2528 = CARTESIAN_POINT ( 'NONE',  ( 813.1304606946830518, -137.9073299311473875, 352.3570229623690580 ) ) ;
#2529 = FACE_OUTER_BOUND ( 'NONE', #15063, .T. ) ;
#2530 = LINE ( 'NONE', #23760, #29132 ) ;
#2531 = CARTESIAN_POINT ( 'NONE',  ( 744.9990715423526808, -234.3510508353232638, -341.2370466360926002 ) ) ;
#2532 = CARTESIAN_POINT ( 'NONE',  ( 776.2046728542105711, -404.1908817542431507, 304.8212110874238761 ) ) ;
#2533 = CARTESIAN_POINT ( 'NONE',  ( 814.5518280994195948, -279.7255117493288026, -332.4837098697145734 ) ) ;
#2534 = CARTESIAN_POINT ( 'NONE',  ( 571.1634899080285095, 256.4999999999999432, -199.9999999999981526 ) ) ;
#2535 = CARTESIAN_POINT ( 'NONE',  ( 792.3570229623688874, -381.1800572038737869, 373.1304606946836202 ) ) ;
#2536 = CARTESIAN_POINT ( 'NONE',  ( 800.9747183278959710, -12.99823902205686821, 311.9810565676471583 ) ) ;
#2537 = CARTESIAN_POINT ( 'NONE',  ( 788.7366044899766848, -347.9073299311467053, -316.5762568750059813 ) ) ;
#2538 = VECTOR ( 'NONE', #9306, 1000.000000000000114 ) ;
#2539 = CARTESIAN_POINT ( 'NONE',  ( 795.9930595647434757, -27.07832356259665474, 320.7433823573372820 ) ) ;
#2540 = AXIS2_PLACEMENT_3D ( 'NONE', #20368, #24281, #24744 ) ;
#2541 = CARTESIAN_POINT ( 'NONE',  ( 788.7631598425961101, -49.44195992623295410, -305.7194118038759143 ) ) ;
#2542 = CARTESIAN_POINT ( 'NONE',  ( 755.8398074228967971, -139.4419599262326699, -333.4516893846970333 ) ) ;
#2543 = CARTESIAN_POINT ( 'NONE',  ( 805.9055244015594326, -171.6237781080507432, 315.8990559732753240 ) ) ;
#2544 = CARTESIAN_POINT ( 'NONE',  ( 804.4286716492782716, 6.638124614306706306, 345.3141322388244703 ) ) ;
#2545 = EDGE_LOOP ( 'NONE', ( #19262, #7741, #30157, #11975 ) ) ;
#2546 = CARTESIAN_POINT ( 'NONE',  ( 795.1360043628807261, -68.08914811296575920, -360.2193346964456282 ) ) ;
#2547 = CARTESIAN_POINT ( 'NONE',  ( 756.7813123517142913, -163.9874144716871456, -329.9779781133712504 ) ) ;
#2548 = CARTESIAN_POINT ( 'NONE',  ( 804.4286716492782716, -161.3618753856927697, 345.3141322388244703 ) ) ;
#2549 = CARTESIAN_POINT ( 'NONE',  ( 791.1614460488616487, -11.26014174441488258, -373.5763878283158874 ) ) ;
#2550 = CARTESIAN_POINT ( 'NONE',  ( 802.1676090361155502, -302.6346026584195670, 327.8955696845344505 ) ) ;
#2551 = PLANE ( 'NONE',  #31550 ) ;
#2552 = ORIENTED_EDGE ( 'NONE', *, *, #44509, .T. ) ;
#2553 = CARTESIAN_POINT ( 'NONE',  ( 804.1601925771018387, -7.441959926233078448, 346.5483106153029098 ) ) ;
#2554 = CARTESIAN_POINT ( 'NONE',  ( 773.7305795820266212, -273.2817908451526137, -374.8230680027170365 ) ) ;
#2555 = CIRCLE ( 'NONE', #20984, 30.00000000000008171 ) ;
#2556 = DIRECTION ( 'NONE',  ( 0.000000000000000000, 0.000000000000000000, -1.000000000000000000 ) ) ;
#2557 = AXIS2_PLACEMENT_3D ( 'NONE', #30153, #39499, #12154 ) ;
#2558 = CARTESIAN_POINT ( 'NONE',  ( 772.5602148656447525, -225.7255117493289163, 305.7998596910095443 ) ) ;
#2559 = CARTESIAN_POINT ( 'NONE',  ( 755.5913626894240451, -349.6454272087887603, 346.6156483768012890 ) ) ;
#2560 = CARTESIAN_POINT ( 'NONE',  ( 755.8398074228967971, -427.4419599262317888, 333.4516893846970333 ) ) ;
#2561 = ORIENTED_EDGE ( 'NONE', *, *, #11429, .F. ) ;
#2562 = CARTESIAN_POINT ( 'NONE',  ( 769.0155153010367712, -130.3726999360621619, -362.7791456095907279 ) ) ;
#2563 = CARTESIAN_POINT ( 'NONE',  ( 774.6312213355099630, -119.3618753856928691, -364.6798772138717482 ) ) ;
#2564 = CARTESIAN_POINT ( 'NONE',  ( 756.5762568750052424, -315.1800572038740711, -348.7366044899774238 ) ) ;
#2565 = VERTEX_POINT ( 'NONE', #39304 ) ;
#2566 = CARTESIAN_POINT ( 'NONE',  ( 785.3687786644884454, -443.3618753856917465, -315.3201227861279676 ) ) ;
#2567 = CARTESIAN_POINT ( 'NONE',  ( 755.0488828828309806, -305.8055962898684470, 344.1219089521771934 ) ) ;
#2568 = CARTESIAN_POINT ( 'NONE',  ( 793.1217772804590140, -457.0129860853185733, 370.3581812299415787 ) ) ;
#2569 = CARTESIAN_POINT ( 'NONE',  ( 794.9999999999993179, 240.0000000000000853, -275.0000000000000000 ) ) ;
#2570 = AXIS2_PLACEMENT_3D ( 'NONE', #24286, #41626, #38393 ) ;
#2571 = CARTESIAN_POINT ( 'NONE',  ( 763.0428371773158460, -107.4636090269713122, 358.7617431975195359 ) ) ;
#2572 = CARTESIAN_POINT ( 'NONE',  ( 804.6798772138708955, 8.274488250670337663, 334.6312213355107019 ) ) ;
#2573 = EDGE_LOOP ( 'NONE', ( #31065, #5375, #41524, #11084 ) ) ;
#2574 = CARTESIAN_POINT ( 'NONE',  ( 754.3581564841646241, -353.4636090269705733, -316.1443688327762516 ) ) ;
#2575 = COLOUR_RGB ( '',0.7921568627450980005, 0.8196078431372548767, 0.9333333333333333481 ) ;
#2576 = EDGE_CURVE ( 'NONE', #42212, #45366, #43443, .T. ) ;
#2577 = CARTESIAN_POINT ( 'NONE',  ( 814.2805881961230625, -217.6454272087891582, 331.2368401574024119 ) ) ;
#2578 = CIRCLE ( 'NONE', #34293, 2.749999999999842792 ) ;
#2579 = CARTESIAN_POINT ( 'NONE',  ( 756.3353852180819104, -317.9073299311468190, -331.1735550268788302 ) ) ;
#2580 = CARTESIAN_POINT ( 'NONE',  ( 784.9999999999992042, 205.0000000000000568, -255.0000000000000000 ) ) ;
#2581 = CARTESIAN_POINT ( 'NONE',  ( 775.8780910478218402, -177.2817908451528695, -364.9511171171680530 ) ) ;
#2582 = EDGE_CURVE ( 'NONE', #39622, #45702, #32793, .T. ) ;
#2583 = CARTESIAN_POINT ( 'NONE',  ( 745.7998596910086917, -29.36187538569318178, 332.5602148656461168 ) ) ;
#2584 = LINE ( 'NONE', #16687, #20282 ) ;
#2586 = VECTOR ( 'NONE', #42191, 1000.000000000000000 ) ;
#2585 = CARTESIAN_POINT ( 'NONE',  ( 805.0032342141413437, -373.5436935675102177, -314.9967657858572352 ) ) ;
#2587 = CARTESIAN_POINT ( 'NONE',  ( 1007.605605532488426, -295.7697417039441916, 122.5118383533586837 ) ) ;
#2588 = VECTOR ( 'NONE', #8913, 1000.000000000000000 ) ;
#2589 = CARTESIAN_POINT ( 'NONE',  ( 812.3518521366052028, -337.0999726633342561, 326.5853460496235243 ) ) ;
#2590 = DIRECTION ( 'NONE',  ( 0.000000000000000000, 0.000000000000000000, -1.000000000000000000 ) ) ;
#2591 = CARTESIAN_POINT ( 'NONE',  ( 808.3070685750230950, -282.9982390220558841, 361.1904061080339261 ) ) ;
#2592 = CARTESIAN_POINT ( 'NONE',  ( 748.9653473494363425, -2.634602658420536869, -356.9462024416521331 ) ) ;
#2593 = CARTESIAN_POINT ( 'NONE',  ( 794.9819416627830151, -252.9982390220560831, -319.9864689768909898 ) ) ;
#2594 = VECTOR ( 'NONE', #24062, 1000.000000000000000 ) ;
#2595 = CARTESIAN_POINT ( 'NONE',  ( -773.4999999999993179, -563.3203001761230553, -342.3463313526983143 ) ) ;
#2596 = CARTESIAN_POINT ( 'NONE',  ( 792.1044303154645831, -396.4527844766010389, 317.8323909638837677 ) ) ;
#2597 = CARTESIAN_POINT ( 'NONE',  ( 766.9102291470427417, -162.5545181178802352, 318.6633372737382501 ) ) ;
#2598 = CARTESIAN_POINT ( 'NONE',  ( 786.6156483768007774, -49.44195992623295410, -315.5913626894246136 ) ) ;
#2599 = CARTESIAN_POINT ( 'NONE',  ( 814.8230680027162407, -77.80559628986920018, 333.7305795820267917 ) ) ;
#2600 = CARTESIAN_POINT ( 'NONE',  ( 759.9864689768902508, -362.0891481129648923, 354.9819416627836404 ) ) ;
#2601 = FACE_OUTER_BOUND ( 'NONE', #38457, .T. ) ;
#2602 = SURFACE_SIDE_STYLE ('',( #27996 ) ) ;
#2603 = CARTESIAN_POINT ( 'NONE',  ( 764.8639956371174549, -416.0891481129645513, 319.7806653035542013 ) ) ;
#2604 = ORIENTED_EDGE ( 'NONE', *, *, #1301, .F. ) ;
#2605 = CARTESIAN_POINT ( 'NONE',  ( 762.3223304703356007, -55.54369356751127640, -322.3223304703362828 ) ) ;
#2606 = CARTESIAN_POINT ( 'NONE',  ( 794.1144889064781864, -370.1692326535045936, -360.9840315886528401 ) ) ;
#2608 = CARTESIAN_POINT ( 'NONE',  ( 785.3141322388236176, -189.7255117493290300, 364.4286716492789537 ) ) ;
#2607 = CARTESIAN_POINT ( 'NONE',  ( 791.9812246680005501, -188.6346026584199365, 361.9419747391813189 ) ) ;
#2609 = CIRCLE ( 'NONE', #10002, 9.999999999999982236 ) ;
#2610 = CARTESIAN_POINT ( 'NONE',  ( 758.0141637701419768, -375.0783235625955285, -367.2620300519063790 ) ) ;
#2611 = CARTESIAN_POINT ( 'NONE',  ( 927.9999999999992042, 219.9999999999998863, -350.0000000000000000 ) ) ;
#2612 = ORIENTED_EDGE ( 'NONE', *, *, #26636, .F. ) ;
#2613 = CARTESIAN_POINT ( 'NONE',  ( 804.4286716492782716, -377.3618753856920875, 345.3141322388244703 ) ) ;
#2614 = VECTOR ( 'NONE', #34560, 1000.000000000000000 ) ;
#2615 = ORIENTED_EDGE ( 'NONE', *, *, #30089, .T. ) ;
#2616 = DIRECTION ( 'NONE',  ( 0.000000000000000000, 0.000000000000000000, 1.000000000000000000 ) ) ;
#2617 = CARTESIAN_POINT ( 'NONE',  ( 787.5162901302840055, -203.3618753856925991, -305.4481719005792684 ) ) ;
#2618 = CARTESIAN_POINT ( 'NONE',  ( 787.5162901302840055, -107.3618753856928976, 305.4481719005793252 ) ) ;
#2619 = VERTEX_POINT ( 'NONE', #14363 ) ;
#2620 = CARTESIAN_POINT ( 'NONE',  ( 756.5762568750052424, -219.1800572038744122, -348.7366044899774238 ) ) ;
#2621 = EDGE_LOOP ( 'NONE', ( #6438, #44076, #22778, #12903 ) ) ;
#2622 = CARTESIAN_POINT ( 'NONE',  ( 765.0180583372156207, -312.9982390220559409, -360.0135310231089534 ) ) ;
#2623 = CARTESIAN_POINT ( 'NONE',  ( 804.4086373105744769, -457.6454272087884760, -333.3843516231986541 ) ) ;
#2624 = PRESENTATION_LAYER_ASSIGNMENT (  '', '', ( #1887 ) ) ;
#2625 = CARTESIAN_POINT ( 'NONE',  ( 756.1348686366196716, -209.2601417444142839, 347.5531968255698416 ) ) ;
#2627 = DIRECTION ( 'NONE',  ( -1.000000000000000000, -0.000000000000000000, -0.000000000000000000 ) ) ;
#2626 = CARTESIAN_POINT ( 'NONE',  ( 809.8718804791541288, -453.2309196406925480, 337.2303869152726179 ) ) ;
#2628 = DIRECTION ( 'NONE',  ( -1.000000000000000000, -0.000000000000000000, 0.000000000000000000 ) ) ;
#2629 = AXIS2_PLACEMENT_3D ( 'NONE', #21604, #35686, #25291 ) ;
#2630 = ADVANCED_FACE ( 'NONE', ( #36510 ), #4432, .T. ) ;
#2631 = PRODUCT ( 'MirrorSlot', 'MirrorSlot', '', ( #40907 ) ) ;
#2632 = ORIENTED_EDGE ( 'NONE', *, *, #41103, .T. ) ;
#2633 = CARTESIAN_POINT ( 'NONE',  ( 755.8894580844503253, -447.8272453906067199, -332.3691319403863531 ) ) ;
#2634 = LINE ( 'NONE', #19962, #23991 ) ;
#2635 = DIRECTION ( 'NONE',  ( -1.000000000000000000, -0.000000000000000000, 0.000000000000000000 ) ) ;
#2636 = EDGE_LOOP ( 'NONE', ( #16416, #40742 ) ) ;
#2637 = CARTESIAN_POINT ( 'NONE',  ( 745.7194118038753459, -229.6454272087890729, -348.7631598425976449 ) ) ;
#2638 = CARTESIAN_POINT ( 'NONE',  ( 786.2694204179717872, -117.2817908451530684, 305.1769319972829067 ) ) ;
#2640 = CARTESIAN_POINT ( 'NONE',  ( 797.8594530101008786, -205.5436935675108430, -322.1405469898980982 ) ) ;
#2639 = CARTESIAN_POINT ( 'NONE',  ( 939.9999999999993179, -600.0000000000001137, -360.0000000000000000 ) ) ;
#2641 = CARTESIAN_POINT ( 'NONE',  ( 757.2208543904082489, -376.7146871989592682, -350.9844846989624330 ) ) ;
#2642 = CARTESIAN_POINT ( 'NONE',  ( 752.7379699480933368, -252.0090635724254184, -361.9858362298580232 ) ) ;
#2643 = CARTESIAN_POINT ( 'NONE',  ( 998.9999999999992042, 249.9999999999998863, 199.9999999999999716 ) ) ;
#2644 = LINE ( 'NONE', #5407, #3910 ) ;
#2645 = CARTESIAN_POINT ( 'NONE',  ( 796.9571628226829034, -71.46360902697141171, -321.2382568024804641 ) ) ;
#2646 = EDGE_CURVE ( 'NONE', #19936, #44204, #25430, .T. ) ;
#2647 = CARTESIAN_POINT ( 'NONE',  ( 790.0220218866281812, -439.0999726633339719, 363.2186876482849129 ) ) ;
#2648 = CARTESIAN_POINT ( 'NONE',  ( 779.9999999999992042, 166.4563064324884465, 339.9999999999999432 ) ) ;
#2649 = CARTESIAN_POINT ( 'NONE',  ( 777.4774526936600978, -274.2709662947832499, -304.7301800767028226 ) ) ;
#2650 = CARTESIAN_POINT ( 'NONE',  ( -338.8365100919713200, 240.0000000000001137, -199.9999999999917861 ) ) ;
#2651 = CARTESIAN_POINT ( 'NONE',  ( -773.4999999999993179, -513.1383975375929367, -349.9999999999999432 ) ) ;
#2652 = CARTESIAN_POINT ( 'NONE',  ( 804.9363028652555840, -40.27096629478405987, -338.2165204200192079 ) ) ;
#2653 = VECTOR ( 'NONE', #14168, 1000.000000000000000 ) ;
#2654 = CARTESIAN_POINT ( 'NONE',  ( 793.5525998758768083, -223.0999726633346256, 372.6845335610516941 ) ) ;
#2655 = CARTESIAN_POINT ( 'NONE',  ( 803.8556311672234642, -177.6237781080507148, -365.6418435158340117 ) ) ;
#2656 = CARTESIAN_POINT ( 'NONE',  ( 745.4481719005789273, -195.7255117493289731, 347.5162901302853129 ) ) ;
#2657 = VECTOR ( 'NONE', #35418, 1000.000000000000000 ) ;
#2658 = CARTESIAN_POINT ( 'NONE',  ( 811.0346526505616112, -422.6346026584192259, -323.0537975583477532 ) ) ;
#2659 = CYLINDRICAL_SURFACE ( 'NONE', #27621, 1.000000000000000888 ) ;
#2660 = CARTESIAN_POINT ( 'NONE',  ( 788.7366044899766848, -275.9073299311469896, 316.5762568750059813 ) ) ;
#2661 = CARTESIAN_POINT ( 'NONE',  ( 793.9708237608222134, -70.91815448151683654, 319.2295555964448681 ) ) ;
#2662 = ADVANCED_FACE ( 'NONE', ( #28443 ), #42759, .T. ) ;
#2663 = CARTESIAN_POINT ( 'NONE',  ( 797.6776695296629214, -427.5436935675101040, -357.6776695296636603 ) ) ;
#2664 = FACE_OUTER_BOUND ( 'NONE', #17522, .T. ) ;
#2666 = ADVANCED_FACE ( 'NONE', ( #14610 ), #43216, .F. ) ;
#2665 = DIRECTION ( 'NONE',  ( 0.000000000000000000, -1.000000000000000000, 0.000000000000000000 ) ) ;
#2668 = CARTESIAN_POINT ( 'NONE',  ( 759.9864689768902508, -338.0891481129649492, 354.9819416627836404 ) ) ;
#2667 = CARTESIAN_POINT ( 'NONE',  ( 798.7617431975189675, -99.62377810805098477, 323.0428371773161871 ) ) ;
#2669 = ORIENTED_EDGE ( 'NONE', *, *, #27519, .F. ) ;
#2670 = VECTOR ( 'NONE', #22384, 1000.000000000000114 ) ;
#2671 = CARTESIAN_POINT ( 'NONE',  ( 799.4546378042377910, -249.0783235625959549, -356.1575198192848006 ) ) ;
#2672 = CARTESIAN_POINT ( 'NONE',  ( 755.0636971347428243, -124.2709662947837899, -341.7834795799807353 ) ) ;
#2673 = CARTESIAN_POINT ( 'NONE',  ( 804.9363028652555840, -64.27096629478397460, 338.2165204200192079 ) ) ;
#2674 = CARTESIAN_POINT ( 'NONE',  ( 815.1787889125755555, -246.8965053807777679, -343.7953271457877804 ) ) ;
#2675 = CARTESIAN_POINT ( 'NONE',  ( -454.7528517110260964, 240.0000000000001421, -122.7905160835438068 ) ) ;
#2676 = CARTESIAN_POINT ( 'NONE',  ( 766.5853460496234675, -373.9874144716864066, 372.3518521366060554 ) ) ;
#2677 = VERTEX_POINT ( 'NONE', #21737 ) ;
#2678 = CARTESIAN_POINT ( 'NONE',  ( 781.8018195045266339, -286.2709662947833635, 365.1927285166406705 ) ) ;
#2679 = CARTESIAN_POINT ( 'NONE',  ( 808.0189434323515343, 9.910851887033969021, 319.0252816721025511 ) ) ;
#2680 = CARTESIAN_POINT ( 'NONE',  ( 793.2243759319678702, -26.53286901714210799, -318.4439275373583200 ) ) ;
#2681 = CARTESIAN_POINT ( 'NONE',  ( 756.5762568750052424, -171.1800572038745543, -348.7366044899774238 ) ) ;
#2682 = CARTESIAN_POINT ( 'NONE',  ( 755.0636971347428243, -364.2709662947830793, 341.7834795799807353 ) ) ;
#2683 = CARTESIAN_POINT ( 'NONE',  ( 814.5518280994195948, -111.7255117493293000, -332.4837098697145734 ) ) ;
#2684 = CARTESIAN_POINT ( 'NONE',  ( 797.6776695296629214, -115.5436935675110988, -357.6776695296636603 ) ) ;
#2685 = ORIENTED_EDGE ( 'NONE', *, *, #32862, .T. ) ;
#2686 = CARTESIAN_POINT ( 'NONE',  ( 766.9102291470427417, -42.55451811788057626, -318.6633372737382501 ) ) ;
#2687 = CARTESIAN_POINT ( 'NONE',  ( 775.8780910478218402, -345.2817908451523863, -364.9511171171680530 ) ) ;
#2688 = EDGE_CURVE ( 'NONE', #33757, #23899, #35833, .T. ) ;
#2690 = CARTESIAN_POINT ( 'NONE',  ( 761.4292242960306112, -401.4636090269704027, 323.2154366446414429 ) ) ;
#2689 = CARTESIAN_POINT ( 'NONE',  ( 788.7366044899766848, -107.9073299311474727, 316.5762568750059813 ) ) ;
#2691 = AXIS2_PLACEMENT_3D ( 'NONE', #6556, #20411, #34260 ) ;
#2694 = CARTESIAN_POINT ( 'NONE',  ( 752.4576283171824116, -357.0783235625956422, 317.7880784355627952 ) ) ;
#2693 = CARTESIAN_POINT ( 'NONE',  ( 939.9999999999993179, -600.0000000000001137, -360.0000000000000000 ) ) ;
#2692 = CARTESIAN_POINT ( 'NONE',  ( 814.9108240113580450, -448.2709662947827951, 337.5031285880265273 ) ) ;
#2695 = ADVANCED_FACE ( 'NONE', ( #18302 ), #32380, .F. ) ;
#2696 = CARTESIAN_POINT ( 'NONE',  ( 755.5913626894240451, -373.6454272087887034, -346.6156483768012890 ) ) ;
#2697 = CARTESIAN_POINT ( 'NONE',  ( 755.3201227861273992, -339.7255117493285184, -345.3687786644892981 ) ) ;
#2698 = CARTESIAN_POINT ( 'NONE',  ( 804.1009440267234822, -119.4636090269712554, -314.0944755984392600 ) ) ;
#2699 = CARTESIAN_POINT ( 'NONE',  ( 760.0363995740630116, -10.91815448151704793, 368.7758568127991907 ) ) ;
#2701 = LINE ( 'NONE', #16798, #7052 ) ;
#2700 = FACE_OUTER_BOUND ( 'NONE', #35564, .T. ) ;
#2702 = CARTESIAN_POINT ( 'NONE',  ( 770.0799878456142551, -253.9874144716868329, -362.9823548866085616 ) ) ;
#2703 = CARTESIAN_POINT ( 'NONE',  ( 804.1009440267234822, -143.4636090269711701, -314.0944755984392600 ) ) ;
#2704 = CARTESIAN_POINT ( 'NONE',  ( 571.1634899080285095, 256.4999999999999432, -199.9999999999981526 ) ) ;
#2706 = EDGE_CURVE ( 'NONE', #8202, #16020, #43813, .T. ) ;
#2705 = CARTESIAN_POINT ( 'NONE',  ( -180.7583438952258916, 294.6698570112193920, -224.9999999999999716 ) ) ;
#2707 = AXIS2_PLACEMENT_3D ( 'NONE', #35758, #1104, #14761 ) ;
#2708 = EDGE_CURVE ( 'NONE', #5066, #9279, #9897, .T. ) ;
#2709 = CARTESIAN_POINT ( 'NONE',  ( 805.2837595273609850, -338.7363362996978822, 340.5290396650784714 ) ) ;
#2710 = ORIENTED_EDGE ( 'NONE', *, *, #30034, .T. ) ;
#2711 = CARTESIAN_POINT ( 'NONE',  ( 804.1009440267234822, -311.4636090269706870, 314.0944755984392600 ) ) ;
#2712 = CARTESIAN_POINT ( 'NONE',  ( 800.9747183278959710, -156.9982390220564241, -311.9810565676471583 ) ) ;
#2713 = CARTESIAN_POINT ( 'NONE',  ( 914.9999999999992042, 74.99999999999984368, -360.0000000000000000 ) ) ;
#2714 = CARTESIAN_POINT ( 'NONE',  ( 805.6418435158337843, -125.4636090269712412, 363.8556311672236916 ) ) ;
#2715 = CARTESIAN_POINT ( 'NONE',  ( 811.0346526505616112, -302.6346026584196238, -323.0537975583477532 ) ) ;
#2716 = CARTESIAN_POINT ( 'NONE',  ( -37.63011601220122770, -544.8427095258973623, -350.0000000000000000 ) ) ;
#2718 = MANIFOLD_SOLID_BREP ( 'CBORE for M5 Hex Head Bolt1[2]', #11423 ) ;
#2717 = CARTESIAN_POINT ( 'NONE',  ( 787.4999999999992042, -462.9681489794448339, -369.0473750965555837 ) ) ;
#2719 = CARTESIAN_POINT ( 'NONE',  ( 759.9864689768902508, -146.0891481129655176, 354.9819416627836404 ) ) ;
#2720 = ORIENTED_EDGE ( 'NONE', *, *, #37012, .T. ) ;
#2721 = CARTESIAN_POINT ( 'NONE',  ( 805.6418435158337843, -413.4636090269704027, 363.8556311672236916 ) ) ;
#2722 = CARTESIAN_POINT ( 'NONE',  ( 813.9316612368132837, -367.4419599262319025, -348.6739635108323228 ) ) ;
#2723 = CARTESIAN_POINT ( 'NONE',  ( 808.0189434323515343, -110.0891481129656597, -319.0252816721025511 ) ) ;
#2724 = CARTESIAN_POINT ( 'NONE',  ( 760.7433823573367135, -60.00906357242598688, 355.9930595647440441 ) ) ;
#2725 = CARTESIAN_POINT ( 'NONE',  ( 814.9108240113580450, -376.2709662947829656, -337.5031285880265273 ) ) ;
#2726 = CARTESIAN_POINT ( 'NONE',  ( 787.4999999999992042, -512.9681489794448908, -309.9999999999998863 ) ) ;
#2727 = CARTESIAN_POINT ( 'NONE',  ( 756.1348686366196716, -425.2601417444136018, 347.5531968255698416 ) ) ;
#2728 = ORIENTED_EDGE ( 'NONE', *, *, #6661, .F. ) ;
#2729 = CARTESIAN_POINT ( 'NONE',  ( 755.3201227861273992, -267.7255117493286320, 345.3687786644892981 ) ) ;
#2730 = AXIS2_PLACEMENT_3D ( 'NONE', #3897, #25127, #45243 ) ;
#2731 = CIRCLE ( 'NONE', #18210, 10.00000000000000888 ) ;
#2732 = CARTESIAN_POINT ( 'NONE',  ( 776.2433038121456548, -156.8965053807780805, -374.8207195650711014 ) ) ;
#2733 = DIRECTION ( 'NONE',  ( -1.000000000000000000, -0.000000000000000000, -0.000000000000000000 ) ) ;
#2734 = CARTESIAN_POINT ( 'NONE',  ( 800.1688906516307043, -274.1692326535049915, 369.0717654672308186 ) ) ;
#2735 = CARTESIAN_POINT ( 'NONE',  ( 797.6776695296629214, -91.54369356751116982, 357.6776695296636603 ) ) ;
#2736 = VERTEX_POINT ( 'NONE', #44578 ) ;
#2737 = CARTESIAN_POINT ( 'NONE',  ( 794.1144889064781864, -10.16923265350579442, -360.9840315886528401 ) ) ;
#2738 = CARTESIAN_POINT ( 'NONE',  ( 774.6312213355099630, -263.3618753856924855, 364.6798772138717482 ) ) ;
#2739 = CARTESIAN_POINT ( 'NONE',  ( 782.4968714119720516, -10.81642084023869543, -305.0891759886411023 ) ) ;
#2740 = CARTESIAN_POINT ( 'NONE',  ( 790.0208454995162128, -448.6851210678752864, 365.6426314972804903 ) ) ;
#2741 = VERTEX_POINT ( 'NONE', #23318 ) ;
#2742 = ORIENTED_EDGE ( 'NONE', *, *, #25270, .T. ) ;
#2743 = CARTESIAN_POINT ( 'NONE',  ( 815.3608509340175488, -410.7363362996976548, -341.2497674668889545 ) ) ;
#2744 = EDGE_CURVE ( 'NONE', #13947, #12019, #37222, .T. ) ;
#2745 = CARTESIAN_POINT ( 'NONE',  ( 794.9819416627830151, -252.9982390220560831, -319.9864689768909898 ) ) ;
#2747 = CARTESIAN_POINT ( 'NONE',  ( 791.1614460488616487, -251.2601417444141134, 373.5763878283158874 ) ) ;
#2746 = CARTESIAN_POINT ( 'NONE',  ( 759.0252816721024374, -360.9982390220557704, 368.0189434323527280 ) ) ;
#2748 = CARTESIAN_POINT ( 'NONE',  ( 790.0220218866281812, -271.0999726633344267, -363.2186876482849129 ) ) ;
#2749 = CARTESIAN_POINT ( 'NONE',  ( 778.1981804954714335, -202.2709662947834772, -314.8072714833589885 ) ) ;
#2750 = CARTESIAN_POINT ( 'NONE',  ( 771.2633955100217236, -431.9073299311464211, -363.4237431249939618 ) ) ;
#2751 = CARTESIAN_POINT ( 'NONE',  ( 788.8264449731200330, -237.1800572038742985, 363.6646147819171233 ) ) ;
#2752 = EDGE_LOOP ( 'NONE', ( #5471, #20327, #25171, #15457 ) ) ;
#2753 = CIRCLE ( 'NONE', #18985, 10.00000000000000888 ) ;
#2754 = CARTESIAN_POINT ( 'NONE',  ( 744.7301800767019131, -364.8164208402374697, 337.4774526936615757 ) ) ;
#2755 = CARTESIAN_POINT ( 'NONE',  ( -879.9999999999992042, 260.0000000000002274, -219.9999999999999716 ) ) ;
#2756 = CARTESIAN_POINT ( 'NONE',  ( 755.8990559732751535, -11.46360902697159290, -365.9055244015606831 ) ) ;
#2757 = CARTESIAN_POINT ( 'NONE',  ( 783.6926022324497580, 16.45630643248849267, 313.7971720364932935 ) ) ;
#2759 = EDGE_CURVE ( 'NONE', #17388, #33219, #5502, .T. ) ;
#2758 = CARTESIAN_POINT ( 'NONE',  ( -468.8365100919714337, 256.5000000000001705, -193.8809999999909053 ) ) ;
#2760 = CARTESIAN_POINT ( 'NONE',  ( 773.4516893846965786, -211.6454272087891582, 315.8398074228977066 ) ) ;
#2761 = CARTESIAN_POINT ( 'NONE',  ( 801.9419747391806368, -114.4527844766020053, 351.9812246680014027 ) ) ;
#2762 = ORIENTED_EDGE ( 'NONE', *, *, #25210, .F. ) ;
#2763 = CARTESIAN_POINT ( 'NONE',  ( 790.9844846989617508, 1.627300063937458408, -317.2208543904092721 ) ) ;
#2764 = CARTESIAN_POINT ( 'NONE',  ( 772.5602148656447525, -81.72551174932937101, -305.7998596910095443 ) ) ;
#2765 = CARTESIAN_POINT ( 'NONE',  ( 779.4709603349208464, -264.3510508353232353, 314.7162404726379918 ) ) ;
#2766 = AXIS2_PLACEMENT_3D ( 'NONE', #23148, #37257, #2373 ) ;
#2767 = CARTESIAN_POINT ( 'NONE',  ( 771.2633955100217236, -431.9073299311464211, -363.4237431249939618 ) ) ;
#2768 = CARTESIAN_POINT ( 'NONE',  ( 755.3201227861273992, -27.72551174932954510, -345.3687786644892981 ) ) ;
#2769 = CARTESIAN_POINT ( 'NONE',  ( 810.7187646348534145, -450.4527844766009821, 356.7737145352016341 ) ) ;
#2770 = CARTESIAN_POINT ( 'NONE',  ( 794.9999999999993179, 205.0000000000000568, 265.0000000000000000 ) ) ;
#2771 = CARTESIAN_POINT ( 'NONE',  ( 801.1904061080336987, -188.0891481129653187, -368.3070685750235498 ) ) ;
#2772 = CARTESIAN_POINT ( 'NONE',  ( 751.6929314249748586, -78.99823902205662307, 318.8095938919659034 ) ) ;
#2773 = CARTESIAN_POINT ( 'NONE',  ( 813.1304606946830518, -185.9073299311472454, 352.3570229623690580 ) ) ;
#2774 = DIRECTION ( 'NONE',  ( -1.000000000000000000, -0.000000000000000000, -0.000000000000000000 ) ) ;
#2775 = CARTESIAN_POINT ( 'NONE',  ( -911.9749999999993406, 154.9999999999998863, -360.0000000000000000 ) ) ;
#2776 = CARTESIAN_POINT ( 'NONE',  ( 764.3348316497523456, -262.7146871989594956, -308.6759233522265617 ) ) ;
#2777 = CARTESIAN_POINT ( 'NONE',  ( 810.4231160770870019, -408.5545181178794110, 321.9338519418446936 ) ) ;
#2778 = CARTESIAN_POINT ( 'NONE',  ( 749.2812353651451076, -270.4527844766014937, -323.2262854647983090 ) ) ;
#2779 = CYLINDRICAL_SURFACE ( 'NONE', #28718, 10.00000000000000888 ) ;
#2780 = CARTESIAN_POINT ( 'NONE',  ( 767.6429770376289525, -393.1800572038737300, 306.8695393053162093 ) ) ;
#2781 = CARTESIAN_POINT ( 'NONE',  ( 814.5518280994195948, -15.72551174932958951, 332.4837098697145166 ) ) ;
#2782 = CARTESIAN_POINT ( 'NONE',  ( 774.6858677611749044, -345.7255117493285184, -315.5713283507209894 ) ) ;
#2783 = CARTESIAN_POINT ( 'NONE',  ( 805.1016975059191054, -30.89650538077846065, 343.0745993439771837 ) ) ;
#2784 = CARTESIAN_POINT ( 'NONE',  ( 786.2056067578752163, -59.80559628986927834, -374.4686193811670023 ) ) ;
#2785 = CARTESIAN_POINT ( 'NONE',  ( 763.2154366446407039, -141.6237781080508569, -321.4292242960311228 ) ) ;
#2786 = CARTESIAN_POINT ( 'NONE',  ( 747.3154664389472828, -163.9874144716871456, 326.4474001241230781 ) ) ;
#2787 = CARTESIAN_POINT ( 'NONE',  ( 803.4237431249931660, 8.819942796124882634, 331.2633955100225194 ) ) ;
#2788 = CARTESIAN_POINT ( 'NONE',  ( 758.0141637701419768, -183.0783235625961538, 367.2620300519063790 ) ) ;
#2789 = VERTEX_POINT ( 'NONE', #27025 ) ;
#2790 = CARTESIAN_POINT ( 'NONE',  ( 755.5713283507202505, -77.36187538569302546, -334.6858677611754729 ) ) ;
#2791 = CARTESIAN_POINT ( 'NONE',  ( 776.9566956441375396, -156.8965053807780805, -364.8461984189686405 ) ) ;
#2792 = CARTESIAN_POINT ( 'NONE',  ( 778.2165204200184689, -166.8164208402382087, 364.9363028652563230 ) ) ;
#2793 = CARTESIAN_POINT ( 'NONE',  ( 800.1688906516307043, 13.83076734649413098, -369.0717654672308186 ) ) ;
#2795 = CARTESIAN_POINT ( 'NONE',  ( 756.5762568750052424, -291.1800572038741848, 348.7366044899774238 ) ) ;
#2794 = CARTESIAN_POINT ( 'NONE',  ( 762.3223304703356007, -295.5436935675105588, 322.3223304703362828 ) ) ;
#2796 = CARTESIAN_POINT ( 'NONE',  ( -26.63011601220122060, -110.5936016518799221, 750.6326042729449455 ) ) ;
#2797 = ORIENTED_EDGE ( 'NONE', *, *, #18532, .T. ) ;
#2798 = CARTESIAN_POINT ( 'NONE',  ( 770.0799878456142551, -13.98741447168760033, 362.9823548866085616 ) ) ;
#2799 = CARTESIAN_POINT ( 'NONE',  ( 783.7953271457878373, -320.1908817542434349, -375.1787889125761239 ) ) ;
#2800 = AXIS2_PLACEMENT_3D ( 'NONE', #39327, #7928, #21531 ) ;
#2801 = CARTESIAN_POINT ( 'NONE',  ( 796.9462024416508257, -252.4527844766015789, 308.9653473494370246 ) ) ;
#2802 = CARTESIAN_POINT ( 'NONE',  ( 763.0428371773158460, -323.4636090269706301, 358.7617431975195359 ) ) ;
#2803 = CARTESIAN_POINT ( 'NONE',  ( 772.3691319403857278, -431.2601417444136018, 315.8894580844506663 ) ) ;
#2804 = CARTESIAN_POINT ( 'NONE',  ( 784.1219089521767955, -141.2817908451530400, -315.0488828828318333 ) ) ;
#2805 = CARTESIAN_POINT ( 'NONE',  ( 759.9864689768902508, -122.0891481129656171, -354.9819416627836404 ) ) ;
#2806 = CARTESIAN_POINT ( 'NONE',  ( 754.8072714833583632, -316.8164208402377540, -338.1981804954721156 ) ) ;
#2807 = ORIENTED_EDGE ( 'NONE', *, *, #14574, .T. ) ;
#2808 = CARTESIAN_POINT ( 'NONE',  ( 774.6858677611749044, -417.7255117493283478, -315.5713283507209894 ) ) ;
#2809 = CARTESIAN_POINT ( 'NONE',  ( 800.7704444035546203, -316.1692326535048210, 326.0291762391768771 ) ) ;
#2810 = CARTESIAN_POINT ( 'NONE',  ( 187.1337867209877857, -185.0721577059061644, -75.19946970736494052 ) ) ;
#2811 = CARTESIAN_POINT ( 'NONE',  ( 51.16348990802859475, 230.0000000000000284, -197.2499999999946851 ) ) ;
#2812 = CARTESIAN_POINT ( 'NONE',  ( 758.4439275373578084, -132.5545181178802920, 353.2243759319684386 ) ) ;
#2813 = CARTESIAN_POINT ( 'NONE',  ( 803.6646147819161570, 6.092670068852159559, 348.8264449731210561 ) ) ;
#2814 = ORIENTED_EDGE ( 'NONE', *, *, #20986, .T. ) ;
#2815 = CARTESIAN_POINT ( 'NONE',  ( 747.6481478633932056, -349.0999726633342561, -353.4146539503763620 ) ) ;
#2816 = CARTESIAN_POINT ( 'NONE',  ( 755.1538015810308480, -230.1908817542436338, 343.0433043558613804 ) ) ;
#2817 = CARTESIAN_POINT ( 'NONE',  ( 802.2119215644370342, -222.0090635724254184, 367.5423716828165084 ) ) ;
#2818 = CARTESIAN_POINT ( 'NONE',  ( 755.5713283507202505, -317.3618753856922581, -334.6858677611754729 ) ) ;
#2819 = DIRECTION ( 'NONE',  ( 0.000000000000000000, 0.000000000000000000, -1.000000000000000000 ) ) ;
#2820 = CARTESIAN_POINT ( 'NONE',  ( 758.4439275373578084, -180.5545181178801499, -353.2243759319684386 ) ) ;
#2821 = CARTESIAN_POINT ( 'NONE',  ( 744.7301800767019131, -52.81642084023856398, 337.4774526936615757 ) ) ;
#2822 = CARTESIAN_POINT ( 'NONE',  ( -858.8365100919713768, 256.5000000000002274, -193.8809999999881768 ) ) ;
#2823 = CARTESIAN_POINT ( 'NONE',  ( 744.7301800767020268, -364.8164208402375266, -337.4774526936615189 ) ) ;
#2824 = DIRECTION ( 'NONE',  ( -1.000000000000000000, -0.000000000000000000, 0.000000000000000000 ) ) ;
#2825 = CARTESIAN_POINT ( 'NONE',  ( 807.2620300519052989, -312.0090635724251911, 318.0141637701419768 ) ) ;
#2826 = LINE ( 'NONE', #36640, #40486 ) ;
#2827 = CARTESIAN_POINT ( 'NONE',  ( 815.2698199232961542, -304.8164208402376403, 342.5225473063383106 ) ) ;
#2828 = CARTESIAN_POINT ( 'NONE',  ( 751.9810565676468741, -2.089148112965993231, -360.9747183278973921 ) ) ;
#2829 = CARTESIAN_POINT ( 'NONE',  ( 755.0636971347428243, -244.2709662947834204, -341.7834795799807353 ) ) ;
#2830 = DIRECTION ( 'NONE',  ( 0.000000000000000000, -1.000000000000000000, 0.000000000000000000 ) ) ;
#2831 = CARTESIAN_POINT ( 'NONE',  ( 774.6312213355099630, -383.3618753856921444, 364.6798772138717482 ) ) ;
#2832 = CARTESIAN_POINT ( 'NONE',  ( 754.7162404726377645, -158.7363362996984222, 339.4709603349214717 ) ) ;
#2833 = CARTESIAN_POINT ( 'NONE',  ( 799.9636004259356241, -22.91815448151701062, -311.2241431872006956 ) ) ;
#2834 = CARTESIAN_POINT ( 'NONE',  ( 770.0799878456142551, -37.98741447168752927, -362.9823548866085616 ) ) ;
#2835 = CARTESIAN_POINT ( 'NONE',  ( 773.7943932421234194, -71.80559628986922860, 305.5313806188329409 ) ) ;
#2836 = CARTESIAN_POINT ( 'NONE',  ( 797.8594530101009923, -373.5436935675102177, 322.1405469898982119 ) ) ;
#2837 = DIRECTION ( 'NONE',  ( 0.000000000000000000, 0.000000000000000000, 1.000000000000000000 ) ) ;
#2838 = DIRECTION ( 'NONE',  ( 0.000000000000000000, 0.000000000000000000, 1.000000000000000000 ) ) ;
#2839 = CARTESIAN_POINT ( 'NONE',  ( 802.1676090361156639, -422.6346026584192259, 327.8955696845344505 ) ) ;
#2840 = EDGE_LOOP ( 'NONE', ( #30324, #23890, #9441, #26256, #17162 ) ) ;
#2841 = CARTESIAN_POINT ( 'NONE',  ( 768.0187753319979720, -56.63460265842036279, -318.0580252608186242 ) ) ;
#2842 = CARTESIAN_POINT ( 'NONE',  ( 780.5290396650775619, -372.3510508353228374, -365.2837595273619513 ) ) ;
#2844 = CARTESIAN_POINT ( 'NONE',  ( 804.9363028652555840, -184.2709662947835909, 338.2165204200192079 ) ) ;
#2843 = CARTESIAN_POINT ( 'NONE',  ( 804.4286716492782716, -209.3618753856926276, 345.3141322388244703 ) ) ;
#2845 = CARTESIAN_POINT ( 'NONE',  ( 815.1787889125755555, -366.8965053807773984, -343.7953271457877804 ) ) ;
#2846 = DIRECTION ( 'NONE',  ( 0.000000000000000000, 0.000000000000000000, 1.000000000000000000 ) ) ;
#2847 = ORIENTED_EDGE ( 'NONE', *, *, #24646, .T. ) ;
#2848 = CARTESIAN_POINT ( 'NONE',  ( 802.1676090361156639, -398.6346026584193396, 327.8955696845344505 ) ) ;
#2849 = ORIENTED_EDGE ( 'NONE', *, *, #4352, .F. ) ;
#2850 =( NAMED_UNIT ( * ) PLANE_ANGLE_UNIT ( ) SI_UNIT ( $, .RADIAN. ) );
#2851 = CARTESIAN_POINT ( 'NONE',  ( 812.7932403749906598, -231.1800572038743553, -327.7687537140311633 ) ) ;
#2852 = CARTESIAN_POINT ( 'NONE',  ( 777.4774526936600978, -130.2709662947837614, 304.7301800767028226 ) ) ;
#2853 = ORIENTED_EDGE ( 'NONE', *, *, #4945, .F. ) ;
#2854 = CARTESIAN_POINT ( 'NONE',  ( 758.0580252608178853, -198.4527844766017495, -328.0187753319985404 ) ) ;
#2855 = ORIENTED_EDGE ( 'NONE', *, *, #19344, .F. ) ;
#2856 = CIRCLE ( 'NONE', #24244, 9.999999999999980460 ) ;
#2857 = CARTESIAN_POINT ( 'NONE',  ( 757.8323909638827445, -314.6346026584194533, -352.1044303154654358 ) ) ;
#2858 = CARTESIAN_POINT ( 'NONE',  ( 755.8894580844503253, -447.8272453906067199, -332.3691319403863531 ) ) ;
#2859 = CARTESIAN_POINT ( 'NONE',  ( 800.7704444035546203, -196.1692326535052473, 326.0291762391768771 ) ) ;
#2860 = DIRECTION ( 'NONE',  ( -0.000000000000000000, 1.000000000000000000, -0.000000000000000000 ) ) ;
#2861 = CARTESIAN_POINT ( 'NONE',  ( 791.7608162188021197, 205.0000000000000568, -339.9999999999999432 ) ) ;
#2862 = MANIFOLD_SOLID_BREP ( '<Heavy Cast Iron Table Bed Base>-<Fillet2>', #27633 ) ;
#2863 = ORIENTED_EDGE ( 'NONE', *, *, #5989, .T. ) ;
#2864 = CARTESIAN_POINT ( 'NONE',  ( 754.7162404726377645, -446.7363362996975980, -339.4709603349214717 ) ) ;
#2865 = LINE ( 'NONE', #23856, #12937 ) ;
#2866 = CARTESIAN_POINT ( 'NONE',  ( 746.4999999999993179, -365.3551492539851893, -8.132432514707076621 ) ) ;
#2867 = ORIENTED_EDGE ( 'NONE', *, *, #33082, .T. ) ;
#2868 = CARTESIAN_POINT ( 'NONE',  ( 746.4236121716829757, -255.8272453906072315, -328.8385539511384650 ) ) ;
#2869 = CARTESIAN_POINT ( 'NONE',  ( 755.8990559732751535, -107.4636090269713122, 365.9055244015606831 ) ) ;
#2871 = CARTESIAN_POINT ( 'NONE',  ( 791.9812246680005501, -212.6346026584198796, -361.9419747391813189 ) ) ;
#2870 = DIRECTION ( 'NONE',  ( 0.000000000000000000, -1.000000000000000000, -1.672022627447524993E-16 ) ) ;
#2872 = CARTESIAN_POINT ( 'NONE',  ( 803.8651313633788504, -413.2601417444136018, -332.4468031744301015 ) ) ;
#2873 = CARTESIAN_POINT ( 'NONE',  ( 813.5763878283155464, -243.8272453906072030, -351.1614460488615350 ) ) ;
#2874 = LINE ( 'NONE', #13736, #20844 ) ;
#2875 = CARTESIAN_POINT ( 'NONE',  ( -775.4999999999993179, -365.3551492539851893, -18.13243251470705886 ) ) ;
#2876 = CARTESIAN_POINT ( 'NONE',  ( 804.1105419155481968, -75.82724539060775726, -347.6308680596136469 ) ) ;
#2877 = CARTESIAN_POINT ( 'NONE',  ( 776.9254006560222479, -428.1908817542430938, 314.8983024940802125 ) ) ;
#2878 = FACE_OUTER_BOUND ( 'NONE', #35462, .T. ) ;
#2879 = CARTESIAN_POINT ( 'NONE',  ( 786.6156483768007774, -433.4419599262316183, -315.5913626894246136 ) ) ;
#2880 = CARTESIAN_POINT ( 'NONE',  ( 748.9653473494365699, -266.6346026584197375, -356.9462024416520762 ) ) ;
#2881 = CARTESIAN_POINT ( 'NONE',  ( 775.4999999999993179, -563.3203001761230553, -342.3463313526983143 ) ) ;
#2882 = DIRECTION ( 'NONE',  ( -0.000000000000000000, 1.000000000000000000, -0.000000000000000000 ) ) ;
#2883 = CARTESIAN_POINT ( 'NONE',  ( 804.9363028652555840, -88.27096629478390355, -338.2165204200192079 ) ) ;
#2884 = CARTESIAN_POINT ( 'NONE',  ( 781.2370466360911223, -212.7363362996982232, 304.9990715423533629 ) ) ;
#2885 = CARTESIAN_POINT ( 'NONE',  ( 815.1787889125755555, -150.8965053807781089, -343.7953271457877804 ) ) ;
#2886 = CARTESIAN_POINT ( 'NONE',  ( 792.2312462859673587, -203.9073299311471885, 307.2067596250082602 ) ) ;
#2887 = CARTESIAN_POINT ( 'NONE',  ( 777.5031285880264704, -406.8164208402375266, -374.9108240113588408 ) ) ;
#2888 = DIRECTION ( 'NONE',  ( 0.000000000000000000, 0.000000000000000000, -1.000000000000000000 ) ) ;
#2889 = CARTESIAN_POINT ( 'NONE',  ( 804.4286716492782716, -281.3618753856923718, 345.3141322388244703 ) ) ;
#2890 = CARTESIAN_POINT ( 'NONE',  ( 804.1105419155481968, -75.82724539060775726, 347.6308680596136469 ) ) ;
#2891 = CARTESIAN_POINT ( 'NONE',  ( 774.6858677611749044, -417.7255117493283478, -315.5713283507209894 ) ) ;
#2892 = CIRCLE ( 'NONE', #14720, 12.00000000000001066 ) ;
#2893 = PLANE ( 'NONE',  #43166 ) ;
#2894 = PLANE ( 'NONE',  #39520 ) ;
#2896 = CARTESIAN_POINT ( 'NONE',  ( 756.3353852180819104, -341.9073299311465917, 331.1735550268788302 ) ) ;
#2895 = CARTESIAN_POINT ( 'NONE',  ( 787.6308680596127942, -131.2601417444144829, 364.1105419155492768 ) ) ;
#2897 = ORIENTED_EDGE ( 'NONE', *, *, #38295, .F. ) ;
#2898 = ADVANCED_FACE ( 'NONE', ( #5539, #37640, #18973 ), #40216, .F. ) ;
#2899 = CARTESIAN_POINT ( 'NONE',  ( 761.2382568024794409, -255.6237781080504874, -356.9571628226838129 ) ) ;
#2900 = CARTESIAN_POINT ( 'NONE',  ( 764.8639956371174549, -80.08914811296574499, 319.7806653035542013 ) ) ;
#2901 = CARTESIAN_POINT ( 'NONE',  ( 808.7758568127978833, -244.1692326535050768, -320.0363995740631822 ) ) ;
#2902 = CARTESIAN_POINT ( 'NONE',  ( 786.4999999999993179, -496.5085659523897448, -356.8883017825714319 ) ) ;
#2903 = CARTESIAN_POINT ( 'NONE',  ( 801.9858362298568863, -363.0783235625955854, 312.7379699480935642 ) ) ;
#2904 = VERTEX_POINT ( 'NONE', #22866 ) ;
#2905 = CARTESIAN_POINT ( 'NONE',  ( 803.4237431249931660, -279.1800572038741848, 331.2633955100225194 ) ) ;
#2906 = CARTESIAN_POINT ( 'NONE',  ( 794.1144889064781864, -58.16923265350564520, -360.9840315886528401 ) ) ;
#2907 = CARTESIAN_POINT ( 'NONE',  ( 767.8955696845333705, -168.4527844766018347, -362.1676090361162323 ) ) ;
#2908 = CARTESIAN_POINT ( 'NONE',  ( 765.0180583372156207, -408.9982390220556567, 360.0135310231089534 ) ) ;
#2909 = EDGE_CURVE ( 'NONE', #33022, #33694, #40657, .T. ) ;
#2910 = CARTESIAN_POINT ( 'NONE',  ( 801.1904061080336987, -116.0891481129656029, -368.3070685750235498 ) ) ;
#2911 = CARTESIAN_POINT ( 'NONE',  ( 774.6312213355098493, -119.3618753856928834, -364.6798772138717482 ) ) ;
#2912 = ORIENTED_EDGE ( 'NONE', *, *, #37065, .T. ) ;
#2913 = CARTESIAN_POINT ( 'NONE',  ( 757.4527132478984868, -40.37269993606240348, -329.1273215169538844 ) ) ;
#2914 = CARTESIAN_POINT ( 'NONE',  ( 766.0291762391763086, -346.9181544815160123, -360.7704444035551319 ) ) ;
#2916 = CARTESIAN_POINT ( 'NONE',  ( 780.5236548040995785, -404.7363362996975980, 314.9735926884559944 ) ) ;
#2915 = CARTESIAN_POINT ( 'NONE',  ( 800.2193346964447755, -138.9982390220563957, 355.1360043628815788 ) ) ;
#2917 = CARTESIAN_POINT ( 'NONE',  ( 783.0433043558608688, -96.89650538077825104, 315.1538015810313027 ) ) ;
#2920 = CARTESIAN_POINT ( 'NONE',  ( 758.0141637701419768, -351.0783235625955854, 367.2620300519063790 ) ) ;
#2919 = FACE_OUTER_BOUND ( 'NONE', #27553, .T. ) ;
#2918 = CARTESIAN_POINT ( 'NONE',  ( -26.63011601220122060, -512.9681489794448908, -352.0000000000000000 ) ) ;
#2921 = CARTESIAN_POINT ( 'NONE',  ( 783.7566961878529810, -120.8965053807781800, 305.1792804349288417 ) ) ;
#2922 = CARTESIAN_POINT ( 'NONE',  ( 757.4527132478984868, -376.3726999360614514, -329.1273215169538844 ) ) ;
#2923 = CARTESIAN_POINT ( 'NONE',  ( 771.1735550268778070, -345.1800572038739006, -316.3353852180827630 ) ) ;
#2924 = CARTESIAN_POINT ( 'NONE',  ( 754.3581564841646241, -137.4636090269711985, -316.1443688327762516 ) ) ;
#2925 = CIRCLE ( 'NONE', #21356, 20.00000000000001776 ) ;
#2926 = CARTESIAN_POINT ( 'NONE',  ( 799.9636004259356241, 1.081845518482914104, 311.2241431872006956 ) ) ;
#2928 = CARTESIAN_POINT ( 'NONE',  ( 794.9999999999993179, -357.6843811873878280, -0.3380660510726891665 ) ) ;
#2927 = CARTESIAN_POINT ( 'NONE',  ( 879.9999999999992042, 99.99999999999984368, -350.0000000000000000 ) ) ;
#2929 = CARTESIAN_POINT ( 'NONE',  ( 804.1601925771018387, -271.4419599262321867, -346.5483106153029098 ) ) ;
#2930 = EDGE_CURVE ( 'NONE', #29766, #7990, #23958, .T. ) ;
#2931 = CARTESIAN_POINT ( 'NONE',  ( 778.7629533639073998, -152.7363362996983938, -375.0009284576466371 ) ) ;
#2932 = DIRECTION ( 'NONE',  ( -0.000000000000000000, 1.000000000000000000, -0.000000000000000000 ) ) ;
#2933 = LINE ( 'NONE', #19798, #13472 ) ;
#2934 = CARTESIAN_POINT ( 'NONE',  ( 766.0291762391763086, -346.9181544815160123, 360.7704444035551319 ) ) ;
#2935 = CARTESIAN_POINT ( 'NONE',  ( 747.6481478633932056, -301.0999726633342561, 353.4146539503763620 ) ) ;
#2936 = CARTESIAN_POINT ( 'NONE',  ( 814.5518280994195948, -183.7255117493290300, -332.4837098697145166 ) ) ;
#2937 = CARTESIAN_POINT ( 'NONE',  ( 786.4999999999993179, -365.3551492539851893, -8.132432514707076621 ) ) ;
#2938 = CARTESIAN_POINT ( 'NONE',  ( 791.0478386215596629, -93.82724539060770041, 306.7653713866226326 ) ) ;
#2939 = CARTESIAN_POINT ( 'NONE',  ( 814.5518280994195948, -303.7255117493287457, -332.4837098697145734 ) ) ;
#2940 = CARTESIAN_POINT ( 'NONE',  ( 959.5497976682736407, 120.6654763175833693, -209.9999999999999716 ) ) ;
#2941 = CARTESIAN_POINT ( 'NONE',  ( -879.9999999999992042, 260.0000000000002274, -179.9999999999999716 ) ) ;
#2942 = CARTESIAN_POINT ( 'NONE',  ( 755.3201227861273992, -195.7255117493289731, 345.3687786644892981 ) ) ;
#2943 = ORIENTED_EDGE ( 'NONE', *, *, #32872, .T. ) ;
#2944 = CARTESIAN_POINT ( 'NONE',  ( 749.5768839229115201, -420.5545181178793541, 358.0661480581553064 ) ) ;
#2945 = CARTESIAN_POINT ( 'NONE',  ( 761.9338519418445230, -374.5328690171410813, -370.4231160770881957 ) ) ;
#2946 = CARTESIAN_POINT ( 'NONE',  ( 763.2262854647970016, -128.6346026584201354, -309.2812353651462445 ) ) ;
#2947 = EDGE_CURVE ( 'NONE', #11840, #5018, #12035, .T. ) ;
#2948 = CARTESIAN_POINT ( 'NONE',  ( 798.5707757039680246, -53.46360902697146855, 356.7845633553585003 ) ) ;
#2949 = CARTESIAN_POINT ( 'NONE',  ( 814.2001403089898304, -401.3618753856920307, -347.4397851343538264 ) ) ;
#2950 = CARTESIAN_POINT ( 'NONE',  ( -786.4999999999993179, -494.6608068873671300, -357.6536686473015720 ) ) ;
#2951 = CARTESIAN_POINT ( 'NONE',  ( 801.3366627262608972, -440.5328690171407970, 353.0897708529566899 ) ) ;
#2952 = VERTEX_POINT ( 'NONE', #44343 ) ;
#2953 = EDGE_CURVE ( 'NONE', #7990, #29766, #45355, .T. ) ;
#2954 = CARTESIAN_POINT ( 'NONE',  ( 752.4576283171824116, -141.0783235625962959, -317.7880784355627952 ) ) ;
#2955 = CARTESIAN_POINT ( 'NONE',  ( -39.63011601220123481, -512.9681489794448908, -339.9999999999999432 ) ) ;
#2956 = CARTESIAN_POINT ( 'NONE',  ( 795.6651683502461765, -274.7146871989594388, 371.3240766477733814 ) ) ;
#2957 = CARTESIAN_POINT ( 'NONE',  ( 768.0187753319979720, -128.6346026584201354, 318.0580252608186242 ) ) ;
#2958 = VERTEX_POINT ( 'NONE', #33493 ) ;
#2959 = CARTESIAN_POINT ( 'NONE',  ( 762.3223304703356007, -271.5436935675106156, 322.3223304703362828 ) ) ;
#2960 = ADVANCED_FACE ( 'NONE', ( #1842 ), #27635, .F. ) ;
#2961 = CARTESIAN_POINT ( 'NONE',  ( 755.2512626584698410, -7.543693567511430942, -315.2512626584710915 ) ) ;
#2962 = DIRECTION ( 'NONE',  ( 0.000000000000000000, 1.000000000000000000, 0.000000000000000000 ) ) ;
#2963 = ORIENTED_EDGE ( 'NONE', *, *, #31104, .T. ) ;
#2964 = ORIENTED_EDGE ( 'NONE', *, *, #13105, .F. ) ;
#2965 = CARTESIAN_POINT ( 'NONE',  ( 804.9363028652555840, -184.2709662947835909, -338.2165204200192079 ) ) ;
#2966 = CARTESIAN_POINT ( 'NONE',  ( 813.5763878283155464, -411.8272453906067199, -351.1614460488615350 ) ) ;
#2967 = CARTESIAN_POINT ( 'NONE',  ( 804.6798772138708955, -39.72551174932951312, 334.6312213355107019 ) ) ;
#2968 = CARTESIAN_POINT ( 'NONE',  ( 804.9363028652555840, -256.2709662947834204, -338.2165204200192079 ) ) ;
#2970 = CARTESIAN_POINT ( 'NONE',  ( 764.3348316497523456, -262.7146871989594956, 308.6759233522265617 ) ) ;
#2969 = CARTESIAN_POINT ( 'NONE',  ( 796.9462024416508257, -372.4527844766012095, 308.9653473494370246 ) ) ;
#2971 = CARTESIAN_POINT ( 'NONE',  ( 799.2566176426618085, -240.0090635724253900, -324.0069404352559559 ) ) ;
#2972 = CARTESIAN_POINT ( 'NONE',  ( 757.8323909638827445, -242.6346026584197659, -352.1044303154654358 ) ) ;
#2973 = CARTESIAN_POINT ( 'NONE',  ( 788.8264449731201466, -405.1800572038737869, -363.6646147819170665 ) ) ;
#2974 = CARTESIAN_POINT ( 'NONE',  ( 781.7834795799800531, -82.81642084023846451, -315.0636971347436202 ) ) ;
#2975 = EDGE_CURVE ( 'NONE', #24210, #43683, #44116, .T. ) ;
#2976 = CARTESIAN_POINT ( 'NONE',  ( 788.7366044899766848, -251.9073299311470748, 316.5762568750059813 ) ) ;
#2977 = EDGE_LOOP ( 'NONE', ( #34128, #28219, #43060, #8539 ) ) ;
#2978 = CARTESIAN_POINT ( 'NONE',  ( 745.4481719005789273, -363.7255117493284047, 347.5162901302853129 ) ) ;
#2979 = CARTESIAN_POINT ( 'NONE',  ( 772.4999999999993179, -512.9681489794448908, -339.9999999999999432 ) ) ;
#2980 = EDGE_CURVE ( 'NONE', #44849, #11829, #23929, .T. ) ;
#2981 = CARTESIAN_POINT ( 'NONE',  ( 749.5768839229115201, -60.55451811788051941, -358.0661480581553064 ) ) ;
#2982 = DIRECTION ( 'NONE',  ( 0.000000000000000000, -0.6594541114781790059, -0.7517448203044204691 ) ) ;
#2983 = FACE_OUTER_BOUND ( 'NONE', #799, .T. ) ;
#2984 = CARTESIAN_POINT ( 'NONE',  ( 755.3028492785439312, -231.2817908451527558, 335.9200461376539693 ) ) ;
#2985 = CARTESIAN_POINT ( 'NONE',  ( 803.4237431249931660, -111.1800572038747532, 331.2633955100225194 ) ) ;
#2986 = ORIENTED_EDGE ( 'NONE', *, *, #41717, .T. ) ;
#2987 = CARTESIAN_POINT ( 'NONE',  ( 755.3028492785439312, -15.28179084515340058, -335.9200461376539693 ) ) ;
#2988 = CARTESIAN_POINT ( 'NONE',  ( 805.0032342141413437, -85.54369356751118403, -314.9967657858572352 ) ) ;
#2989 = CARTESIAN_POINT ( 'NONE',  ( 756.1348686366196716, -281.2601417444139997, 347.5531968255698416 ) ) ;
#2990 = CARTESIAN_POINT ( 'NONE',  ( 804.6798772138708955, -447.7255117493280636, -334.6312213355107019 ) ) ;
#2991 = CARTESIAN_POINT ( 'NONE',  ( 774.6858677611749044, -33.72551174932952733, -315.5713283507209894 ) ) ;
#2992 = CARTESIAN_POINT ( 'NONE',  ( 813.1304606946830518, -449.9073299311463643, 352.3570229623690580 ) ) ;
#2993 = CARTESIAN_POINT ( 'NONE',  ( 763.0537975583475827, -192.4527844766016926, -371.0346526505627480 ) ) ;
#2994 = CARTESIAN_POINT ( 'NONE',  ( 744.7301800767019131, -172.8164208402381234, 337.4774526936615757 ) ) ;
#2995 = CARTESIAN_POINT ( 'NONE',  ( 758.0580252608178853, -78.45278447660211896, 328.0187753319985404 ) ) ;
#2996 = CARTESIAN_POINT ( 'NONE',  ( 914.9999999999992042, 74.99999999999984368, 350.0000000000000000 ) ) ;
#2997 = DIRECTION ( 'NONE',  ( 1.000000000000000000, 0.000000000000000000, 0.000000000000000000 ) ) ;
#2998 = CARTESIAN_POINT ( 'NONE',  ( 813.9316612368132837, -271.4419599262321867, -348.6739635108323228 ) ) ;
#2999 = EDGE_CURVE ( 'NONE', #14626, #24474, #40884, .T. ) ;
#3000 = CARTESIAN_POINT ( 'NONE',  ( 799.9636004259356241, -430.9181544815157849, 311.2241431872006956 ) ) ;
#3001 = CARTESIAN_POINT ( 'NONE',  ( 745.0891759886404770, -292.2709662947831930, -342.4968714119734159 ) ) ;
#3002 = DIRECTION ( 'NONE',  ( -1.000000000000000000, -0.000000000000000000, -0.000000000000000000 ) ) ;
#3003 = CARTESIAN_POINT ( 'NONE',  ( 787.4397851343537695, -405.7255117493283478, 374.2001403089903988 ) ) ;
#3004 = CARTESIAN_POINT ( 'NONE',  ( 748.9653473494365699, -26.63460265842046226, 356.9462024416520762 ) ) ;
#3005 = CARTESIAN_POINT ( 'NONE',  ( 811.6461892240364477, -28.71468719896028077, -324.1737431748509835 ) ) ;
#3006 = CARTESIAN_POINT ( 'NONE',  ( 755.5713283507202505, -389.3618753856919739, -334.6858677611754729 ) ) ;
#3007 = EDGE_CURVE ( 'NONE', #41246, #7001, #8498, .T. ) ;
#3008 = CARTESIAN_POINT ( 'NONE',  ( 787.6308680596127942, -35.26014174441480264, 364.1105419155492768 ) ) ;
#3009 = CARTESIAN_POINT ( 'NONE',  ( 815.1787889125755555, -54.89650538077837183, -343.7953271457877804 ) ) ;
#3010 = CARTESIAN_POINT ( 'NONE',  ( 804.1601925771018387, -151.4419599262326415, -346.5483106153029098 ) ) ;
#3011 = CARTESIAN_POINT ( 'NONE',  ( 761.9338519418445230, -158.5328690171417065, 370.4231160770881957 ) ) ;
#3012 = CARTESIAN_POINT ( 'NONE',  ( 762.1405469898973024, -25.54369356751137232, 357.8594530101016176 ) ) ;
#3013 = CARTESIAN_POINT ( 'NONE',  ( 815.0009284576459549, -174.3510508353234627, 338.7629533639073429 ) ) ;
#3014 = ORIENTED_EDGE ( 'NONE', *, *, #18532, .F. ) ;
#3015 = CARTESIAN_POINT ( 'NONE',  ( 758.0580252608178853, -54.45278447660219001, -328.0187753319985404 ) ) ;
#3016 = CARTESIAN_POINT ( 'NONE',  ( 776.9566956441375396, -180.8965053807779952, -364.8461984189686405 ) ) ;
#3017 = EDGE_CURVE ( 'NONE', #34587, #4508, #10696, .T. ) ;
#3018 = CARTESIAN_POINT ( 'NONE',  ( 774.6858677611749044, -177.7255117493290868, 315.5713283507209894 ) ) ;
#3019 = CARTESIAN_POINT ( 'NONE',  ( 807.5423716828161105, 14.92167643740321381, -362.2119215644372048 ) ) ;
#3020 = CARTESIAN_POINT ( 'NONE',  ( 797.8594530101009923, -301.5436935675105588, 322.1405469898982119 ) ) ;
#3021 = LINE ( 'NONE', #2796, #39689 ) ;
#3022 = ORIENTED_EDGE ( 'NONE', *, *, #32275, .F. ) ;
#3023 = CARTESIAN_POINT ( 'NONE',  ( 798.7617431975189675, -27.62377810805120149, 323.0428371773161871 ) ) ;
#3024 = CARTESIAN_POINT ( 'NONE',  ( 773.7305795820266212, -297.2817908451526137, -374.8230680027170365 ) ) ;
#3025 = CARTESIAN_POINT ( 'NONE',  ( 748.9653473494365699, -242.6346026584197659, 356.9462024416520762 ) ) ;
#3026 = CARTESIAN_POINT ( 'NONE',  ( 786.5483106153019435, -319.6454272087888739, 364.1601925771022366 ) ) ;
#3027 = CARTESIAN_POINT ( 'NONE',  ( 793.4146539503750546, 22.01258552831228599, 307.6481478633938877 ) ) ;
#3028 = CARTESIAN_POINT ( 'NONE',  ( 755.8894580844503253, -135.8272453906076009, -332.3691319403863531 ) ) ;
#3029 = CARTESIAN_POINT ( 'NONE',  ( 788.8264449731200330, -165.1800572038745258, -363.6646147819171233 ) ) ;
#3030 = VERTEX_POINT ( 'NONE', #3217 ) ;
#3031 = CARTESIAN_POINT ( 'NONE',  ( 761.2382568024794409, -351.6237781080502032, 356.9571628226838129 ) ) ;
#3032 = CARTESIAN_POINT ( 'NONE',  ( 999.5857864376259840, 249.9999999999998863, -199.9999999999999432 ) ) ;
#3033 = CARTESIAN_POINT ( 'NONE',  ( 763.8424801807145741, -138.0090635724257311, 320.5453621957614700 ) ) ;
#3034 = CARTESIAN_POINT ( 'NONE',  ( 785.3141322388236176, 2.274488250670355871, 364.4286716492789537 ) ) ;
#3035 = EDGE_LOOP ( 'NONE', ( #21215, #32230 ) ) ;
#3036 = CARTESIAN_POINT ( 'NONE',  ( 802.2119215644370342, -390.0090635724249069, -367.5423716828165084 ) ) ;
#3037 = DIRECTION ( 'NONE',  ( -0.000000000000000000, 1.000000000000000000, -0.000000000000000000 ) ) ;
#3038 = CARTESIAN_POINT ( 'NONE',  ( 768.9521613784389729, -249.8272453906072315, 373.2346286133773106 ) ) ;
#3039 = CARTESIAN_POINT ( 'NONE',  ( 755.8398074228967971, -187.4419599262325278, 333.4516893846970333 ) ) ;
#3040 = CARTESIAN_POINT ( 'NONE',  ( 758.0580252608178853, -342.4527844766013231, -328.0187753319985404 ) ) ;
#3041 = DIRECTION ( 'NONE',  ( 0.000000000000000000, -1.000000000000000000, 0.000000000000000000 ) ) ;
#3042 = CARTESIAN_POINT ( 'NONE',  ( 800.9840315886518738, -220.9181544815164102, -354.1144889064786412 ) ) ;
#3043 = CARTESIAN_POINT ( 'NONE',  ( 813.1304606946830518, -65.90732993114758642, 352.3570229623690580 ) ) ;
#3044 = LINE ( 'NONE', #38609, #24699 ) ;
#3045 = CARTESIAN_POINT ( 'NONE',  ( 808.3070685750232087, -402.9982390220555999, -361.1904061080339829 ) ) ;
#3046 = CYLINDRICAL_SURFACE ( 'NONE', #13598, 7.999999999999896083 ) ;
#3047 = CARTESIAN_POINT ( 'NONE',  ( 762.1177392798416577, -354.5545181178796383, 309.8865473780659272 ) ) ;
#3048 = CARTESIAN_POINT ( 'NONE',  ( 799.9999999999993179, -365.3551492539851893, -18.13243251470705886 ) ) ;
#3049 = CARTESIAN_POINT ( 'NONE',  ( 787.4397851343537695, -309.7255117493287457, 374.2001403089903988 ) ) ;
#3050 = CARTESIAN_POINT ( 'NONE',  ( 749.2812353651451076, -54.45278447660219001, -323.2262854647983090 ) ) ;
#3051 = CARTESIAN_POINT ( 'NONE',  ( 797.6776695296629214, -259.5436935675106156, -357.6776695296636603 ) ) ;
#3052 = DIRECTION ( 'NONE',  ( 0.000000000000000000, 0.000000000000000000, 1.000000000000000000 ) ) ;
#3053 = CARTESIAN_POINT ( 'NONE',  ( 758.0580252608178853, -390.4527844766011526, 328.0187753319985404 ) ) ;
#3054 = VECTOR ( 'NONE', #29626, 1000.000000000000000 ) ;
#3055 = CARTESIAN_POINT ( 'NONE',  ( 790.9844846989617508, -142.3726999360620766, 317.2208543904092721 ) ) ;
#3056 = CARTESIAN_POINT ( 'NONE',  ( 746.4236121716829757, -39.82724539060786384, -328.8385539511384650 ) ) ;
#3057 = CARTESIAN_POINT ( 'NONE',  ( 770.0799878456142551, -61.98741447168745822, -362.9823548866085616 ) ) ;
#3058 = CARTESIAN_POINT ( 'NONE',  ( 807.5423716828161105, -57.07832356259658013, 362.2119215644372048 ) ) ;
#3059 = CARTESIAN_POINT ( 'NONE',  ( 805.1927285166399315, -376.8164208402375834, 341.8018195045277707 ) ) ;
#3060 = CARTESIAN_POINT ( 'NONE',  ( 772.5602148656447525, 14.27448825067031812, 305.7998596910095443 ) ) ;
#3061 = CARTESIAN_POINT ( 'NONE',  ( 799.9999999999993179, -512.9681489794448908, -309.9999999999998863 ) ) ;
#3062 = CARTESIAN_POINT ( 'NONE',  ( 762.1405469898971887, -433.5436935675099903, 357.8594530101015607 ) ) ;
#3063 = CARTESIAN_POINT ( 'NONE',  ( 792.1044303154645831, -60.45278447660215448, -317.8323909638837677 ) ) ;
#3064 = CARTESIAN_POINT ( 'NONE',  ( 758.6633372737375112, -380.5328690171409676, -326.9102291470432533 ) ) ;
#3066 = CARTESIAN_POINT ( 'NONE',  ( 757.8323909638828582, -194.6346026584199080, 352.1044303154654358 ) ) ;
#3065 = CARTESIAN_POINT ( 'NONE',  ( 803.6646147819161570, -185.9073299311472454, 348.8264449731210561 ) ) ;
#3067 = CARTESIAN_POINT ( 'NONE',  ( 813.9316612368132837, -367.4419599262319025, -348.6739635108323228 ) ) ;
#3068 = DIRECTION ( 'NONE',  ( -1.000000000000000000, 0.000000000000000000, 0.000000000000000000 ) ) ;
#3069 = EDGE_LOOP ( 'NONE', ( #41787, #15073, #40615, #43520 ) ) ;
#3070 = CARTESIAN_POINT ( 'NONE',  ( 791.9812246680005501, -380.6346026584192828, 361.9419747391813189 ) ) ;
#3071 = ORIENTED_EDGE ( 'NONE', *, *, #44258, .T. ) ;
#3072 = CARTESIAN_POINT ( 'NONE',  ( 814.2001403089898304, -209.3618753856926276, -347.4397851343538264 ) ) ;
#3073 = CARTESIAN_POINT ( 'NONE',  ( 772.5602148656447525, -153.7255117493291721, 305.7998596910095443 ) ) ;
#3074 = EDGE_LOOP ( 'NONE', ( #11565, #26546, #9323, #31356 ) ) ;
#3075 = CARTESIAN_POINT ( 'NONE',  ( 744.8212110874229666, -186.8965053807779668, 336.2046728542121627 ) ) ;
#3076 = CARTESIAN_POINT ( 'NONE',  ( 778.1981804954715471, -202.2709662947835341, -314.8072714833591021 ) ) ;
#3077 = ORIENTED_EDGE ( 'NONE', *, *, #33082, .F. ) ;
#3078 = CARTESIAN_POINT ( 'NONE',  ( 803.4237431249931660, -375.1800572038739574, -331.2633955100225194 ) ) ;
#3079 = CARTESIAN_POINT ( 'NONE',  ( 778.1981804954714335, -10.27096629478414691, -314.8072714833589885 ) ) ;
#3080 = CARTESIAN_POINT ( 'NONE',  ( 790.8726784830453198, -202.7146871989597514, 362.5472867521010585 ) ) ;
#3081 = DIRECTION ( 'NONE',  ( 0.000000000000000000, 0.000000000000000000, -1.000000000000000000 ) ) ;
#3082 = DIRECTION ( 'NONE',  ( -0.000000000000000000, -0.000000000000000000, 1.000000000000000000 ) ) ;
#3083 = EDGE_LOOP ( 'NONE', ( #15792, #4178, #15921, #13120 ) ) ;
#3084 = CARTESIAN_POINT ( 'NONE',  ( 791.9812246680005501, 3.365397341579444479, -361.9419747391813189 ) ) ;
#3085 = DIRECTION ( 'NONE',  ( 1.000000000000000000, 0.000000000000000000, -0.000000000000000000 ) ) ;
#3086 = LINE ( 'NONE', #2866, #40334 ) ;
#3087 = VERTEX_POINT ( 'NONE', #20084 ) ;
#3088 = CARTESIAN_POINT ( 'NONE',  ( 745.5313806188320314, -279.2817908451526137, -333.7943932421247268 ) ) ;
#3089 = VECTOR ( 'NONE', #24966, 1000.000000000000000 ) ;
#3090 = CARTESIAN_POINT ( 'NONE',  ( 814.4686193811664907, -123.2817908451530542, 346.2056067578752732 ) ) ;
#3092 = CARTESIAN_POINT ( 'NONE',  ( 800.2193346964447755, -210.9982390220561967, -355.1360043628815788 ) ) ;
#3091 = CARTESIAN_POINT ( 'NONE',  ( 989.9999999999992042, 240.0000000000001990, 201.9999999999999716 ) ) ;
#3093 = CARTESIAN_POINT ( 'NONE',  ( 783.0433043558608688, -408.8965053807772847, -315.1538015810313027 ) ) ;
#3094 = LINE ( 'NONE', #34515, #5316 ) ;
#3095 = DIRECTION ( 'NONE',  ( 0.000000000000000000, -0.6594541114781790059, -0.7517448203044204691 ) ) ;
#3096 = CARTESIAN_POINT ( 'NONE',  ( 799.2566176426618085, -96.00906357242585898, -324.0069404352559559 ) ) ;
#3097 = LINE ( 'NONE', #10720, #15942 ) ;
#3098 = CARTESIAN_POINT ( 'NONE',  ( 781.2497674668890113, 11.64894916467595642, -375.3608509340180603 ) ) ;
#3099 = CARTESIAN_POINT ( 'NONE',  ( 746.8695393053151292, -293.9073299311468759, -327.6429770376306578 ) ) ;
#3100 = CYLINDRICAL_SURFACE ( 'NONE', #33467, 1.000000000000000888 ) ;
#3101 = CARTESIAN_POINT ( 'NONE',  ( 778.1981804954714335, 13.72903370521577138, 314.8072714833589885 ) ) ;
#3102 = CARTESIAN_POINT ( 'NONE',  ( 788.8264449731200330, -93.18005720387481006, -363.6646147819171233 ) ) ;
#3103 = CARTESIAN_POINT ( 'NONE',  ( 804.1009440267234822, -215.4636090269709712, 314.0944755984392600 ) ) ;
#3104 = CARTESIAN_POINT ( 'NONE',  ( 754.0944755984390895, -183.6237781080507148, -364.1009440267246760 ) ) ;
#3105 = CARTESIAN_POINT ( 'NONE',  ( 808.0189434323515343, -206.0891481129653471, 319.0252816721025511 ) ) ;
#3106 = CARTESIAN_POINT ( 'NONE',  ( 800.9747183278959710, -420.9982390220555999, -311.9810565676471583 ) ) ;
#3107 = CARTESIAN_POINT ( 'NONE',  ( 939.9999999999993179, -590.0000000000001137, -360.0000000000000000 ) ) ;
#3108 = CARTESIAN_POINT ( 'NONE',  ( 759.7806653035534055, -294.9982390220560546, 324.8639956371180801 ) ) ;
#3109 = ADVANCED_FACE ( 'NONE', ( #13398 ), #38115, .F. ) ;
#3110 = CARTESIAN_POINT ( 'NONE',  ( 804.1105419155481968, -51.82724539060782121, 347.6308680596136469 ) ) ;
#3111 = CARTESIAN_POINT ( 'NONE',  ( 758.0580252608178853, -414.4527844766010389, -328.0187753319985404 ) ) ;
#3112 = CARTESIAN_POINT ( 'NONE',  ( 791.7608162188021197, 240.0000000000000853, -360.0000000000000000 ) ) ;
#3113 = FACE_OUTER_BOUND ( 'NONE', #38208, .T. ) ;
#3115 = CARTESIAN_POINT ( 'NONE',  ( 781.7834795799800531, -322.8164208402377540, 315.0636971347436202 ) ) ;
#3114 = CARTESIAN_POINT ( 'NONE',  ( 755.8398074228967971, -115.4419599262327409, 333.4516893846970333 ) ) ;
#3116 = ORIENTED_EDGE ( 'NONE', *, *, #41125, .T. ) ;
#3117 = CARTESIAN_POINT ( 'NONE',  ( 764.0069404352550464, -255.0783235625958980, -359.2566176426627180 ) ) ;
#3118 = CARTESIAN_POINT ( 'NONE',  ( 757.8323909638827445, -98.63460265842024910, 352.1044303154654358 ) ) ;
#3119 = CIRCLE ( 'NONE', #40733, 2.749999999999863665 ) ;
#3120 = CARTESIAN_POINT ( 'NONE',  ( 813.9316612368132837, -247.4419599262323004, -348.6739635108323228 ) ) ;
#3121 = FACE_OUTER_BOUND ( 'NONE', #37828, .T. ) ;
#3122 = CARTESIAN_POINT ( 'NONE',  ( 759.8311093483677041, -406.1692326535045368, 310.9282345327691814 ) ) ;
#3123 = VERTEX_POINT ( 'NONE', #20992 ) ;
#3124 = CARTESIAN_POINT ( 'NONE',  ( 754.8072714833581358, -292.8164208402376971, 338.1981804954720587 ) ) ;
#3125 = CARTESIAN_POINT ( 'NONE',  ( 783.0433043558608688, -48.89650538077840025, -315.1538015810313027 ) ) ;
#3126 = CARTESIAN_POINT ( 'NONE',  ( 771.1735550268778070, -153.1800572038746395, -316.3353852180827630 ) ) ;
#3127 = CARTESIAN_POINT ( 'NONE',  ( 765.0180583372156207, -216.9982390220562252, -360.0135310231089534 ) ) ;
#3128 = CARTESIAN_POINT ( 'NONE',  ( 800.2193346964447755, -402.9982390220555430, 355.1360043628815788 ) ) ;
#3129 = CARTESIAN_POINT ( 'NONE',  ( 772.5602148656447525, -105.7255117493293000, -305.7998596910095443 ) ) ;
#3130 = ADVANCED_FACE ( 'NONE', ( #27469 ), #31625, .F. ) ;
#3131 = CARTESIAN_POINT ( 'NONE',  ( 767.8955696845334842, -120.4527844766019768, -362.1676090361161755 ) ) ;
#3132 = ORIENTED_EDGE ( 'NONE', *, *, #28735, .F. ) ;
#3133 = CARTESIAN_POINT ( 'NONE',  ( 755.8894580844503253, -39.82724539060786384, -332.3691319403863531 ) ) ;
#3134 = CARTESIAN_POINT ( 'NONE',  ( 755.3028492785439312, -399.2817908451522726, -335.9200461376539693 ) ) ;
#3136 = CARTESIAN_POINT ( 'NONE',  ( 798.5707757039680246, -437.4636090269703459, 356.7845633553585003 ) ) ;
#3135 = CARTESIAN_POINT ( 'NONE',  ( 754.8072714833581358, -124.8164208402383508, 338.1981804954720587 ) ) ;
#3139 = CARTESIAN_POINT ( 'NONE',  ( 813.2346286133761168, -341.2601417444138292, 328.9521613784389160 ) ) ;
#3138 = LINE ( 'NONE', #38714, #14438 ) ;
#3137 = CARTESIAN_POINT ( 'NONE',  ( -208.8365100919714052, 256.5000000000001137, -202.7499999999925819 ) ) ;
#3140 = VERTEX_POINT ( 'NONE', #17553 ) ;
#3141 = CARTESIAN_POINT ( 'NONE',  ( 802.9823548866075953, -361.0999726633341425, -330.0799878456151077 ) ) ;
#3142 = CARTESIAN_POINT ( 'NONE',  ( 754.8072714833581358, -340.8164208402376971, -338.1981804954720587 ) ) ;
#3143 = AXIS2_PLACEMENT_3D ( 'NONE', #45436, #38276, #45669 ) ;
#3144 = CARTESIAN_POINT ( 'NONE',  ( 813.5763878283155464, -123.8272453906076009, -351.1614460488615350 ) ) ;
#3145 = CARTESIAN_POINT ( 'NONE',  ( 799.9636004259356241, -46.91815448151694312, 311.2241431872006956 ) ) ;
#3147 = DIRECTION ( 'NONE',  ( 0.000000000000000000, -1.000000000000000000, 0.000000000000000000 ) ) ;
#3146 = CYLINDRICAL_SURFACE ( 'NONE', #3469, 10.00000000000000888 ) ;
#3148 = CARTESIAN_POINT ( 'NONE',  ( 761.2382568024794409, -279.6237781080503737, -356.9571628226838129 ) ) ;
#3149 = CARTESIAN_POINT ( 'NONE',  ( 804.9363028652555840, -448.2709662947827951, -338.2165204200192079 ) ) ;
#3150 = CARTESIAN_POINT ( 'NONE',  ( 773.7305795820266212, -153.2817908451529831, -374.8230680027170365 ) ) ;
#3151 = PLANE ( 'NONE',  #34830 ) ;
#3152 = DIRECTION ( 'NONE',  ( -1.000000000000000000, -0.000000000000000000, -0.000000000000000000 ) ) ;
#3153 = CARTESIAN_POINT ( 'NONE',  ( 786.5483106153019435, -367.6454272087886466, 364.1601925771022366 ) ) ;
#3154 = CARTESIAN_POINT ( 'NONE',  ( 809.0717654672305343, -316.9181544815160692, 360.1688906516309885 ) ) ;
#3155 = CARTESIAN_POINT ( 'NONE',  ( 792.3570229623691148, -165.1800572038745543, -373.1304606946836770 ) ) ;
#3156 = EDGE_CURVE ( 'NONE', #29447, #23565, #7737, .T. ) ;
#3157 = DIRECTION ( 'NONE',  ( -1.000000000000000000, -0.000000000000000000, -0.000000000000000000 ) ) ;
#3158 = CARTESIAN_POINT ( 'NONE',  ( 795.8262568251477660, -118.3726999360621619, 308.3538107759623585 ) ) ;
#3159 = CARTESIAN_POINT ( 'NONE',  ( 754.9967657858570647, -289.5436935675103882, -365.0032342141425374 ) ) ;
#3160 = EDGE_CURVE ( 'NONE', #24078, #3360, #45503, .T. ) ;
#3161 = CARTESIAN_POINT ( 'NONE',  ( -468.8365100919714337, 240.0000000000001421, -202.7499999999907345 ) ) ;
#3162 = PLANE ( 'NONE',  #5755 ) ;
#3163 = CARTESIAN_POINT ( 'NONE',  ( 797.8594530101008786, -181.5436935675108145, 322.1405469898980982 ) ) ;
#3164 = ORIENTED_EDGE ( 'NONE', *, *, #27411, .F. ) ;
#3165 = CARTESIAN_POINT ( 'NONE',  ( 813.5763878283155464, -435.8272453906066062, 351.1614460488615350 ) ) ;
#3166 = CARTESIAN_POINT ( 'NONE',  ( 754.0944755984390895, -375.6237781080501463, -364.1009440267246760 ) ) ;
#3167 = CARTESIAN_POINT ( 'NONE',  ( 814.5518280994195948, -135.7255117493291152, -332.4837098697145734 ) ) ;
#3168 = CARTESIAN_POINT ( 'NONE',  ( 744.7301800767019131, -388.8164208402374129, -337.4774526936615757 ) ) ;
#3169 = DIRECTION ( 'NONE',  ( -1.000000000000000000, 0.000000000000000000, 0.000000000000000000 ) ) ;
#3170 = CARTESIAN_POINT ( 'NONE',  ( 773.7943932421234194, 0.1944037101305369775, 305.5313806188329409 ) ) ;
#3171 = VERTEX_POINT ( 'NONE', #6468 ) ;
#3172 = VECTOR ( 'NONE', #39419, 1000.000000000000000 ) ;
#3173 = CARTESIAN_POINT ( 'NONE',  ( 746.0683387631852383, -139.4419599262326699, -331.3260364891676204 ) ) ;
#3174 = DIRECTION ( 'NONE',  ( 0.000000000000000000, 0.000000000000000000, -1.000000000000000000 ) ) ;
#3175 = CARTESIAN_POINT ( 'NONE',  ( 810.1134526219336749, -320.5328690171411949, 357.8822607201570349 ) ) ;
#3176 = CARTESIAN_POINT ( 'NONE',  ( 800.2193346964446619, -114.9982390220565378, 355.1360043628816925 ) ) ;
#3177 = PRODUCT_DEFINITION_FORMATION_WITH_SPECIFIED_SOURCE ( 'ANY', '', #6326, .NOT_KNOWN. ) ;
#3178 = ORIENTED_EDGE ( 'NONE', *, *, #9445, .F. ) ;
#3179 = CARTESIAN_POINT ( 'NONE',  ( 759.7806653035534055, -294.9982390220560546, 324.8639956371180801 ) ) ;
#3180 = CARTESIAN_POINT ( 'NONE',  ( 796.7737145352015204, -20.63460265842048003, -370.7187646348536987 ) ) ;
#3181 = EDGE_CURVE ( 'NONE', #29825, #17451, #35755, .T. ) ;
#3182 = DIRECTION ( 'NONE',  ( -1.000000000000000000, 1.892425610156518354E-16, -0.000000000000000000 ) ) ;
#3183 = ORIENTED_EDGE ( 'NONE', *, *, #16214, .F. ) ;
#3184 = CARTESIAN_POINT ( 'NONE',  ( 791.9812246680005501, -188.6346026584199365, -361.9419747391813189 ) ) ;
#3185 = CARTESIAN_POINT ( 'NONE',  ( 750.9282345327678740, -424.9181544815158986, -319.8311093483690115 ) ) ;
#3186 = ORIENTED_EDGE ( 'NONE', *, *, #45316, .T. ) ;
#3187 = AXIS2_PLACEMENT_3D ( 'NONE', #13354, #45692, #3174 ) ;
#3188 = CARTESIAN_POINT ( 'NONE',  ( 801.9419747391806368, -18.45278447660230725, 351.9812246680014027 ) ) ;
#3189 = CARTESIAN_POINT ( 'NONE',  ( 767.8955696845333705, -264.4527844766016074, -362.1676090361162323 ) ) ;
#3191 = CARTESIAN_POINT ( 'NONE',  ( 778.7502325331095108, -264.3510508353232353, 304.6391490659818828 ) ) ;
#3190 = CARTESIAN_POINT ( 'NONE',  ( 814.5518280994195948, -375.7255117493284047, 332.4837098697145166 ) ) ;
#3192 = CARTESIAN_POINT ( 'NONE',  ( 802.9823548866075953, -241.0999726633345119, -330.0799878456151077 ) ) ;
#3193 = CARTESIAN_POINT ( 'NONE',  ( 755.5713283507202505, -269.3618753856924286, -334.6858677611754729 ) ) ;
#3194 = CARTESIAN_POINT ( 'NONE',  ( 778.1981804954715471, -442.2709662947827383, -314.8072714833591021 ) ) ;
#3195 = CARTESIAN_POINT ( 'NONE',  ( 788.7366044899766848, -83.90732993114754379, -316.5762568750059813 ) ) ;
#3196 = CARTESIAN_POINT ( 'NONE',  ( 804.4286716492782716, -257.3618753856924286, 345.3141322388244703 ) ) ;
#3197 = CARTESIAN_POINT ( 'NONE',  ( 751.9810565676468741, -386.0891481129647786, 360.9747183278973921 ) ) ;
#3198 = LINE ( 'NONE', #20529, #22575 ) ;
#3199 = CARTESIAN_POINT ( 'NONE',  ( 744.6391490659812007, -38.73633629969877035, -338.7502325331110455 ) ) ;
#3200 = FACE_BOUND ( 'NONE', #2636, .T. ) ;
#3201 = CARTESIAN_POINT ( 'NONE',  ( 786.4999999999993179, -544.8427095258973623, -369.9999999999999432 ) ) ;
#3202 = EDGE_CURVE ( 'NONE', #30680, #28948, #34290, .T. ) ;
#3203 = CARTESIAN_POINT ( 'NONE',  ( 763.0428371773158460, -227.4636090269709143, 358.7617431975195359 ) ) ;
#3204 = CARTESIAN_POINT ( 'NONE',  ( 804.6798772138708955, -135.7255117493291152, 334.6312213355107019 ) ) ;
#3205 = VERTEX_POINT ( 'NONE', #45260 ) ;
#3206 = CARTESIAN_POINT ( 'NONE',  ( 784.1219089521767955, 2.718209154846545683, -315.0488828828318333 ) ) ;
#3207 = CARTESIAN_POINT ( 'NONE',  ( 763.0537975583476964, -72.45278447660213317, -371.0346526505628617 ) ) ;
#3208 = VECTOR ( 'NONE', #4412, 1000.000000000000000 ) ;
#3209 = CARTESIAN_POINT ( 'NONE',  ( 784.0799538623451781, -299.8055962898685038, 364.6971507214555572 ) ) ;
#3210 = CARTESIAN_POINT ( 'NONE',  ( 764.8639956371174549, -416.0891481129645513, -319.7806653035542013 ) ) ;
#3211 = CARTESIAN_POINT ( 'NONE',  ( 755.8990559732751535, -11.46360902697159290, 365.9055244015606831 ) ) ;
#3212 = CARTESIAN_POINT ( 'NONE',  ( 814.2001403089898304, -209.3618753856926276, -347.4397851343538264 ) ) ;
#3213 = ADVANCED_FACE ( 'NONE', ( #13857 ), #44817, .F. ) ;
#3214 = CARTESIAN_POINT ( 'NONE',  ( 811.0346526505616112, -182.6346026584199649, 323.0537975583477532 ) ) ;
#3215 = CARTESIAN_POINT ( 'NONE',  ( 788.8264449731200330, -93.18005720387481006, 363.6646147819171233 ) ) ;
#3216 = CARTESIAN_POINT ( 'NONE',  ( 779.9999999999997726, 16.45630643248849267, 339.9999999999994884 ) ) ;
#3217 = CARTESIAN_POINT ( 'NONE',  ( 939.9999999999992042, 46.15097736693707020, -350.0000000000000000 ) ) ;
#3218 = CARTESIAN_POINT ( 'NONE',  ( 813.2346286133761168, -269.2601417444139997, -328.9521613784389160 ) ) ;
#3219 = CIRCLE ( 'NONE', #24604, 18.00000000000001421 ) ;
#3220 = CARTESIAN_POINT ( 'NONE',  ( 748.6759233522253680, -424.3726999360612808, 324.3348316497537098 ) ) ;
#3221 = CARTESIAN_POINT ( 'NONE',  ( 767.7687537140311633, -287.9073299311468759, -372.7932403749916830 ) ) ;
#3222 = LINE ( 'NONE', #31169, #16909 ) ;
#3223 = CARTESIAN_POINT ( 'NONE',  ( 754.9735926884551418, -378.3510508353227806, 340.5236548041000333 ) ) ;
#3224 = CARTESIAN_POINT ( 'NONE',  ( 796.9462024416508257, -60.45278447660216159, 308.9653473494370246 ) ) ;
#3225 = CARTESIAN_POINT ( 'NONE',  ( 800.2193346964447755, -402.9982390220555430, -355.1360043628815788 ) ) ;
#3226 = CARTESIAN_POINT ( 'NONE',  ( 804.9511171171677688, -5.805596289869448867, 335.8780910478229202 ) ) ;
#3227 = CARTESIAN_POINT ( 'NONE',  ( 781.8018195045266339, -190.2709662947835909, -365.1927285166406705 ) ) ;
#3228 = CARTESIAN_POINT ( 'NONE',  ( 812.6845335610512393, -55.98741447168748664, -353.5525998758768651 ) ) ;
#3229 = CARTESIAN_POINT ( 'NONE',  ( 775.9200461376533440, -191.8055962898689017, -315.3028492785443291 ) ) ;
#3230 = EDGE_CURVE ( 'NONE', #20750, #15194, #21736, .T. ) ;
#3231 = CARTESIAN_POINT ( 'NONE',  ( 752.4576283171824116, -165.0783235625962391, 317.7880784355627952 ) ) ;
#3232 = CARTESIAN_POINT ( 'NONE',  ( 767.8955696845334842, -24.45278447660228949, 362.1676090361161755 ) ) ;
#3233 = EDGE_CURVE ( 'NONE', #44752, #8827, #2530, .T. ) ;
#3234 = VERTEX_POINT ( 'NONE', #24684 ) ;
#3235 = CARTESIAN_POINT ( 'NONE',  ( 804.9363028652555840, -88.27096629478390355, -338.2165204200192079 ) ) ;
#3236 = CARTESIAN_POINT ( 'NONE',  ( 790.8726784830453198, -202.7146871989597514, -362.5472867521010585 ) ) ;
#3237 = CARTESIAN_POINT ( 'NONE',  ( 788.7366044899766848, -203.9073299311471885, 316.5762568750059813 ) ) ;
#3238 = CARTESIAN_POINT ( 'NONE',  ( 815.0009284576459549, -6.351050835323991173, -338.7629533639073429 ) ) ;
#3239 = CARTESIAN_POINT ( 'NONE',  ( 755.0636971347428243, -316.2709662947832499, 341.7834795799807353 ) ) ;
#3240 = VECTOR ( 'NONE', #38051, 1000.000000000000000 ) ;
#3241 = DIRECTION ( 'NONE',  ( 1.880165489482579047E-16, 1.000000000000000000, 0.000000000000000000 ) ) ;
#3242 = VECTOR ( 'NONE', #3579, 1000.000000000000000 ) ;
#3243 = EDGE_LOOP ( 'NONE', ( #545, #41841, #11943 ) ) ;
#3244 = CARTESIAN_POINT ( 'NONE',  ( 755.0488828828309806, -41.80559628986934229, 344.1219089521771934 ) ) ;
#3245 = CARTESIAN_POINT ( 'NONE',  ( 747.6481478633932056, -301.0999726633342561, -353.4146539503763620 ) ) ;
#3246 = CARTESIAN_POINT ( 'NONE',  ( 767.6429770376291799, -249.1800572038742700, 306.8695393053162093 ) ) ;
#3247 = CARTESIAN_POINT ( 'NONE',  ( 758.4439275373578084, -348.5545181178796383, 353.2243759319684386 ) ) ;
#3248 = CARTESIAN_POINT ( 'NONE',  ( 754.9735926884551418, -426.3510508353226669, 340.5236548041000333 ) ) ;
#3249 = CARTESIAN_POINT ( 'NONE',  ( 790.9844846989617508, -142.3726999360620766, -317.2208543904092721 ) ) ;
#3250 = CARTESIAN_POINT ( 'NONE',  ( 755.0636971347428243, -148.2709662947837330, -341.7834795799807353 ) ) ;
#3251 = CARTESIAN_POINT ( 'NONE',  ( 785.3687786644885591, -347.3618753856922012, -315.3201227861280813 ) ) ;
#3252 = ORIENTED_EDGE ( 'NONE', *, *, #8593, .T. ) ;
#3253 = CARTESIAN_POINT ( 'NONE',  ( 767.7687537140311633, -239.9073299311470748, 372.7932403749916830 ) ) ;
#3254 = CIRCLE ( 'NONE', #2490, 10.00000000000000888 ) ;
#3255 = EDGE_CURVE ( 'NONE', #5332, #39962, #34406, .T. ) ;
#3256 = CARTESIAN_POINT ( 'NONE',  ( 800.7704444035546203, -340.1692326535047641, 326.0291762391768771 ) ) ;
#3257 = CARTESIAN_POINT ( 'NONE',  ( 794.9999999999993179, 205.0000000000000568, 245.0000000000000284 ) ) ;
#3258 = EDGE_CURVE ( 'NONE', #37112, #36817, #13621, .T. ) ;
#3259 = CARTESIAN_POINT ( 'NONE',  ( 802.9823548866075953, -121.0999726633348956, 330.0799878456151077 ) ) ;
#3260 = CARTESIAN_POINT ( 'NONE',  ( 800.2193346964447755, -18.99823902205683979, 355.1360043628815788 ) ) ;
#3261 = ORIENTED_EDGE ( 'NONE', *, *, #14766, .F. ) ;
#3262 = CARTESIAN_POINT ( 'NONE',  ( 815.3608509340175488, -362.7363362996977116, -341.2497674668889545 ) ) ;
#3263 = DIRECTION ( 'NONE',  ( -1.000000000000000000, -0.000000000000000000, 0.000000000000000000 ) ) ;
#3264 = CARTESIAN_POINT ( 'NONE',  ( 748.6759233522253680, -232.3726999360617924, 324.3348316497537098 ) ) ;
#3265 = CARTESIAN_POINT ( 'NONE',  ( 796.7845633553578182, -177.6237781080507148, 358.5707757039688204 ) ) ;
#3266 = CARTESIAN_POINT ( 'NONE',  ( 802.1676090361156639, -326.6346026584193396, -327.8955696845344505 ) ) ;
#3267 = CARTESIAN_POINT ( 'NONE',  ( 804.6971507214547046, -219.2817908451527558, -344.0799538623459739 ) ) ;
#3268 = EDGE_CURVE ( 'NONE', #5854, #2789, #37873, .T. ) ;
#3269 = EDGE_CURVE ( 'NONE', #13352, #14381, #34673, .T. ) ;
#3270 = AXIS2_PLACEMENT_3D ( 'NONE', #10948, #20633, #307 ) ;
#3271 = CARTESIAN_POINT ( 'NONE',  ( 800.9747183278959710, -12.99823902205686821, 311.9810565676471583 ) ) ;
#3272 = CARTESIAN_POINT ( 'NONE',  ( 800.9747183278959710, -84.99823902205663728, 311.9810565676471583 ) ) ;
#3273 = CARTESIAN_POINT ( 'NONE',  ( 802.7276637122909051, -452.9681489794449476, 352.0069550970126784 ) ) ;
#3274 = CARTESIAN_POINT ( 'NONE',  ( 810.7187646348534145, -402.4527844766010389, -356.7737145352016341 ) ) ;
#3275 = AXIS2_PLACEMENT_3D ( 'NONE', #9976, #20811, #24047 ) ;
#3276 = DIRECTION ( 'NONE',  ( -0.000000000000000000, -0.000000000000000000, -1.000000000000000000 ) ) ;
#3277 = CARTESIAN_POINT ( 'NONE',  ( 766.4474001241216001, -355.0999726633341993, 307.3154664389482491 ) ) ;
#3278 = DIRECTION ( 'NONE',  ( 8.326672684688676025E-16, -1.000000000000000000, 0.000000000000000000 ) ) ;
#3279 = CARTESIAN_POINT ( 'NONE',  ( 812.7932403749906598, -279.1800572038741848, 327.7687537140311633 ) ) ;
#3280 = CARTESIAN_POINT ( 'NONE',  ( 777.5031285880264704, -46.81642084023858530, -374.9108240113588408 ) ) ;
#3281 = CARTESIAN_POINT ( 'NONE',  ( 756.5762568750052424, -291.1800572038741848, -348.7366044899774238 ) ) ;
#3282 = FACE_BOUND ( 'NONE', #18764, .T. ) ;
#3283 = CARTESIAN_POINT ( 'NONE',  ( 785.3141322388236176, -405.7255117493283478, 364.4286716492789537 ) ) ;
#3284 = CARTESIAN_POINT ( 'NONE',  ( 804.1105419155481968, -147.8272453906075157, 347.6308680596136469 ) ) ;
#3285 = CARTESIAN_POINT ( 'NONE',  ( 805.6418435158337843, -29.46360902697153250, -363.8556311672236916 ) ) ;
#3286 = CARTESIAN_POINT ( 'NONE',  ( 760.5453621957607311, -69.07832356259653750, -323.8424801807151425 ) ) ;
#3287 = CARTESIAN_POINT ( 'NONE',  ( 810.1134526219336749, -80.53286901714194812, 357.8822607201570349 ) ) ;
#3288 = CARTESIAN_POINT ( 'NONE',  ( 803.4237431249931660, -399.1800572038738437, 331.2633955100225194 ) ) ;
#3289 = DIRECTION ( 'NONE',  ( 0.000000000000000000, 0.000000000000000000, -1.000000000000000000 ) ) ;
#3290 = CIRCLE ( 'NONE', #45331, 8.024999999999948841 ) ;
#3291 = CARTESIAN_POINT ( 'NONE',  ( 773.7943932421234194, -143.8055962898690154, 305.5313806188329409 ) ) ;
#3292 = CARTESIAN_POINT ( 'NONE',  ( 788.8264449731200330, -429.1800572038737869, 363.6646147819171233 ) ) ;
#3293 = ORIENTED_EDGE ( 'NONE', *, *, #27744, .F. ) ;
#3294 = CARTESIAN_POINT ( 'NONE',  ( 802.1676090361156639, -62.63460265842031305, -327.8955696845344505 ) ) ;
#3295 = CIRCLE ( 'NONE', #4026, 9.999999999999980460 ) ;
#3296 = CARTESIAN_POINT ( 'NONE',  ( 759.2295555964440155, -352.1692326535046504, -353.9708237608231229 ) ) ;
#3298 = CARTESIAN_POINT ( 'NONE',  ( 800.0135310231082713, -206.0891481129653471, 325.0180583372163028 ) ) ;
#3297 = CARTESIAN_POINT ( 'NONE',  ( 754.8072714833581358, -220.8164208402379529, 338.1981804954720587 ) ) ;
#3299 = ORIENTED_EDGE ( 'NONE', *, *, #19907, .F. ) ;
#3300 = CARTESIAN_POINT ( 'NONE',  ( 756.1443688327750579, -405.6237781080500326, -314.3581564841659315 ) ) ;
#3301 = FACE_OUTER_BOUND ( 'NONE', #15485, .T. ) ;
#3302 = ORIENTED_EDGE ( 'NONE', *, *, #40695, .T. ) ;
#3303 = CARTESIAN_POINT ( 'NONE',  ( 797.6776695296629214, -403.5436935675101608, 357.6776695296636603 ) ) ;
#3304 = EDGE_LOOP ( 'NONE', ( #13111, #25405, #11101, #40410 ) ) ;
#3305 =( NAMED_UNIT ( * ) PLANE_ANGLE_UNIT ( ) SI_UNIT ( $, .RADIAN. ) );
#3306 = CARTESIAN_POINT ( 'NONE',  ( 792.2312462859673587, -251.9073299311470748, -307.2067596250082602 ) ) ;
#3307 = CARTESIAN_POINT ( 'NONE',  ( 763.0537975583476964, -144.4527844766018632, 371.0346526505628617 ) ) ;
#3308 = ORIENTED_EDGE ( 'NONE', *, *, #36589, .T. ) ;
#3309 = CARTESIAN_POINT ( 'NONE',  ( 748.3538107759620743, -184.7146871989598083, 355.8262568251490165 ) ) ;
#3310 = CARTESIAN_POINT ( 'NONE',  ( 805.1927285166399315, -208.8164208402380666, -341.8018195045277707 ) ) ;
#3311 = AXIS2_PLACEMENT_3D ( 'NONE', #15950, #12699, #30032 ) ;
#3312 = ORIENTED_EDGE ( 'NONE', *, *, #8604, .F. ) ;
#3313 = CARTESIAN_POINT ( 'NONE',  ( 778.1981804954714335, -370.2709662947831362, -314.8072714833589885 ) ) ;
#3314 = CARTESIAN_POINT ( 'NONE',  ( 795.1360043628807261, -20.08914811296592973, -360.2193346964456282 ) ) ;
#3315 = AXIS2_PLACEMENT_3D ( 'NONE', #45042, #34639, #16633 ) ;
#3316 = EDGE_CURVE ( 'NONE', #28329, #4120, #38339, .T. ) ;
#3317 = CARTESIAN_POINT ( 'NONE',  ( 794.1144889064781864, -226.1692326535051052, 360.9840315886528401 ) ) ;
#3318 = DIRECTION ( 'NONE',  ( -0.000000000000000000, 1.000000000000000000, -0.000000000000000000 ) ) ;
#3319 = DIRECTION ( 'NONE',  ( 0.000000000000000000, 0.000000000000000000, -1.000000000000000000 ) ) ;
#3320 = MANIFOLD_SOLID_BREP ( 'Cut-Extrude8', #6229 ) ;
#3321 = EDGE_LOOP ( 'NONE', ( #37502, #19598 ) ) ;
#3322 = CARTESIAN_POINT ( 'NONE',  ( 793.0897708529556667, -462.5545181178792973, -361.3366627262616362 ) ) ;
#3323 = DIRECTION ( 'NONE',  ( 0.000000000000000000, 0.000000000000000000, 1.000000000000000000 ) ) ;
#3324 = DIRECTION ( 'NONE',  ( -0.000000000000000000, -1.110223024625155554E-15, -1.000000000000000000 ) ) ;
#3325 = EDGE_LOOP ( 'NONE', ( #12467, #24130 ) ) ;
#3326 = CARTESIAN_POINT ( 'NONE',  ( 754.3581564841646241, -257.4636090269708575, -316.1443688327762516 ) ) ;
#3327 = CIRCLE ( 'NONE', #20980, 6.118999999999985562 ) ;
#3328 = CARTESIAN_POINT ( 'NONE',  ( 745.7194118038753459, -133.6454272087893571, 348.7631598425976449 ) ) ;
#3329 = VECTOR ( 'NONE', #38752, 999.9999999999998863 ) ;
#3331 = CARTESIAN_POINT ( 'NONE',  ( 800.2193346964447755, -234.9982390220561683, -355.1360043628815788 ) ) ;
#3330 = DIRECTION ( 'NONE',  ( -1.000000000000000000, 0.000000000000000000, 0.000000000000000000 ) ) ;
#3332 = CARTESIAN_POINT ( 'NONE',  ( 758.6633372737375112, -404.5328690171409107, -326.9102291470432533 ) ) ;
#3333 = DIRECTION ( 'NONE',  ( 1.000000000000000000, 0.000000000000000000, -0.000000000000000000 ) ) ;
#3334 = CARTESIAN_POINT ( 'NONE',  ( -728.8365100919714905, 260.0000000000001705, -208.0249999999890349 ) ) ;
#3335 = CARTESIAN_POINT ( 'NONE',  ( 804.4086373105744769, -121.6454272087894282, -333.3843516231986541 ) ) ;
#3336 = CIRCLE ( 'NONE', #30589, 2.749999999999919176 ) ;
#3337 = AXIS2_PLACEMENT_3D ( 'NONE', #41849, #38377, #14122 ) ;
#3338 = CARTESIAN_POINT ( 'NONE',  ( 748.6759233522253680, -376.3726999360614514, 324.3348316497537098 ) ) ;
#3339 = DIRECTION ( 'NONE',  ( 0.000000000000000000, 1.000000000000000000, 0.000000000000000000 ) ) ;
#3340 = CARTESIAN_POINT ( 'NONE',  ( 786.2056067578752163, 12.19440371013049784, -374.4686193811670023 ) ) ;
#3341 = CARTESIAN_POINT ( 'NONE',  ( 813.1304606946831655, -305.9073299311468190, -352.3570229623691716 ) ) ;
#3342 =( NAMED_UNIT ( * ) PLANE_ANGLE_UNIT ( ) SI_UNIT ( $, .RADIAN. ) );
#3343 = CARTESIAN_POINT ( 'NONE',  ( 180.7583438952260622, 239.9999999999991473, -244.9999999999999716 ) ) ;
#3344 = CARTESIAN_POINT ( 'NONE',  ( 785.3687786644884454, -83.36187538569296862, -315.3201227861279676 ) ) ;
#3345 = CARTESIAN_POINT ( 'NONE',  ( 752.7379699480933368, -252.0090635724254184, 361.9858362298580232 ) ) ;
#3346 = CARTESIAN_POINT ( 'NONE',  ( 788.7631598425961101, -217.4419599262324141, -305.7194118038759143 ) ) ;
#3347 = CARTESIAN_POINT ( 'NONE',  ( 792.2312462859673587, -179.9073299311472454, 307.2067596250082602 ) ) ;
#3348 = CARTESIAN_POINT ( 'NONE',  ( 782.5225473063381969, -430.2709662947827383, -375.2698199232970637 ) ) ;
#3349 = CARTESIAN_POINT ( 'NONE',  ( 779.9999999999992042, -462.9681489794448339, -339.9999999999999432 ) ) ;
#3350 = AXIS2_PLACEMENT_3D ( 'NONE', #35593, #3969, #7913 ) ;
#3351 = CARTESIAN_POINT ( 'NONE',  ( 794.9819416627830151, -300.9982390220559409, 319.9864689768909898 ) ) ;
#3352 = AXIS2_PLACEMENT_3D ( 'NONE', #10849, #17778, #32078 ) ;
#3353 = CARTESIAN_POINT ( 'NONE',  ( 802.5472867521000353, -76.37269993606228979, 350.8726784830461156 ) ) ;
#3354 = CARTESIAN_POINT ( 'NONE',  ( 762.1405469898971887, -433.5436935675099903, -357.8594530101015607 ) ) ;
#3355 = CIRCLE ( 'NONE', #43885, 30.00000000000008171 ) ;
#3356 = DIRECTION ( 'NONE',  ( 0.000000000000000000, 0.000000000000000000, 1.000000000000000000 ) ) ;
#3357 = CARTESIAN_POINT ( 'NONE',  ( -722.7175100919714623, 256.5000000000001705, -199.9999999999890861 ) ) ;
#3359 = CARTESIAN_POINT ( 'NONE',  ( 757.8323909638827445, -314.6346026584194533, 352.1044303154654358 ) ) ;
#3358 = CARTESIAN_POINT ( 'NONE',  ( 755.0488828828309806, -137.8055962898690154, 344.1219089521771934 ) ) ;
#3360 = VERTEX_POINT ( 'NONE', #22140 ) ;
#3361 = CARTESIAN_POINT ( 'NONE',  ( 802.7791456095903868, -268.7146871989595525, -329.0155153010375102 ) ) ;
#3362 = CARTESIAN_POINT ( 'NONE',  ( 755.5713283507202505, -77.36187538569302546, 334.6858677611754729 ) ) ;
#3363 = CARTESIAN_POINT ( 'NONE',  ( 811.6461892240364477, -292.7146871989594956, -324.1737431748509835 ) ) ;
#3364 = DIRECTION ( 'NONE',  ( 0.000000000000000000, 0.000000000000000000, 1.000000000000000000 ) ) ;
#3365 = CARTESIAN_POINT ( 'NONE',  ( 761.9338519418445230, -398.5328690171409107, 370.4231160770881957 ) ) ;
#3366 = ORIENTED_EDGE ( 'NONE', *, *, #17368, .F. ) ;
#3367 = CARTESIAN_POINT ( 'NONE',  ( 768.0187753319979720, -296.6346026584195670, 318.0580252608186242 ) ) ;
#3368 = AXIS2_PLACEMENT_3D ( 'NONE', #34752, #23660, #44938 ) ;
#3369 = CARTESIAN_POINT ( 'NONE',  ( 763.2154366446407039, -45.62377810805114109, -321.4292242960311228 ) ) ;
#3370 = CARTESIAN_POINT ( 'NONE',  ( 771.1735550268778070, -177.1800572038744690, -316.3353852180827630 ) ) ;
#3371 = CARTESIAN_POINT ( 'NONE',  ( 774.6858677611749044, -201.7255117493290015, -315.5713283507209894 ) ) ;
#3372 = CARTESIAN_POINT ( 'NONE',  ( 805.1927285166397041, -400.8164208402373561, 341.8018195045277707 ) ) ;
#3373 = AXIS2_PLACEMENT_3D ( 'NONE', #20882, #23659, #3356 ) ;
#3374 = CARTESIAN_POINT ( 'NONE',  ( 800.9747183278959710, -108.9982390220565804, -311.9810565676471583 ) ) ;
#3375 = CARTESIAN_POINT ( 'NONE',  ( 759.9864689768902508, -122.0891481129656171, -354.9819416627836404 ) ) ;
#3376 = ORIENTED_EDGE ( 'NONE', *, *, #23841, .T. ) ;
#3377 = CARTESIAN_POINT ( 'NONE',  ( 754.7162404726377645, -398.7363362996976548, -339.4709603349214717 ) ) ;
#3379 = CARTESIAN_POINT ( 'NONE',  ( 776.9254006560222479, -428.1908817542430938, 314.8983024940802125 ) ) ;
#3378 = CARTESIAN_POINT ( 'NONE',  ( 757.8323909638827445, -122.6346026584201354, 352.1044303154654358 ) ) ;
#3380 = CARTESIAN_POINT ( 'NONE',  ( 793.2243759319678702, -122.5328690171417918, 318.4439275373583200 ) ) ;
#3383 = CARTESIAN_POINT ( 'NONE',  ( 746.0683387631852383, -355.4419599262319593, 331.3260364891676204 ) ) ;
#3382 = CYLINDRICAL_SURFACE ( 'NONE', #23994, 10.00000000000000888 ) ;
#3381 = LINE ( 'NONE', #6608, #24751 ) ;
#3384 = ORIENTED_EDGE ( 'NONE', *, *, #14831, .F. ) ;
#3385 = CARTESIAN_POINT ( 'NONE',  ( 773.4516893846965786, -355.6454272087887603, -315.8398074228977066 ) ) ;
#3386 = CARTESIAN_POINT ( 'NONE',  ( 800.2193346964447755, -354.9982390220557704, -355.1360043628815788 ) ) ;
#3387 = CARTESIAN_POINT ( 'NONE',  ( 773.7305795820266212, -153.2817908451529831, -374.8230680027170365 ) ) ;
#3388 = EDGE_CURVE ( 'NONE', #10815, #22607, #39504, .T. ) ;
#3389 = CIRCLE ( 'NONE', #44586, 30.00000000000008171 ) ;
#3390 = CARTESIAN_POINT ( 'NONE',  ( 745.7194118038753459, -37.64542720878968396, 348.7631598425976449 ) ) ;
#3391 = VECTOR ( 'NONE', #32469, 999.9999999999998863 ) ;
#3393 = DIRECTION ( 'NONE',  ( -0.000000000000000000, 1.000000000000000000, -0.000000000000000000 ) ) ;
#3392 = CYLINDRICAL_SURFACE ( 'NONE', #42536, 2.749999999999835687 ) ;
#3394 = CARTESIAN_POINT ( 'NONE',  ( 804.6798772138708955, -447.7255117493280636, -334.6312213355107019 ) ) ;
#3395 = CARTESIAN_POINT ( 'NONE',  ( 810.4231160770870019, -144.5545181178802636, -321.9338519418446936 ) ) ;
#3396 = LINE ( 'NONE', #20922, #2018 ) ;
#3397 = DIRECTION ( 'NONE',  ( 1.000000000000000000, 0.000000000000000000, 0.000000000000000000 ) ) ;
#3398 = CARTESIAN_POINT ( 'NONE',  ( 804.4086373105744769, -361.6454272087887603, 333.3843516231986541 ) ) ;
#3399 = CARTESIAN_POINT ( 'NONE',  ( 746.4236121716829757, -327.8272453906069472, 328.8385539511384650 ) ) ;
#3400 = CARTESIAN_POINT ( 'NONE',  ( 808.0189434323515343, -206.0891481129653471, -319.0252816721025511 ) ) ;
#3401 = DIRECTION ( 'NONE',  ( -1.000000000000000000, 0.000000000000000000, 0.000000000000000000 ) ) ;
#3402 = CARTESIAN_POINT ( 'NONE',  ( 810.4231160770870019, -144.5545181178802636, 321.9338519418446936 ) ) ;
#3403 = CARTESIAN_POINT ( 'NONE',  ( 804.7487373415286811, -331.5436935675104451, -364.7487373415288516 ) ) ;
#3404 = VECTOR ( 'NONE', #7997, 1000.000000000000000 ) ;
#3405 = DIRECTION ( 'NONE',  ( -0.7071067811857625340, 8.659560562345319848E-17, 0.7071067811873326114 ) ) ;
#3406 = LINE ( 'NONE', #41291, #31582 ) ;
#3407 = CARTESIAN_POINT ( 'NONE',  ( 785.3141322388236176, -189.7255117493290300, 364.4286716492789537 ) ) ;
#3408 = EDGE_LOOP ( 'NONE', ( #13481, #19468, #22043, #26306 ) ) ;
#3409 = CARTESIAN_POINT ( 'NONE',  ( 778.7629533639073998, -416.7363362996975980, 375.0009284576466371 ) ) ;
#3410 = CARTESIAN_POINT ( 'NONE',  ( 813.2346286133761168, -389.2601417444136018, -328.9521613784389160 ) ) ;
#3411 = CARTESIAN_POINT ( 'NONE',  ( 751.6929314249748586, -126.9982390220565094, -318.8095938919659034 ) ) ;
#3412 = CARTESIAN_POINT ( 'NONE',  ( 745.0891759886404770, -436.2709662947827951, -342.4968714119734159 ) ) ;
#3413 = FACE_OUTER_BOUND ( 'NONE', #849, .T. ) ;
#3414 = CARTESIAN_POINT ( 'NONE',  ( 815.0009284576459549, 17.64894916467593688, 338.7629533639073429 ) ) ;
#3415 = VERTEX_POINT ( 'NONE', #14308 ) ;
#3416 = CARTESIAN_POINT ( 'NONE',  ( 752.4576283171824116, -165.0783235625962391, -317.7880784355627952 ) ) ;
#3417 = CARTESIAN_POINT ( 'NONE',  ( 744.8212110874229666, -306.8965053807775689, 336.2046728542121627 ) ) ;
#3418 = CARTESIAN_POINT ( 'NONE',  ( 781.7834795799800531, -106.8164208402383935, 315.0636971347436202 ) ) ;
#3419 = ORIENTED_EDGE ( 'NONE', *, *, #32569, .F. ) ;
#3420 = CIRCLE ( 'NONE', #15201, 20.00000000000001776 ) ;
#3421 = CARTESIAN_POINT ( 'NONE',  ( 767.8955696845333705, -144.4527844766018632, -362.1676090361162323 ) ) ;
#3422 = CARTESIAN_POINT ( 'NONE',  ( 788.7366044899766848, -299.9073299311468759, 316.5762568750059813 ) ) ;
#3423 = CARTESIAN_POINT ( 'NONE',  ( 749.2812353651451076, -6.452784476602343666, -323.2262854647983090 ) ) ;
#3424 = CARTESIAN_POINT ( 'NONE',  ( 999.9999999999992042, -599.5857864376268935, -359.5857864376268935 ) ) ;
#3425 = ORIENTED_EDGE ( 'NONE', *, *, #40263, .F. ) ;
#3426 = CARTESIAN_POINT ( 'NONE',  ( 802.2119215644370342, -414.0090635724249637, -367.5423716828165084 ) ) ;
#3427 = VERTEX_POINT ( 'NONE', #29080 ) ;
#3428 = CARTESIAN_POINT ( 'NONE',  ( 794.9819416627830151, -12.99823902205686821, 319.9864689768909898 ) ) ;
#3429 = CARTESIAN_POINT ( 'NONE',  ( 757.8323909638827445, -266.6346026584197375, -352.1044303154654358 ) ) ;
#3430 = AXIS2_PLACEMENT_3D ( 'NONE', #8557, #4189, #19171 ) ;
#3432 = CARTESIAN_POINT ( 'NONE',  ( 788.7631598425961101, -241.4419599262322720, 305.7194118038759143 ) ) ;
#3431 = CARTESIAN_POINT ( 'NONE',  ( 763.0537975583476964, -360.4527844766011526, 371.0346526505628617 ) ) ;
#3433 = CARTESIAN_POINT ( 'NONE',  ( 795.6651683502461765, -58.71468719896019905, 371.3240766477733814 ) ) ;
#3434 = CARTESIAN_POINT ( 'NONE',  ( 787.5531968255692163, -261.8272453906071746, -316.1348686366205811 ) ) ;
#3435 = CARTESIAN_POINT ( 'NONE',  ( 803.4237431249931660, -255.1800572038742700, -331.2633955100225194 ) ) ;
#3436 = CARTESIAN_POINT ( 'NONE',  ( 800.2193346964446619, -450.9982390220554294, -355.1360043628816925 ) ) ;
#3437 = CARTESIAN_POINT ( 'NONE',  ( 771.2633955100217236, -119.9073299311474443, -363.4237431249939618 ) ) ;
#3438 = CARTESIAN_POINT ( 'NONE',  ( 771.1735550268778070, -249.1800572038742416, 316.3353852180827630 ) ) ;
#3439 = EDGE_LOOP ( 'NONE', ( #17422, #16149, #26248, #25911 ) ) ;
#3440 = CARTESIAN_POINT ( 'NONE',  ( 782.5225473063381969, -382.2709662947828519, 375.2698199232970637 ) ) ;
#3441 = CARTESIAN_POINT ( 'NONE',  ( 831.1634899080286232, 256.4999999999998863, -197.2500000000000284 ) ) ;
#3442 = CARTESIAN_POINT ( 'NONE',  ( 786.2694204179717872, -45.28179084515329578, -305.1769319972829067 ) ) ;
#3443 = CARTESIAN_POINT ( 'NONE',  ( -858.8365100919713768, 258.0940000000002215, -193.8809999999881768 ) ) ;
#3444 = DIRECTION ( 'NONE',  ( -1.000000000000000000, -0.000000000000000000, 0.000000000000000000 ) ) ;
#3445 = CARTESIAN_POINT ( 'NONE',  ( 798.5707757039680246, -269.4636090269708006, 356.7845633553585003 ) ) ;
#3446 = CARTESIAN_POINT ( 'NONE',  ( 755.5713283507202505, -101.3618753856929544, 334.6858677611754729 ) ) ;
#3447 = EDGE_LOOP ( 'NONE', ( #7412, #17344 ) ) ;
#3448 = CARTESIAN_POINT ( 'NONE',  ( 758.4439275373578084, -12.55451811788067751, -353.2243759319684386 ) ) ;
#3449 = CARTESIAN_POINT ( 'NONE',  ( 811.0346526505617248, -110.6346026584201923, -323.0537975583478101 ) ) ;
#3450 = CARTESIAN_POINT ( 'NONE',  ( 770.0799878456142551, -277.9874144716867477, 362.9823548866085616 ) ) ;
#3451 = AXIS2_PLACEMENT_3D ( 'NONE', #42334, #21326, #31709 ) ;
#3452 = DIRECTION ( 'NONE',  ( -0.000000000000000000, -0.000000000000000000, 1.000000000000000000 ) ) ;
#3453 = CARTESIAN_POINT ( 'NONE',  ( 781.2370466360911223, 3.263663700301089765, 304.9990715423533629 ) ) ;
#3455 = VECTOR ( 'NONE', #31937, 1000.000000000000000 ) ;
#3454 = CARTESIAN_POINT ( 'NONE',  ( 792.3570229623688874, -189.1800572038744122, -373.1304606946836202 ) ) ;
#3456 = CARTESIAN_POINT ( 'NONE',  ( 748.9653473494363425, -170.6346026584199649, 356.9462024416521331 ) ) ;
#3457 = CARTESIAN_POINT ( 'NONE',  ( 803.6646147819161570, -65.90732993114758642, 348.8264449731210561 ) ) ;
#3458 = AXIS2_PLACEMENT_3D ( 'NONE', #40138, #18451, #11058 ) ;
#3459 = DIRECTION ( 'NONE',  ( -0.000000000000000000, 0.000000000000000000, 1.000000000000000000 ) ) ;
#3460 = CARTESIAN_POINT ( 'NONE',  ( 754.0944755984390895, -255.6237781080504874, -364.1009440267246760 ) ) ;
#3461 = CIRCLE ( 'NONE', #25583, 6.118999999999985562 ) ;
#3462 = CARTESIAN_POINT ( 'NONE',  ( 745.1792804349281596, -446.1908817542429802, 343.7566961878542884 ) ) ;
#3463 = CARTESIAN_POINT ( 'NONE',  ( 813.1304606946830518, -329.9073299311467053, -352.3570229623690580 ) ) ;
#3464 = FACE_OUTER_BOUND ( 'NONE', #14443, .T. ) ;
#3465 = CARTESIAN_POINT ( 'NONE',  ( 799.4546378042377910, -345.0783235625956991, 356.1575198192848006 ) ) ;
#3466 = CARTESIAN_POINT ( 'NONE',  ( 808.0189434323515343, -38.08914811296587999, 319.0252816721025511 ) ) ;
#3467 = CARTESIAN_POINT ( 'NONE',  ( 814.8230680027162407, -29.80559628986937781, -333.7305795820267917 ) ) ;
#3468 = CARTESIAN_POINT ( 'NONE',  ( 804.9363028652555840, -376.2709662947829656, -338.2165204200192079 ) ) ;
#3469 = AXIS2_PLACEMENT_3D ( 'NONE', #144, #6618, #38485 ) ;
#3470 = CARTESIAN_POINT ( 'NONE',  ( 805.0264073115434940, -54.35105083532383219, 339.4763451958999099 ) ) ;
#3471 = CARTESIAN_POINT ( 'NONE',  ( 746.7653713866222915, -65.26014174441471027, -351.0478386215610271 ) ) ;
#3472 = CARTESIAN_POINT ( 'NONE',  ( 794.1144889064781864, -178.1692326535052473, -360.9840315886528401 ) ) ;
#3473 = CARTESIAN_POINT ( 'NONE',  ( 791.1614460488616487, -203.2601417444143124, 373.5763878283158874 ) ) ;
#3474 = CARTESIAN_POINT ( 'NONE',  ( 804.9363028652555840, -16.27096629478413092, 338.2165204200192079 ) ) ;
#3475 = ORIENTED_EDGE ( 'NONE', *, *, #35991, .F. ) ;
#3476 = CARTESIAN_POINT ( 'NONE',  ( 771.1735550268778070, -81.18005720387481006, -316.3353852180827630 ) ) ;
#3477 = CARTESIAN_POINT ( 'NONE',  ( 799.4546378042377910, -201.0783235625961254, -356.1575198192848006 ) ) ;
#3478 = CARTESIAN_POINT ( 'NONE',  ( 755.5713283507202505, -197.3618753856926560, 334.6858677611754729 ) ) ;
#3479 = EDGE_CURVE ( 'NONE', #34504, #21916, #14994, .T. ) ;
#3480 = CARTESIAN_POINT ( 'NONE',  ( 788.7631598425961101, -25.44195992623301450, -305.7194118038759143 ) ) ;
#3481 = CARTESIAN_POINT ( 'NONE',  ( 774.6312213355098493, -335.3618753856921444, 364.6798772138717482 ) ) ;
#3482 = PLANE ( 'NONE',  #17576 ) ;
#3483 = VERTEX_POINT ( 'NONE', #18684 ) ;
#3484 = CARTESIAN_POINT ( 'NONE',  ( 798.7617431975189675, -51.62377810805111267, 323.0428371773161871 ) ) ;
#3486 = AXIS2_PLACEMENT_3D ( 'NONE', #31839, #14303, #14077 ) ;
#3485 = CARTESIAN_POINT ( 'NONE',  ( 799.9636004259356241, -310.9181544815160123, -311.2241431872006956 ) ) ;
#3487 = AXIS2_PLACEMENT_3D ( 'NONE', #27406, #9632, #8946 ) ;
#3488 = EDGE_CURVE ( 'NONE', #26915, #40829, #16634, .T. ) ;
#3489 = CARTESIAN_POINT ( 'NONE',  ( 772.4837098697145166, -239.3618753856924855, 374.5518280994205611 ) ) ;
#3490 = CARTESIAN_POINT ( 'NONE',  ( 763.2154366446407039, -429.6237781080499190, 321.4292242960311228 ) ) ;
#3491 = CARTESIAN_POINT ( 'NONE',  ( 769.0155153010367712, -154.3726999360620198, -362.7791456095907279 ) ) ;
#3492 = CARTESIAN_POINT ( 'NONE',  ( 781.7834795799800531, -154.8164208402382371, -315.0636971347436202 ) ) ;
#3493 = CARTESIAN_POINT ( 'NONE',  ( 797.6776695296629214, -355.5436935675103882, -357.6776695296636603 ) ) ;
#3494 = EDGE_LOOP ( 'NONE', ( #1018, #39594 ) ) ;
#3495 = AXIS2_PLACEMENT_3D ( 'NONE', #13303, #23897, #38017 ) ;
#3496 = CARTESIAN_POINT ( 'NONE',  ( 745.7998596910086917, -293.3618753856923718, 332.5602148656461168 ) ) ;
#3497 = CARTESIAN_POINT ( 'NONE',  ( -786.4999999999993179, -110.5936016518799221, 750.6326042729449455 ) ) ;
#3498 = CARTESIAN_POINT ( 'NONE',  ( 755.0488828828309806, -329.8055962898683902, 344.1219089521771934 ) ) ;
#3499 = DIRECTION ( 'NONE',  ( 1.000000000000000000, 0.000000000000000000, -0.000000000000000000 ) ) ;
#3500 = AXIS2_PLACEMENT_3D ( 'NONE', #44971, #38722, #41966 ) ;
#3501 = CARTESIAN_POINT ( 'NONE',  ( 804.6971507214547046, -147.2817908451529547, 344.0799538623459739 ) ) ;
#3502 = CARTESIAN_POINT ( 'NONE',  ( 767.8955696845333705, -24.45278447660229304, 362.1676090361162323 ) ) ;
#3503 = ORIENTED_EDGE ( 'NONE', *, *, #13757, .T. ) ;
#3504 = CARTESIAN_POINT ( 'NONE',  ( 814.8207195650702488, -362.1908817542432644, -336.2433038121456548 ) ) ;
#3505 = DIRECTION ( 'NONE',  ( -0.000000000000000000, -1.000000000000000000, 0.000000000000000000 ) ) ;
#3506 = ADVANCED_FACE ( 'NONE', ( #35777 ), #24919, .F. ) ;
#3507 = CARTESIAN_POINT ( 'NONE',  ( 764.1737431748507561, -250.3726999360618208, 371.6461892240376415 ) ) ;
#3508 = CARTESIAN_POINT ( 'NONE',  ( 798.7617431975189675, -171.6237781080507432, 323.0428371773161871 ) ) ;
#3509 = CARTESIAN_POINT ( 'NONE',  ( 804.9363028652555840, -376.2709662947829656, -338.2165204200192079 ) ) ;
#3510 = ADVANCED_FACE ( 'NONE', ( #3911 ), #28380, .F. ) ;
#3511 = DIRECTION ( 'NONE',  ( 0.000000000000000000, 0.000000000000000000, -1.000000000000000000 ) ) ;
#3512 = CARTESIAN_POINT ( 'NONE',  ( 805.2837595273609850, -218.7363362996982232, -340.5290396650784714 ) ) ;
#3513 = CARTESIAN_POINT ( 'NONE',  ( 751.6929314249748586, -30.99823902205680071, 318.8095938919659034 ) ) ;
#3514 = EDGE_CURVE ( 'NONE', #6763, #11154, #36229, .T. ) ;
#3515 = CARTESIAN_POINT ( 'NONE',  ( 799.9999999999993179, 205.0000000000000568, 329.9999999999999432 ) ) ;
#3516 = CARTESIAN_POINT ( 'NONE',  ( 810.7187646348534145, -426.4527844766010389, -356.7737145352016341 ) ) ;
#3517 = DIRECTION ( 'NONE',  ( 0.000000000000000000, 0.000000000000000000, 1.000000000000000000 ) ) ;
#3518 = CARTESIAN_POINT ( 'NONE',  ( 815.3608509340175488, -362.7363362996977116, 341.2497674668889545 ) ) ;
#3519 = DIRECTION ( 'NONE',  ( 1.000000000000000000, 0.000000000000000000, 0.000000000000000000 ) ) ;
#3520 = CARTESIAN_POINT ( 'NONE',  ( 796.9462024416508257, -324.4527844766013231, 308.9653473494370246 ) ) ;
#3521 = CARTESIAN_POINT ( 'NONE',  ( 800.9747183278959710, -36.99823902205679360, -311.9810565676471583 ) ) ;
#3522 = CARTESIAN_POINT ( 'NONE',  ( 774.6858677611749044, -297.7255117493286889, -315.5713283507209894 ) ) ;
#3523 = FACE_OUTER_BOUND ( 'NONE', #33807, .T. ) ;
#3524 = CARTESIAN_POINT ( 'NONE',  ( 757.8323909638827445, -386.6346026584191691, 352.1044303154654358 ) ) ;
#3525 = CARTESIAN_POINT ( 'NONE',  ( 769.9779781133707957, -163.0999726633347677, 316.7813123517150871 ) ) ;
#3526 = CARTESIAN_POINT ( 'NONE',  ( 811.3240766477731540, -28.37269993606244967, -355.6651683502462902 ) ) ;
#3527 = CARTESIAN_POINT ( 'NONE',  ( 793.2243759319678702, -74.53286901714196233, -318.4439275373583200 ) ) ;
#3528 = CARTESIAN_POINT ( 'NONE',  ( 754.0944755984390895, -111.6237781080509279, 364.1009440267246760 ) ) ;
#3529 = CARTESIAN_POINT ( 'NONE',  ( 756.3353852180820240, -389.9073299311465917, 331.1735550268787733 ) ) ;
#3530 = AXIS2_PLACEMENT_3D ( 'NONE', #4233, #14156, #36304 ) ;
#3531 = CARTESIAN_POINT ( 'NONE',  ( 804.7487373415286811, 4.456306432488530866, 364.7487373415288516 ) ) ;
#3532 = EDGE_CURVE ( 'NONE', #35031, #33715, #11535, .T. ) ;
#3533 = CARTESIAN_POINT ( 'NONE',  ( -786.4999999999993179, -513.1383975375929367, -369.9999999999999432 ) ) ;
#3534 = CARTESIAN_POINT ( 'NONE',  ( 758.0141637701419768, -159.0783235625962391, 367.2620300519063790 ) ) ;
#3535 = CARTESIAN_POINT ( 'NONE',  ( 781.7834795799800531, 13.18357915976123174, -315.0636971347436202 ) ) ;
#3536 = VERTEX_POINT ( 'NONE', #11072 ) ;
#3537 = CARTESIAN_POINT ( 'NONE',  ( 801.9419747391806368, -66.45278447660216159, -351.9812246680014027 ) ) ;
#3538 = EDGE_CURVE ( 'NONE', #12793, #28817, #21458, .T. ) ;
#3539 = CARTESIAN_POINT ( 'NONE',  ( 769.1273215169530886, -382.7146871989591546, -317.4527132478988847 ) ) ;
#3541 = CARTESIAN_POINT ( 'NONE',  ( 765.0180583372156207, -216.9982390220562252, 360.0135310231089534 ) ) ;
#3540 = CARTESIAN_POINT ( 'NONE',  ( 756.3353852180819104, -221.9073299311470464, 331.1735550268788302 ) ) ;
#3542 = VERTEX_POINT ( 'NONE', #21927 ) ;
#3543 = CARTESIAN_POINT ( 'NONE',  ( 752.4576283171824116, -405.0783235625954148, -317.7880784355627952 ) ) ;
#3544 = CARTESIAN_POINT ( 'NONE',  ( 808.3070685750230950, 5.001760977943074948, 361.1904061080339261 ) ) ;
#3545 = PLANE ( 'NONE',  #24184 ) ;
#3546 = ORIENTED_EDGE ( 'NONE', *, *, #36022, .T. ) ;
#3547 = CARTESIAN_POINT ( 'NONE',  ( 788.7366044899766848, -443.9073299311464780, 316.5762568750059813 ) ) ;
#3548 = ORIENTED_EDGE ( 'NONE', *, *, #352, .T. ) ;
#3549 = EDGE_CURVE ( 'NONE', #39281, #38048, #37255, .T. ) ;
#3550 = ADVANCED_FACE ( 'NONE', ( #25617 ), #32324, .T. ) ;
#3551 = CARTESIAN_POINT ( 'NONE',  ( 745.0891759886404770, -244.2709662947834204, -342.4968714119734159 ) ) ;
#3552 = CARTESIAN_POINT ( 'NONE',  ( 811.0346526505617248, -158.6346026584200217, 323.0537975583478101 ) ) ;
#3553 = ORIENTED_EDGE ( 'NONE', *, *, #6505, .F. ) ;
#3554 = CARTESIAN_POINT ( 'NONE',  ( 745.1769319972822814, -185.8055962898689302, 346.2694204179732083 ) ) ;
#3555 = CARTESIAN_POINT ( 'NONE',  ( 800.0135310231082713, -230.0891481129652618, -325.0180583372163028 ) ) ;
#3556 = EDGE_LOOP ( 'NONE', ( #5524, #38328, #27108, #43854 ) ) ;
#3557 = CARTESIAN_POINT ( 'NONE',  ( 797.6776695296629214, -355.5436935675103882, -357.6776695296636603 ) ) ;
#3558 = CARTESIAN_POINT ( 'NONE',  ( 804.6798772138708955, -15.72551174932958951, -334.6312213355107019 ) ) ;
#3559 = CARTESIAN_POINT ( 'NONE',  ( 765.8855110935204493, -214.1692326535052189, 319.0159684113471599 ) ) ;
#3560 = CARTESIAN_POINT ( 'NONE',  ( -598.8365100919716042, 260.0000000000001705, -199.9999999999899671 ) ) ;
#3561 = DIRECTION ( 'NONE',  ( 1.000000000000000000, -0.000000000000000000, -0.000000000000000000 ) ) ;
#3562 = ORIENTED_EDGE ( 'NONE', *, *, #17880, .T. ) ;
#3563 = CARTESIAN_POINT ( 'NONE',  ( 797.6776695296629214, -19.54369356751139364, -357.6776695296636603 ) ) ;
#3564 = DIRECTION ( 'NONE',  ( -0.7071067811865697772, 0.000000000000000000, 0.7071067811865252573 ) ) ;
#3565 = DIRECTION ( 'NONE',  ( -0.000000000000000000, 1.110223024625155554E-15, 1.000000000000000000 ) ) ;
#3566 = VERTEX_POINT ( 'NONE', #36012 ) ;
#3567 = CARTESIAN_POINT ( 'NONE',  ( 745.1792804349281596, -278.1908817542434917, -343.7566961878542884 ) ) ;
#3568 = CARTESIAN_POINT ( 'NONE',  ( 809.0717654672305343, -148.9181544815166092, 360.1688906516309885 ) ) ;
#3569 = AXIS2_PLACEMENT_3D ( 'NONE', #27047, #27953, #42049 ) ;
#3571 = CARTESIAN_POINT ( 'NONE',  ( 774.6312213355099630, -239.3618753856924570, -364.6798772138717482 ) ) ;
#3570 = DIRECTION ( 'NONE',  ( 0.000000000000000000, 0.000000000000000000, -1.000000000000000000 ) ) ;
#3572 = CARTESIAN_POINT ( 'NONE',  ( 756.7813123517142913, -379.9874144716865203, -329.9779781133712504 ) ) ;
#3573 = EDGE_CURVE ( 'NONE', #13352, #40320, #25375, .T. ) ;
#3574 = FILL_AREA_STYLE_COLOUR ( '', #31175 ) ;
#3575 = CARTESIAN_POINT ( 'NONE',  ( 766.9102291470427417, -114.5545181178803631, -318.6633372737382501 ) ) ;
#3576 = DIRECTION ( 'NONE',  ( -1.000000000000000000, 0.000000000000000000, 0.000000000000000000 ) ) ;
#3577 = CARTESIAN_POINT ( 'NONE',  ( 761.9338519418445230, 9.467130982857780097, -370.4231160770881957 ) ) ;
#3578 = CARTESIAN_POINT ( 'NONE',  ( 758.8095938919644823, -320.0891481129648923, -311.6929314249762797 ) ) ;
#3579 = DIRECTION ( 'NONE',  ( -0.000000000000000000, 1.000000000000000000, -0.000000000000000000 ) ) ;
#3580 = FACE_OUTER_BOUND ( 'NONE', #40404, .T. ) ;
#3581 = CARTESIAN_POINT ( 'NONE',  ( 785.3141322388236176, -93.72551174932934259, -364.4286716492789537 ) ) ;
#3582 = CARTESIAN_POINT ( 'NONE',  ( 771.3260364891663130, -259.6454272087890445, 306.0683387631859773 ) ) ;
#3583 = CARTESIAN_POINT ( 'NONE',  ( 748.3538107759620743, -208.7146871989596946, -355.8262568251490165 ) ) ;
#3584 = CARTESIAN_POINT ( 'NONE',  ( 787.4397851343537695, -213.7255117493289731, 374.2001403089903988 ) ) ;
#3585 = CARTESIAN_POINT ( 'NONE',  ( 751.6929314249748586, -438.9982390220553157, -318.8095938919659034 ) ) ;
#3586 = CARTESIAN_POINT ( 'NONE',  ( 701.1634899080286232, 259.9999999999999432, -199.9999999999990337 ) ) ;
#3587 = CARTESIAN_POINT ( 'NONE',  ( 800.2193346964447755, -306.9982390220558273, 355.1360043628815788 ) ) ;
#3588 = CARTESIAN_POINT ( 'NONE',  ( 758.4439275373578084, -84.55451811788046257, 353.2243759319684386 ) ) ;
#3589 = CARTESIAN_POINT ( 'NONE',  ( 796.7845633553578182, 14.37622189194867417, -358.5707757039688204 ) ) ;
#3590 = DIRECTION ( 'NONE',  ( -1.000000000000000000, -0.000000000000000000, -0.000000000000000000 ) ) ;
#3591 = EDGE_CURVE ( 'NONE', #43844, #27381, #39729, .T. ) ;
#3592 = DIRECTION ( 'NONE',  ( 0.000000000000000000, 0.000000000000000000, -1.000000000000000000 ) ) ;
#3594 = CARTESIAN_POINT ( 'NONE',  ( 758.0580252608178853, -366.4527844766012095, 328.0187753319985404 ) ) ;
#3593 = CARTESIAN_POINT ( 'NONE',  ( 758.6633372737375112, -140.5328690171417634, 326.9102291470432533 ) ) ;
#3595 = ORIENTED_EDGE ( 'NONE', *, *, #14216, .F. ) ;
#3596 = CARTESIAN_POINT ( 'NONE',  ( 797.8594530101008786, -229.5436935675106440, -322.1405469898980982 ) ) ;
#3597 = EDGE_CURVE ( 'NONE', #2789, #10930, #41580, .T. ) ;
#3598 = CARTESIAN_POINT ( 'NONE',  ( 754.8983024940795303, -282.8965053807776258, -336.9254006560228163 ) ) ;
#3599 = CARTESIAN_POINT ( 'NONE',  ( 771.1735550268778070, -105.1800572038747248, 316.3353852180827630 ) ) ;
#3600 = CARTESIAN_POINT ( 'NONE',  ( 814.8230680027162407, -293.8055962898685607, -333.7305795820267917 ) ) ;
#3601 = CARTESIAN_POINT ( 'NONE',  ( -28.63011601220122415, -563.3203001761231690, -342.3463313526983143 ) ) ;
#3602 = CARTESIAN_POINT ( 'NONE',  ( 744.8212110874229666, -402.8965053807773415, 336.2046728542121627 ) ) ;
#3603 = VERTEX_POINT ( 'NONE', #12710 ) ;
#3604 = CARTESIAN_POINT ( 'NONE',  ( 759.7806653035534055, -318.9982390220557704, 324.8639956371180801 ) ) ;
#3605 = AXIS2_PLACEMENT_3D ( 'NONE', #14612, #17604, #28446 ) ;
#3606 = CARTESIAN_POINT ( 'NONE',  ( 766.7756240680305382, -38.53286901714206891, -361.5560724626415663 ) ) ;
#3607 = CARTESIAN_POINT ( 'NONE',  ( 756.3353852180819104, -197.9073299311472169, -331.1735550268788302 ) ) ;
#3608 = CARTESIAN_POINT ( 'NONE',  ( 764.8639956371174549, -416.0891481129645513, 319.7806653035542013 ) ) ;
#3609 = CARTESIAN_POINT ( 'NONE',  ( 808.3070685750230950, -138.9982390220563957, -361.1904061080339261 ) ) ;
#3610 = PRODUCT_DEFINITION ( 'UNKNOWN', '', #3177, #12551 ) ;
#3611 = CARTESIAN_POINT ( 'NONE',  ( 792.1044303154646968, -132.4527844766019200, -317.8323909638837677 ) ) ;
#3612 = VERTEX_POINT ( 'NONE', #23552 ) ;
#3613 = CARTESIAN_POINT ( 'NONE',  ( 804.1105419155481968, -387.8272453906067767, -347.6308680596136469 ) ) ;
#3614 = CARTESIAN_POINT ( 'NONE',  ( 761.4292242960306112, -449.4636090269702322, 323.2154366446414429 ) ) ;
#3615 = CARTESIAN_POINT ( 'NONE',  ( 780.5290396650775619, -108.3510508353236759, 365.2837595273619513 ) ) ;
#3618 = CARTESIAN_POINT ( 'NONE',  ( 761.9338519418445230, -374.5328690171410813, 370.4231160770881957 ) ) ;
#3617 = FACE_OUTER_BOUND ( 'NONE', #40533, .T. ) ;
#3616 = DIRECTION ( 'NONE',  ( 0.000000000000000000, 0.000000000000000000, 1.000000000000000000 ) ) ;
#3619 = ORIENTED_EDGE ( 'NONE', *, *, #13436, .F. ) ;
#3620 = CARTESIAN_POINT ( 'NONE',  ( 804.1105419155481968, -387.8272453906067767, -347.6308680596136469 ) ) ;
#3621 = CARTESIAN_POINT ( 'NONE',  ( 781.8018195045266339, -358.2709662947829088, -365.1927285166406705 ) ) ;
#3622 = CARTESIAN_POINT ( 'NONE',  ( 793.5525998758768083, -175.0999726633346825, -372.6845335610516941 ) ) ;
#3623 = CARTESIAN_POINT ( 'NONE',  ( 786.2694204179717872, -21.28179084515337749, 305.1769319972829067 ) ) ;
#3625 = PLANE ( 'NONE',  #4125 ) ;
#3624 = DIRECTION ( 'NONE',  ( -0.000000000000000000, -0.6438296778008192334, 0.7651688349527135946 ) ) ;
#3626 = CARTESIAN_POINT ( 'NONE',  ( 798.7617431975189675, -291.6237781080503169, -323.0428371773161871 ) ) ;
#3627 = CARTESIAN_POINT ( 'NONE',  ( 781.7834795799800531, -442.8164208402372992, -315.0636971347436202 ) ) ;
#3628 = CARTESIAN_POINT ( 'NONE',  ( 776.2046728542105711, -164.1908817542438612, -304.8212110874238761 ) ) ;
#3629 = CARTESIAN_POINT ( 'NONE',  ( 779.9999999999992042, 126.4563064324884465, 329.9999999999999432 ) ) ;
#3630 = DIRECTION ( 'NONE',  ( -0.000000000000000000, -0.000000000000000000, 1.000000000000000000 ) ) ;
#3631 = CARTESIAN_POINT ( 'NONE',  ( 796.9571628226829034, -359.4636090269705164, 321.2382568024804641 ) ) ;
#3632 = CARTESIAN_POINT ( 'NONE',  ( 788.6739635108323228, -343.6454272087887603, 373.9316612368139090 ) ) ;
#3633 = CARTESIAN_POINT ( 'NONE',  ( 787.4397851343537695, -213.7255117493289731, -374.2001403089903988 ) ) ;
#3634 = CARTESIAN_POINT ( 'NONE',  ( 799.9999999999993179, 205.0000000000000568, 339.9999999999999432 ) ) ;
#3635 = DIRECTION ( 'NONE',  ( -0.000000000000000000, 1.000000000000000000, -0.000000000000000000 ) ) ;
#3636 = VECTOR ( 'NONE', #9011, 1000.000000000000114 ) ;
#3637 = CARTESIAN_POINT ( 'NONE',  ( 805.6418435158337843, -149.4636090269711417, 363.8556311672236916 ) ) ;
#3638 = CARTESIAN_POINT ( 'NONE',  ( 761.9338519418445230, -110.5328690171418629, -370.4231160770881957 ) ) ;
#3639 = CARTESIAN_POINT ( 'NONE',  ( 747.2067596250078623, -75.18005720387485269, 352.2312462859687230 ) ) ;
#3640 = CARTESIAN_POINT ( 'NONE',  ( 763.0537975583475827, -336.4527844766012095, -371.0346526505627480 ) ) ;
#3641 = DIRECTION ( 'NONE',  ( 1.000000000000000000, 0.000000000000000000, -0.000000000000000000 ) ) ;
#3642 = CARTESIAN_POINT ( 'NONE',  ( -26.63011601220122060, -365.3551492539851893, -8.132432514707076621 ) ) ;
#3643 = CARTESIAN_POINT ( 'NONE',  ( 758.0580252608178853, -174.4527844766018063, 328.0187753319985404 ) ) ;
#3644 = CARTESIAN_POINT ( 'NONE',  ( 814.8207195650702488, -458.1908817542429802, 336.2433038121456548 ) ) ;
#3645 = CARTESIAN_POINT ( 'NONE',  ( 746.7653713866222915, -425.2601417444136018, -351.0478386215610271 ) ) ;
#3646 = CARTESIAN_POINT ( 'NONE',  ( 782.5225473063381969, -142.2709662947837330, -375.2698199232970637 ) ) ;
#3647 = CARTESIAN_POINT ( 'NONE',  ( 796.7737145352015204, -404.6346026584193396, -370.7187646348536987 ) ) ;
#3648 = LINE ( 'NONE', #7110, #17334 ) ;
#3649 = CARTESIAN_POINT ( 'NONE',  ( 810.1134526219336749, 15.46713098285775878, 357.8822607201570349 ) ) ;
#3650 = ORIENTED_EDGE ( 'NONE', *, *, #36433, .F. ) ;
#3651 = CARTESIAN_POINT ( 'NONE',  ( 768.8385539511368734, -191.2601417444143976, -306.4236121716840557 ) ) ;
#3652 = PRESENTATION_STYLE_ASSIGNMENT (( #24636 ) ) ;
#3653 = CARTESIAN_POINT ( 'NONE',  ( 814.8230680027162407, -317.8055962898684470, 333.7305795820267917 ) ) ;
#3654 = CARTESIAN_POINT ( 'NONE',  ( 803.4237431249931660, -111.1800572038747532, 331.2633955100225194 ) ) ;
#3655 = ORIENTED_EDGE ( 'NONE', *, *, #27411, .T. ) ;
#3656 = CARTESIAN_POINT ( 'NONE',  ( 756.5762568750052424, -315.1800572038740711, 348.7366044899774238 ) ) ;
#3657 = CARTESIAN_POINT ( 'NONE',  ( 758.8095938919642549, -56.08914811296580893, -311.6929314249763365 ) ) ;
#3658 = CARTESIAN_POINT ( 'NONE',  ( 814.2001403089898304, -89.36187538569299704, 347.4397851343538264 ) ) ;
#3659 = ORIENTED_EDGE ( 'NONE', *, *, #40850, .T. ) ;
#3660 = CARTESIAN_POINT ( 'NONE',  ( 744.6391490659812007, -446.7363362996975980, -338.7502325331110455 ) ) ;
#3661 = VECTOR ( 'NONE', #15436, 1000.000000000000000 ) ;
#3662 = EDGE_LOOP ( 'NONE', ( #22676, #3827, #31750, #2963 ) ) ;
#3663 = PRODUCT_CONTEXT ( 'NONE', #30200, 'mechanical' ) ;
#3664 = CARTESIAN_POINT ( 'NONE',  ( 791.9812246680005501, -20.63460265842048003, 361.9419747391813189 ) ) ;
#3665 = CARTESIAN_POINT ( 'NONE',  ( 755.3201227861273992, -267.7255117493286320, -345.3687786644892981 ) ) ;
#3667 = CARTESIAN_POINT ( 'NONE',  ( 776.2433038121456548, -300.8965053807775689, 374.8207195650711014 ) ) ;
#3666 = CARTESIAN_POINT ( 'NONE',  ( 747.2067596250078623, -363.1800572038739006, 352.2312462859687230 ) ) ;
#3668 = CARTESIAN_POINT ( 'NONE',  ( 807.5423716828161105, -57.07832356259658013, 362.2119215644372048 ) ) ;
#3669 = CARTESIAN_POINT ( 'NONE',  ( 793.9708237608222134, -262.9181544815162965, -319.2295555964448681 ) ) ;
#3670 = CARTESIAN_POINT ( 'NONE',  ( 762.3223304703356007, -247.5436935675106724, -322.3223304703362828 ) ) ;
#3671 = LINE ( 'NONE', #30417, #17960 ) ;
#3672 = CARTESIAN_POINT ( 'NONE',  ( 781.7834795799800531, -106.8164208402383935, -315.0636971347436202 ) ) ;
#3673 = CARTESIAN_POINT ( 'NONE',  ( 804.6798772138708955, -255.7255117493287742, 334.6312213355107019 ) ) ;
#3674 = CARTESIAN_POINT ( 'NONE',  ( 767.7687537140311633, -383.9073299311466485, 372.7932403749916830 ) ) ;
#3676 = CARTESIAN_POINT ( 'NONE',  ( 939.9999999999992042, 62.85347435602262323, 357.4246812887967621 ) ) ;
#3675 = DIRECTION ( 'NONE',  ( -1.000000000000000000, 0.000000000000000000, 0.000000000000000000 ) ) ;
#3677 = CARTESIAN_POINT ( 'NONE',  ( 745.1792804349281596, -62.19088175424416676, -343.7566961878542884 ) ) ;
#3678 = CARTESIAN_POINT ( 'NONE',  ( 521.6730038022808458, 199.9999999999999147, 350.0000000000000000 ) ) ;
#3679 = CARTESIAN_POINT ( 'NONE',  ( -728.8365100919714905, 260.0000000000001705, -206.1189999999890574 ) ) ;
#3680 = CARTESIAN_POINT ( 'NONE',  ( 760.7433823573367135, -252.0090635724254184, 355.9930595647440441 ) ) ;
#3681 = CARTESIAN_POINT ( 'NONE',  ( 800.2193346964447755, -114.9982390220565236, 355.1360043628815788 ) ) ;
#3682 = EDGE_LOOP ( 'NONE', ( #18165, #4144, #29968, #9995, #14865, #36556 ) ) ;
#3683 = CARTESIAN_POINT ( 'NONE',  ( 755.5913626894240451, -13.64542720878976390, -346.6156483768012890 ) ) ;
#3684 = CARTESIAN_POINT ( 'NONE',  ( 813.1304606946831655, -89.90732993114752958, -352.3570229623691716 ) ) ;
#3685 = CARTESIAN_POINT ( 'NONE',  ( 766.7756240680305382, -278.5328690171412518, 361.5560724626415663 ) ) ;
#3686 = DIRECTION ( 'NONE',  ( 1.000000000000000000, 4.625929269271485914E-16, 0.000000000000000000 ) ) ;
#3687 = CARTESIAN_POINT ( 'NONE',  ( 745.1792804349281596, -38.19088175424422360, 343.7566961878542884 ) ) ;
#3688 = CARTESIAN_POINT ( 'NONE',  ( 763.0537975583475827, -240.4527844766015221, -371.0346526505627480 ) ) ;
#3689 = CARTESIAN_POINT ( 'NONE',  ( 814.2001403089898304, -161.3618753856927697, 347.4397851343538264 ) ) ;
#3690 = CARTESIAN_POINT ( 'NONE',  ( 805.1927285166397041, -64.81642084023852135, 341.8018195045277707 ) ) ;
#3691 = CARTESIAN_POINT ( 'NONE',  ( 355.8971257818259915, 290.0000000000001137, -244.9999999999999716 ) ) ;
#3692 = CARTESIAN_POINT ( 'NONE',  ( 766.5853460496234675, -277.9874144716867477, -372.3518521366060554 ) ) ;
#3693 = CARTESIAN_POINT ( 'NONE',  ( 761.4292242960306112, 6.536390973028352924, 323.2154366446414429 ) ) ;
#3694 = CARTESIAN_POINT ( 'NONE',  ( 808.0189434323515343, -302.0891481129650629, -319.0252816721025511 ) ) ;
#3695 = FACE_BOUND ( 'NONE', #34718, .T. ) ;
#3696 = CARTESIAN_POINT ( 'NONE',  ( 758.6633372737375112, -356.5328690171410813, 326.9102291470432533 ) ) ;
#3697 = CARTESIAN_POINT ( 'NONE',  ( 745.4481719005789273, -51.72551174932947049, 347.5162901302853697 ) ) ;
#3698 = CARTESIAN_POINT ( 'NONE',  ( 801.9419747391806368, -378.4527844766011526, -351.9812246680014027 ) ) ;
#3699 = CARTESIAN_POINT ( 'NONE',  ( 789.9200121543843807, -49.98741447168749374, 317.0176451133914384 ) ) ;
#3700 = CARTESIAN_POINT ( 'NONE',  ( 788.7366044899766848, -203.9073299311471885, -316.5762568750059813 ) ) ;
#3701 = CARTESIAN_POINT ( 'NONE',  ( 814.8230680027162407, -101.8055962898691718, -333.7305795820267917 ) ) ;
#3702 = CARTESIAN_POINT ( 'NONE',  ( 773.7943932421234194, -191.8055962898689017, 305.5313806188329409 ) ) ;
#3703 = CARTESIAN_POINT ( 'NONE',  ( 762.3223304703356007, -31.54369356751135456, 322.3223304703362828 ) ) ;
#3704 = CARTESIAN_POINT ( 'NONE',  ( 787.6308680596127942, -371.2601417444136587, 364.1105419155492768 ) ) ;
#3705 = ORIENTED_EDGE ( 'NONE', *, *, #17646, .F. ) ;
#3706 = CARTESIAN_POINT ( 'NONE',  ( 765.8855110935204493, -214.1692326535052189, -319.0159684113471599 ) ) ;
#3707 = CARTESIAN_POINT ( 'NONE',  ( 804.4286716492782716, -209.3618753856926276, 345.3141322388244703 ) ) ;
#3708 = CARTESIAN_POINT ( 'NONE',  ( 744.8212110874229666, -42.89650538077842157, -336.2046728542121627 ) ) ;
#3709 = CARTESIAN_POINT ( 'NONE',  ( 792.1044303154646968, -324.4527844766013231, 317.8323909638837677 ) ) ;
#3710 = DIRECTION ( 'NONE',  ( 1.000000000000000000, 0.000000000000000000, 0.000000000000000000 ) ) ;
#3711 = ORIENTED_EDGE ( 'NONE', *, *, #37418, .F. ) ;
#3712 = CARTESIAN_POINT ( 'NONE',  ( 756.7813123517142913, -43.98741447168752217, 329.9779781133712504 ) ) ;
#3713 = CARTESIAN_POINT ( 'NONE',  ( 793.5525998758768083, -319.0999726633342561, -372.6845335610516941 ) ) ;
#3714 = CARTESIAN_POINT ( 'NONE',  ( 777.5031285880264704, -262.8164208402379245, 374.9108240113588408 ) ) ;
#3715 = CARTESIAN_POINT ( 'NONE',  ( 752.4576283171824116, 2.921676437403253779, 317.7880784355627952 ) ) ;
#3716 = CARTESIAN_POINT ( 'NONE',  ( 755.8894580844503253, -159.8272453906075157, -332.3691319403863531 ) ) ;
#3717 = CARTESIAN_POINT ( 'NONE',  ( 802.1676090361156639, -134.6346026584201070, -327.8955696845344505 ) ) ;
#3718 = CARTESIAN_POINT ( 'NONE',  ( 800.2193346964446619, -354.9982390220557136, -355.1360043628816925 ) ) ;
#3719 = ORIENTED_EDGE ( 'NONE', *, *, #24375, .T. ) ;
#3720 = CARTESIAN_POINT ( 'NONE',  ( 805.0032342141412300, -277.5436935675105019, 314.9967657858571783 ) ) ;
#3721 = DIRECTION ( 'NONE',  ( -0.000000000000000000, 1.000000000000000000, -0.000000000000000000 ) ) ;
#3722 = CARTESIAN_POINT ( 'NONE',  ( 799.4546378042377910, -345.0783235625956991, 356.1575198192848006 ) ) ;
#3723 = DIRECTION ( 'NONE',  ( 1.000000000000000000, 0.000000000000000000, 0.000000000000000000 ) ) ;
#3724 = CARTESIAN_POINT ( 'NONE',  ( 761.4292242960306112, -161.4636090269711133, 323.2154366446414429 ) ) ;
#3725 = CARTESIAN_POINT ( 'NONE',  ( 803.4237431249931660, -15.18005720387504631, 331.2633955100225194 ) ) ;
#3726 = ORIENTED_EDGE ( 'NONE', *, *, #27806, .F. ) ;
#3727 = CARTESIAN_POINT ( 'NONE',  ( 766.4474001241216001, -379.0999726633341993, -307.3154664389482491 ) ) ;
#3728 = CARTESIAN_POINT ( 'NONE',  ( 814.9108240113580450, -16.27096629478413092, -337.5031285880265273 ) ) ;
#3729 = CARTESIAN_POINT ( 'NONE',  ( 813.5763878283155464, -219.8272453906073167, 351.1614460488615350 ) ) ;
#3730 = CARTESIAN_POINT ( 'NONE',  ( 775.9200461376533440, -191.8055962898689017, 315.3028492785443291 ) ) ;
#3731 = CARTESIAN_POINT ( 'NONE',  ( 791.9812246680005501, -356.6346026584193964, -361.9419747391813189 ) ) ;
#3732 = CARTESIAN_POINT ( 'NONE',  ( 791.9460785601769430, -462.7578698805381237, 362.0383033825738721 ) ) ;
#3733 = PLANE ( 'NONE',  #1594 ) ;
#3734 = CARTESIAN_POINT ( 'NONE',  ( 780.5236548040995785, -236.7363362996981380, -314.9735926884559944 ) ) ;
#3735 = CARTESIAN_POINT ( 'NONE',  ( 763.0537975583475827, -0.4527844766023628176, 371.0346526505627480 ) ) ;
#3736 = CARTESIAN_POINT ( 'NONE',  ( 759.0252816721024374, -72.99823902205667991, 368.0189434323527280 ) ) ;
#3737 = FACE_OUTER_BOUND ( 'NONE', #34936, .T. ) ;
#3738 = CARTESIAN_POINT ( 'NONE',  ( 755.2512626584698410, -415.5436935675102177, -315.2512626584710915 ) ) ;
#3739 = CARTESIAN_POINT ( 'NONE',  ( 914.9999999999992042, 99.99999999999984368, -360.0000000000000000 ) ) ;
#3740 = CARTESIAN_POINT ( 'NONE',  ( 813.5763878283155464, -339.8272453906069472, 351.1614460488615350 ) ) ;
#3741 = CARTESIAN_POINT ( 'NONE',  ( -37.63011601220122770, -512.9681489794448908, -352.0000000000000000 ) ) ;
#3742 = CARTESIAN_POINT ( 'NONE',  ( 813.1304606946830518, -329.9073299311467053, 352.3570229623690580 ) ) ;
#3743 = CARTESIAN_POINT ( 'NONE',  ( 763.0537975583475827, -48.45278447660219712, -371.0346526505627480 ) ) ;
#3744 = ADVANCED_FACE ( 'NONE', ( #37655, #9262 ), #2308, .F. ) ;
#3745 = CARTESIAN_POINT ( 'NONE',  ( 797.8594530101008786, -277.5436935675105019, -322.1405469898980982 ) ) ;
#3746 = CARTESIAN_POINT ( 'NONE',  ( 799.9999999999993179, -512.9681489794448908, 339.9999999999999432 ) ) ;
#3747 = CARTESIAN_POINT ( 'NONE',  ( 795.1360043628807261, -428.0891481129644944, 360.2193346964456282 ) ) ;
#3748 = CARTESIAN_POINT ( 'NONE',  ( 763.0428371773158460, -203.4636090269709996, 358.7617431975195359 ) ) ;
#3749 = CARTESIAN_POINT ( 'NONE',  ( 745.1792804349281596, -38.19088175424422360, -343.7566961878542884 ) ) ;
#3750 = CARTESIAN_POINT ( 'NONE',  ( 765.8855110935204493, -70.16923265350563099, -319.0159684113471599 ) ) ;
#3751 = CARTESIAN_POINT ( 'NONE',  ( 752.4576283171824116, -117.0783235625963528, 317.7880784355627952 ) ) ;
#3752 = CARTESIAN_POINT ( 'NONE',  ( 792.1044303154646968, -396.4527844766010958, 317.8323909638837677 ) ) ;
#3753 = CARTESIAN_POINT ( 'NONE',  ( 771.1735550268778070, 14.81994279612486309, -316.3353852180827630 ) ) ;
#3754 = ORIENTED_EDGE ( 'NONE', *, *, #38002, .F. ) ;
#3755 = CARTESIAN_POINT ( 'NONE',  ( 788.7366044899766848, -107.9073299311474727, -316.5762568750059813 ) ) ;
#3756 = CARTESIAN_POINT ( 'NONE',  ( 795.9930595647434757, -387.0783235625955285, -320.7433823573372820 ) ) ;
#3758 = CARTESIAN_POINT ( 'NONE',  ( 805.1927285166399315, -208.8164208402380666, 341.8018195045277707 ) ) ;
#3757 = CARTESIAN_POINT ( 'NONE',  ( 791.9812246680005501, -236.6346026584198228, 361.9419747391813189 ) ) ;
#3759 = CARTESIAN_POINT ( 'NONE',  ( 783.7566961878529810, -408.8965053807772847, -305.1792804349288417 ) ) ;
#3760 = LINE ( 'NONE', #7240, #27889 ) ;
#3761 = ORIENTED_EDGE ( 'NONE', *, *, #25566, .T. ) ;
#3762 = CARTESIAN_POINT ( 'NONE',  ( 803.4237431249931660, -423.1800572038737300, 331.2633955100225194 ) ) ;
#3763 = ORIENTED_EDGE ( 'NONE', *, *, #42223, .T. ) ;
#3764 = SHAPE_REPRESENTATION_RELATIONSHIP ( 'NONE' , 'NONE' ,  #15645, #8939 ) ;
#3765 = CARTESIAN_POINT ( 'NONE',  ( 808.3070685750230950, -258.9982390220561115, -361.1904061080339261 ) ) ;
#3766 = CARTESIAN_POINT ( 'NONE',  ( 796.7737145352015204, -164.6346026584200217, 370.7187646348536987 ) ) ;
#3767 = CARTESIAN_POINT ( 'NONE',  ( 769.0155153010367712, -274.3726999360617356, 362.7791456095907279 ) ) ;
#3768 = ORIENTED_EDGE ( 'NONE', *, *, #28665, .F. ) ;
#3769 = CARTESIAN_POINT ( 'NONE',  ( 797.8594530101009923, -253.5436935675105588, -322.1405469898982119 ) ) ;
#3770 = ORIENTED_EDGE ( 'NONE', *, *, #22696, .F. ) ;
#3771 = CARTESIAN_POINT ( 'NONE',  ( 762.1405469898971887, -361.5436935675103882, -357.8594530101015607 ) ) ;
#3772 = CARTESIAN_POINT ( 'NONE',  ( 758.0580252608178853, -6.452784476602343666, -328.0187753319985404 ) ) ;
#3773 = CARTESIAN_POINT ( 'NONE',  ( 802.7791456095903868, -220.7146871989596661, 329.0155153010375102 ) ) ;
#3774 = DIRECTION ( 'NONE',  ( 0.000000000000000000, 0.000000000000000000, 1.000000000000000000 ) ) ;
#3775 = CYLINDRICAL_SURFACE ( 'NONE', #33686, 2.749999999999863665 ) ;
#3776 = ORIENTED_EDGE ( 'NONE', *, *, #45342, .T. ) ;
#3777 = CARTESIAN_POINT ( 'NONE',  ( 757.8323909638827445, -2.634602658420536869, -352.1044303154654358 ) ) ;
#3778 = FACE_OUTER_BOUND ( 'NONE', #39106, .T. ) ;
#3779 = CARTESIAN_POINT ( 'NONE',  ( 989.9999999999992042, 56.73212367640085318, 362.5753187112032379 ) ) ;
#3780 = ORIENTED_EDGE ( 'NONE', *, *, #3573, .F. ) ;
#3781 = CARTESIAN_POINT ( 'NONE',  ( 750.9282345327678740, -280.9181544815162965, -319.8311093483690115 ) ) ;
#3782 = CARTESIAN_POINT ( 'NONE',  ( 783.7953271457878373, -152.1908817542438612, 375.1787889125761239 ) ) ;
#3784 = CARTESIAN_POINT ( 'NONE',  ( 781.7834795799800531, -274.8164208402378108, -315.0636971347436202 ) ) ;
#3783 = PLANE ( 'NONE',  #13583 ) ;
#3785 = CARTESIAN_POINT ( 'NONE',  ( 784.0799538623451781, -395.8055962898682765, -364.6971507214555572 ) ) ;
#3786 =( BOUNDED_CURVE ( )  B_SPLINE_CURVE ( 2, ( #44669, #39067, #37967, #22, #482, #14343, #21489, #23851, #23626, #7414, #2626, #16725, #13029 ),
 .UNSPECIFIED., .F., .T. ) 
 B_SPLINE_CURVE_WITH_KNOTS ( ( 3, 2, 2, 2, 2, 2, 3 ),
 ( 0.000000000000000000, 0.0008527428137030668154, 0.003125470086430381933, 0.005398197359157586028, 0.007670924631884902013, 0.009943651904612216264, 0.01049328897333767253 ),
 .UNSPECIFIED. ) 
 CURVE ( )  GEOMETRIC_REPRESENTATION_ITEM ( )  RATIONAL_B_SPLINE_CURVE ( ( 0.4976140944542620792, 0.4980906878130254567, 0.5000002209606652093, 0.4949109396520706139, 0.5000002209606652093, 0.4949109396520706139, 0.5000002209606652093, 0.4949109396520706139, 0.5000002209606652093, 0.4949109396520706139, 0.5000002209606652093, 0.4987694275901001228, 0.4981339451206906466 ) ) 
 REPRESENTATION_ITEM ( '' )  );
#3787 = DIRECTION ( 'NONE',  ( 0.000000000000000000, -0.000000000000000000, -1.000000000000000000 ) ) ;
#3788 = CARTESIAN_POINT ( 'NONE',  ( 790.0220218866281812, -127.0999726633348672, -363.2186876482849129 ) ) ;
#3789 = EDGE_CURVE ( 'NONE', #44896, #39863, #40665, .T. ) ;
#3790 = CARTESIAN_POINT ( 'NONE',  ( 760.0363995740630116, -370.9181544815159555, 368.7758568127991907 ) ) ;
#3791 = FACE_BOUND ( 'NONE', #28122, .T. ) ;
#3792 = CARTESIAN_POINT ( 'NONE',  ( 810.1134526219336749, 15.46713098285775878, -357.8822607201570349 ) ) ;
#3793 = CARTESIAN_POINT ( 'NONE',  ( 767.6429770376291799, -321.1800572038740711, -306.8695393053162093 ) ) ;
#3794 = CARTESIAN_POINT ( 'NONE',  ( 791.9812246680005501, -20.63460265842048003, 361.9419747391813189 ) ) ;
#3795 = CARTESIAN_POINT ( 'NONE',  ( 815.3608509340175488, -266.7363362996981095, 341.2497674668889545 ) ) ;
#3796 = CARTESIAN_POINT ( 'NONE',  ( 746.7653713866222915, -185.2601417444143692, -351.0478386215610271 ) ) ;
#3797 = CARTESIAN_POINT ( 'NONE',  ( 808.0189434323515343, -230.0891481129652618, 319.0252816721025511 ) ) ;
#3798 = CARTESIAN_POINT ( 'NONE',  ( 799.9636004259356241, 1.081845518482914104, -311.2241431872006956 ) ) ;
#3799 = EDGE_CURVE ( 'NONE', #36535, #14349, #2609, .T. ) ;
#3800 = LINE ( 'NONE', #28968, #14383 ) ;
#3801 = CARTESIAN_POINT ( 'NONE',  ( 803.6646147819161570, -329.9073299311467053, 348.8264449731210561 ) ) ;
#3802 = CARTESIAN_POINT ( 'NONE',  ( 805.2837595273609850, -98.73633629969859271, 340.5290396650784714 ) ) ;
#3803 = CARTESIAN_POINT ( 'NONE',  ( 763.8424801807145741, -66.00906357242595845, 320.5453621957614700 ) ) ;
#3804 = CARTESIAN_POINT ( 'NONE',  ( 754.8983024940795303, 5.103494619221427442, -336.9254006560228163 ) ) ;
#3805 = DIRECTION ( 'NONE',  ( -0.000000000000000000, -0.000000000000000000, 1.000000000000000000 ) ) ;
#3806 = LINE ( 'NONE', #574, #29221 ) ;
#3808 = CARTESIAN_POINT ( 'NONE',  ( 785.3141322388236176, -357.7255117493285184, 364.4286716492789537 ) ) ;
#3807 = CARTESIAN_POINT ( 'NONE',  ( 756.1348686366196716, -113.2601417444145682, 347.5531968255698416 ) ) ;
#3809 = ORIENTED_EDGE ( 'NONE', *, *, #12744, .F. ) ;
#3810 = CARTESIAN_POINT ( 'NONE',  ( 755.8398074228967971, -307.4419599262320730, -333.4516893846970333 ) ) ;
#3811 = CARTESIAN_POINT ( 'NONE',  ( 785.3687786644884454, -107.3618753856928976, 315.3201227861279676 ) ) ;
#3812 = CARTESIAN_POINT ( 'NONE',  ( 803.8556311672234642, -297.6237781080502600, -365.6418435158340117 ) ) ;
#3813 = DIRECTION ( 'NONE',  ( -1.000000000000000000, 0.000000000000000000, 0.000000000000000000 ) ) ;
#3814 = CARTESIAN_POINT ( 'NONE',  ( 746.0683387631852383, -427.4419599262317888, 331.3260364891676204 ) ) ;
#3815 = EDGE_CURVE ( 'NONE', #31813, #29825, #6235, .T. ) ;
#3816 = VERTEX_POINT ( 'NONE', #6003 ) ;
#3817 = CARTESIAN_POINT ( 'NONE',  ( 756.3353852180819104, -317.9073299311468190, 331.1735550268788302 ) ) ;
#3818 = ADVANCED_FACE ( 'NONE', ( #40894 ), #12490, .F. ) ;
#3819 = CARTESIAN_POINT ( 'NONE',  ( 784.0799538623451781, -59.80559628986927834, -364.6971507214555572 ) ) ;
#3820 = CARTESIAN_POINT ( 'NONE',  ( 781.7834795799800531, -154.8164208402382371, -315.0636971347436202 ) ) ;
#3821 = CARTESIAN_POINT ( 'NONE',  ( 755.5713283507202505, -221.3618753856925707, -334.6858677611754729 ) ) ;
#3822 = CARTESIAN_POINT ( 'NONE',  ( 802.1676090361156639, -398.6346026584193396, 327.8955696845344505 ) ) ;
#3823 = CARTESIAN_POINT ( 'NONE',  ( 810.7187646348534145, -138.4527844766019200, -356.7737145352016341 ) ) ;
#3824 = VERTEX_POINT ( 'NONE', #23331 ) ;
#3825 = VECTOR ( 'NONE', #37918, 1000.000000000000000 ) ;
#3826 = CARTESIAN_POINT ( 'NONE',  ( 762.1405469898973024, -145.5436935675109851, -357.8594530101016176 ) ) ;
#3827 = ORIENTED_EDGE ( 'NONE', *, *, #13072, .F. ) ;
#3828 = CARTESIAN_POINT ( 'NONE',  ( 773.4516893846965786, -403.6454272087884760, -315.8398074228977066 ) ) ;
#3830 = CARTESIAN_POINT ( 'NONE',  ( 755.5913626894240451, -445.6454272087883055, 346.6156483768012890 ) ) ;
#3829 = CARTESIAN_POINT ( 'NONE',  ( 801.9419747391806368, -114.4527844766020053, 351.9812246680014027 ) ) ;
#3831 = CARTESIAN_POINT ( 'NONE',  ( 780.5290396650775619, -132.3510508353235764, 365.2837595273619513 ) ) ;
#3834 = CARTESIAN_POINT ( 'NONE',  ( 783.7566961878529810, -408.8965053807772847, 305.1792804349288417 ) ) ;
#3833 = DIRECTION ( 'NONE',  ( 0.000000000000000000, 0.000000000000000000, 1.000000000000000000 ) ) ;
#3832 = CARTESIAN_POINT ( 'NONE',  ( 939.9999999999993179, -590.0000000000001137, 209.9999999999999716 ) ) ;
#3835 = EDGE_LOOP ( 'NONE', ( #2476, #20852, #37122, #36881 ) ) ;
#3836 = CARTESIAN_POINT ( 'NONE',  ( 754.7162404726377645, -398.7363362996976548, -339.4709603349214717 ) ) ;
#3837 = CARTESIAN_POINT ( 'NONE',  ( -784.4999999999993179, -544.8427095258973623, -350.0000000000000000 ) ) ;
#3838 = CARTESIAN_POINT ( 'NONE',  ( 814.4686193811664907, -171.2817908451529263, -346.2056067578752732 ) ) ;
#3839 = CARTESIAN_POINT ( 'NONE',  ( 791.0478386215596629, -45.82724539060783542, 306.7653713866226326 ) ) ;
#3841 = CARTESIAN_POINT ( 'NONE',  ( 51.16348990802859475, 260.0000000000000568, -199.9999999999945146 ) ) ;
#3840 = CYLINDRICAL_SURFACE ( 'NONE', #29331, 2.749999999999863665 ) ;
#3842 = EDGE_CURVE ( 'NONE', #40829, #26915, #24728, .T. ) ;
#3843 = CARTESIAN_POINT ( 'NONE',  ( 804.9511171171677688, -293.8055962898685607, -335.8780910478229202 ) ) ;
#3844 = CYLINDRICAL_SURFACE ( 'NONE', #12912, 6.118999999999985562 ) ;
#3845 = CARTESIAN_POINT ( 'NONE',  ( 745.7194118038753459, -205.6454272087891297, -348.7631598425976449 ) ) ;
#3846 = CARTESIAN_POINT ( 'NONE',  ( 914.9999999999992042, 99.99999999999984368, -360.0000000000000000 ) ) ;
#3847 = CARTESIAN_POINT ( 'NONE',  ( -858.8365100919713768, 256.5000000000002274, -199.9999999999881481 ) ) ;
#3848 = CARTESIAN_POINT ( 'NONE',  ( 755.5913626894240451, -349.6454272087887603, 346.6156483768012890 ) ) ;
#3849 = EDGE_CURVE ( 'NONE', #20161, #21828, #36164, .T. ) ;
#3850 = CARTESIAN_POINT ( 'NONE',  ( 747.6481478633932056, -349.0999726633342561, 353.4146539503763620 ) ) ;
#3851 = CARTESIAN_POINT ( 'NONE',  ( 811.0346526505617248, -206.6346026584198796, -323.0537975583478101 ) ) ;
#3852 = CARTESIAN_POINT ( 'NONE',  ( 914.9999999999992042, 99.99999999999984368, -360.0000000000000000 ) ) ;
#3853 = CARTESIAN_POINT ( 'NONE',  ( 778.1981804954714335, 13.72903370521577138, -314.8072714833589885 ) ) ;
#3854 = CARTESIAN_POINT ( 'NONE',  ( 744.6391490659812007, -134.7363362996984790, 338.7502325331110455 ) ) ;
#3855 = CARTESIAN_POINT ( 'NONE',  ( 746.0683387631852383, -91.44195992623282621, -331.3260364891676204 ) ) ;
#3856 = CARTESIAN_POINT ( 'NONE',  ( 746.8695393053150156, -125.9073299311474159, 327.6429770376306010 ) ) ;
#3857 = CARTESIAN_POINT ( 'NONE',  ( 772.5602148656447525, -345.7255117493285184, -305.7998596910095443 ) ) ;
#3858 = ADVANCED_FACE ( 'NONE', ( #28917 ), #29596, .F. ) ;
#3859 = CARTESIAN_POINT ( 'NONE',  ( 914.9999999999992042, 99.99999999999984368, 360.0000000000000000 ) ) ;
#3860 = CARTESIAN_POINT ( 'NONE',  ( -784.4999999999993179, -365.3551492539851893, -18.13243251470705886 ) ) ;
#3861 = CARTESIAN_POINT ( 'NONE',  ( 800.2193346964447755, -186.9982390220563104, 355.1360043628815788 ) ) ;
#3862 = CIRCLE ( 'NONE', #2344, 6.118999999999985562 ) ;
#3863 = CARTESIAN_POINT ( 'NONE',  ( 763.8424801807145741, 5.990936427573807954, 320.5453621957614700 ) ) ;
#3864 = CARTESIAN_POINT ( 'NONE',  ( 808.7758568127978833, -412.1692326535045936, -320.0363995740631822 ) ) ;
#3865 = CARTESIAN_POINT ( 'NONE',  ( 792.2312462859673587, -419.9073299311465348, -307.2067596250082602 ) ) ;
#3866 = DIRECTION ( 'NONE',  ( 0.000000000000000000, 0.000000000000000000, -1.000000000000000000 ) ) ;
#3867 = CARTESIAN_POINT ( 'NONE',  ( 791.1614460488616487, -11.26014174441488258, 373.5763878283158874 ) ) ;
#3868 = ORIENTED_EDGE ( 'NONE', *, *, #1507, .F. ) ;
#3869 = CARTESIAN_POINT ( 'NONE',  ( 815.1787889125755555, -174.8965053807779952, -343.7953271457877804 ) ) ;
#3870 = CYLINDRICAL_SURFACE ( 'NONE', #3187, 9.999999999999980460 ) ;
#3871 = CARTESIAN_POINT ( 'NONE',  ( 803.8556311672234642, -321.6237781080502600, 365.6418435158340117 ) ) ;
#3872 = CARTESIAN_POINT ( 'NONE',  ( 804.4286716492782716, -137.3618753856928265, 345.3141322388244703 ) ) ;
#3873 = ORIENTED_EDGE ( 'NONE', *, *, #45007, .F. ) ;
#3874 = CARTESIAN_POINT ( 'NONE',  ( 762.3223304703356007, -319.5436935675104451, 322.3223304703362828 ) ) ;
#3875 = CARTESIAN_POINT ( 'NONE',  ( 745.0891759886404770, -52.27096629478401724, -342.4968714119734159 ) ) ;
#3876 = VECTOR ( 'NONE', #8066, 1000.000000000000000 ) ;
#3877 = CARTESIAN_POINT ( 'NONE',  ( 748.9653473494365699, -74.63460265842030594, 356.9462024416520762 ) ) ;
#3878 = ORIENTED_EDGE ( 'NONE', *, *, #26405, .T. ) ;
#3879 = CARTESIAN_POINT ( 'NONE',  ( 788.6739635108323228, -439.6454272087884760, -373.9316612368139090 ) ) ;
#3880 = ORIENTED_EDGE ( 'NONE', *, *, #12353, .F. ) ;
#3881 = PRODUCT_CONTEXT ( 'NONE', #32571, 'mechanical' ) ;
#3882 = CARTESIAN_POINT ( 'NONE',  ( 788.7366044899766848, -35.90732993114770011, 316.5762568750059813 ) ) ;
#3883 = CARTESIAN_POINT ( 'NONE',  ( 756.3353852180819104, -293.9073299311468759, -331.1735550268788302 ) ) ;
#3885 = CARTESIAN_POINT ( 'NONE',  ( 795.6651683502461765, -274.7146871989594388, 371.3240766477733814 ) ) ;
#3884 = CARTESIAN_POINT ( 'NONE',  ( 767.6429770376291799, -393.1800572038737869, 306.8695393053162093 ) ) ;
#3886 = CARTESIAN_POINT ( 'NONE',  ( 811.6461892240364477, -76.71468719896012090, 324.1737431748509835 ) ) ;
#3887 = CARTESIAN_POINT ( 'NONE',  ( 766.0291762391763086, -298.9181544815161828, -360.7704444035551319 ) ) ;
#3888 = CARTESIAN_POINT ( 'NONE',  ( 767.8955696845333705, -264.4527844766016074, -362.1676090361162323 ) ) ;
#3889 = CARTESIAN_POINT ( 'NONE',  ( 949.5497976682736407, 229.9999999999998579, -210.0000000000000000 ) ) ;
#3890 = CARTESIAN_POINT ( 'NONE',  ( 762.3223304703356007, -127.5436935675110561, -322.3223304703362828 ) ) ;
#3891 = DIRECTION ( 'NONE',  ( 0.000000000000000000, 0.000000000000000000, 1.000000000000000000 ) ) ;
#3892 = ORIENTED_EDGE ( 'NONE', *, *, #42510, .F. ) ;
#3893 = CARTESIAN_POINT ( 'NONE',  ( 787.4397851343537695, -405.7255117493283478, 374.2001403089903988 ) ) ;
#3895 = CARTESIAN_POINT ( 'NONE',  ( 799.9999999999993179, 205.0000000000000568, 350.0000000000000000 ) ) ;
#3894 = CARTESIAN_POINT ( 'NONE',  ( -829.9999999999994316, 579.9999999999998863, -360.0000000000000000 ) ) ;
#3896 = CARTESIAN_POINT ( 'NONE',  ( 814.2805881961230625, -73.64542720878957027, -331.2368401574024119 ) ) ;
#3897 = CARTESIAN_POINT ( 'NONE',  ( 799.9999999999993179, -512.9681489794448908, 339.9999999999999432 ) ) ;
#3898 = FACE_OUTER_BOUND ( 'NONE', #20408, .T. ) ;
#3899 = CARTESIAN_POINT ( 'NONE',  ( 766.0291762391763086, -250.9181544815163534, 360.7704444035551319 ) ) ;
#3900 = CARTESIAN_POINT ( 'NONE',  ( 781.8018195045266339, -166.2709662947835909, 365.1927285166406705 ) ) ;
#3901 = ORIENTED_EDGE ( 'NONE', *, *, #6862, .T. ) ;
#3902 = CARTESIAN_POINT ( 'NONE',  ( 763.8424801807145741, -42.00906357242603661, -320.5453621957614700 ) ) ;
#3903 = CARTESIAN_POINT ( 'NONE',  ( 814.5518280994195948, -111.7255117493292857, -332.4837098697145166 ) ) ;
#3904 = CARTESIAN_POINT ( 'NONE',  ( 759.2295555964440155, -328.1692326535048210, 353.9708237608231229 ) ) ;
#3905 = FACE_BOUND ( 'NONE', #1345, .T. ) ;
#3906 = CARTESIAN_POINT ( 'NONE',  ( 754.3581564841646241, -41.46360902697149697, 316.1443688327762516 ) ) ;
#3907 = CARTESIAN_POINT ( 'NONE',  ( 745.0891759886404770, -220.2709662947834772, -342.4968714119734159 ) ) ;
#3908 = CARTESIAN_POINT ( 'NONE',  ( 787.4397851343537695, -213.7255117493289731, 374.2001403089903988 ) ) ;
#3909 = CARTESIAN_POINT ( 'NONE',  ( 791.9812246680005501, -68.63460265842033436, 361.9419747391813189 ) ) ;
#3910 = VECTOR ( 'NONE', #13045, 1000.000000000000000 ) ;
#3911 = FACE_OUTER_BOUND ( 'NONE', #37370, .T. ) ;
#3912 = CARTESIAN_POINT ( 'NONE',  ( 814.8230680027162407, -317.8055962898684470, -333.7305795820267917 ) ) ;
#3913 = AXIS2_PLACEMENT_3D ( 'NONE', #2322, #20110, #16193 ) ;
#3914 = CARTESIAN_POINT ( 'NONE',  ( 812.3518521366052028, -457.0999726633339151, 326.5853460496235243 ) ) ;
#3915 = CARTESIAN_POINT ( 'NONE',  ( 796.7737145352015204, -308.6346026584195670, -370.7187646348536987 ) ) ;
#3916 = CARTESIAN_POINT ( 'NONE',  ( 786.6156483768007774, -361.4419599262319593, 315.5913626894246136 ) ) ;
#3917 = CARTESIAN_POINT ( 'NONE',  ( 782.4968714119720516, -58.81642084023854267, 305.0891759886411023 ) ) ;
#3918 = CARTESIAN_POINT ( 'NONE',  ( 767.8955696845333705, -384.4527844766011526, -362.1676090361162323 ) ) ;
#3919 = CARTESIAN_POINT ( 'NONE',  ( 763.2154366446407039, -69.62377810805107003, 321.4292242960311228 ) ) ;
#3920 = CARTESIAN_POINT ( 'NONE',  ( 800.0135310231082713, -206.0891481129653471, -325.0180583372163028 ) ) ;
#3921 = CARTESIAN_POINT ( 'NONE',  ( 783.7566961878529810, -96.89650538077825104, -305.1792804349288417 ) ) ;
#3922 = CARTESIAN_POINT ( 'NONE',  ( 801.9858362298568863, -219.0783235625960401, 312.7379699480935642 ) ) ;
#3923 = CARTESIAN_POINT ( 'NONE',  ( 771.1735550268780344, -33.18005720387498769, 316.3353852180828198 ) ) ;
#3924 = ORIENTED_EDGE ( 'NONE', *, *, #9203, .T. ) ;
#3925 = CARTESIAN_POINT ( 'NONE',  ( 803.8651313633788504, -197.2601417444143124, -332.4468031744301015 ) ) ;
#3926 = CARTESIAN_POINT ( 'NONE',  ( 774.6312213355099630, -215.3618753856925423, 364.6798772138717482 ) ) ;
#3927 = CARTESIAN_POINT ( 'NONE',  ( 814.8230680027162407, -29.80559628986937781, -333.7305795820267917 ) ) ;
#3928 = CARTESIAN_POINT ( 'NONE',  ( 771.2633955100217236, -335.9073299311468190, 363.4237431249939618 ) ) ;
#3929 = CARTESIAN_POINT ( 'NONE',  ( 791.7608162188021197, 205.0000000000000568, -319.9999999999999432 ) ) ;
#3930 = CARTESIAN_POINT ( 'NONE',  ( 758.7867965644026071, 16.45630643248849267, 318.7867965644036303 ) ) ;
#3931 = ORIENTED_EDGE ( 'NONE', *, *, #3789, .F. ) ;
#3932 = CARTESIAN_POINT ( 'NONE',  ( 787.6308680596127942, -59.26014174441473870, 364.1105419155492768 ) ) ;
#3933 = CARTESIAN_POINT ( 'NONE',  ( 771.3260364891663130, -331.6454272087888171, -306.0683387631859773 ) ) ;
#3934 = CARTESIAN_POINT ( 'NONE',  ( 782.4968714119720516, -298.8164208402377540, 305.0891759886411023 ) ) ;
#3935 = CARTESIAN_POINT ( 'NONE',  ( 751.2241431872005251, 7.830767346494148740, 359.9636004259367610 ) ) ;
#3936 = CARTESIAN_POINT ( 'NONE',  ( 798.5707757039680246, -173.4636090269710849, -356.7845633553585003 ) ) ;
#3937 = CARTESIAN_POINT ( 'NONE',  ( 794.9819416627830151, -156.9982390220564241, -319.9864689768909898 ) ) ;
#3938 = VECTOR ( 'NONE', #20737, 1000.000000000000000 ) ;
#3939 = CARTESIAN_POINT ( 'NONE',  ( 754.8072714833583632, -340.8164208402376403, -338.1981804954721156 ) ) ;
#3940 = EDGE_LOOP ( 'NONE', ( #39481, #22505 ) ) ;
#3941 = VECTOR ( 'NONE', #43200, 1000.000000000000000 ) ;
#3942 = CARTESIAN_POINT ( 'NONE',  ( 751.9810565676468741, -290.0891481129650629, 360.9747183278973921 ) ) ;
#3943 = CARTESIAN_POINT ( 'NONE',  ( 311.1634899080286232, 229.9999999999999716, -202.7499999999961915 ) ) ;
#3944 = CARTESIAN_POINT ( 'NONE',  ( 794.1144889064781864, -346.1692326535047641, 360.9840315886528401 ) ) ;
#3945 = DIRECTION ( 'NONE',  ( -1.880165489482579047E-16, -1.000000000000000000, 0.000000000000000000 ) ) ;
#3946 = CARTESIAN_POINT ( 'NONE',  ( 779.4763451958990572, -152.7363362996983938, 365.0264073115438919 ) ) ;
#3947 = CARTESIAN_POINT ( 'NONE',  ( 754.8072714833581358, -28.81642084023863148, 338.1981804954720587 ) ) ;
#3948 = EDGE_LOOP ( 'NONE', ( #23305, #31638 ) ) ;
#3949 = CARTESIAN_POINT ( 'NONE',  ( 795.8262568251477660, -382.3726999360613945, -308.3538107759623585 ) ) ;
#3950 = ADVANCED_FACE ( 'NONE', ( #22875 ), #36966, .T. ) ;
#3951 = CARTESIAN_POINT ( 'NONE',  ( 808.0189434323515343, 9.910851887033969021, -319.0252816721025511 ) ) ;
#3952 = ADVANCED_BREP_SHAPE_REPRESENTATION ( '', ( #31868, #26858 ), #29006 ) ;
#3953 = CARTESIAN_POINT ( 'NONE',  ( 771.3260364891663130, -283.6454272087889308, 306.0683387631859773 ) ) ;
#3954 = CARTESIAN_POINT ( 'NONE',  ( 776.9566956441375396, -204.8965053807779100, 364.8461984189686405 ) ) ;
#3955 = CARTESIAN_POINT ( 'NONE',  ( 756.5762568750052424, -363.1800572038739006, -348.7366044899774238 ) ) ;
#3956 = CARTESIAN_POINT ( 'NONE',  ( 762.3223304703356007, 16.45630643248849267, 322.3223304703362828 ) ) ;
#3957 = DIRECTION ( 'NONE',  ( 1.000000000000000000, 0.000000000000000000, 0.000000000000000000 ) ) ;
#3958 = CARTESIAN_POINT ( 'NONE',  ( 766.9102291470427417, -234.5545181178799794, -318.6633372737382501 ) ) ;
#3959 = CARTESIAN_POINT ( 'NONE',  ( 772.4837098697144029, 0.6381246143067236254, 374.5518280994205611 ) ) ;
#3960 = CARTESIAN_POINT ( 'NONE',  ( 814.5518280994195948, -87.72551174932937101, 332.4837098697145734 ) ) ;
#3961 = DIRECTION ( 'NONE',  ( 1.000000000000000000, -0.000000000000000000, -0.000000000000000000 ) ) ;
#3962 = CARTESIAN_POINT ( 'NONE',  ( 814.9108240113580450, -400.2709662947828519, -337.5031285880265273 ) ) ;
#3963 = LINE ( 'NONE', #21507, #30562 ) ;
#3964 = CARTESIAN_POINT ( 'NONE',  ( 757.7880784355613741, -354.0090635724250774, 312.4576283171834916 ) ) ;
#3965 = CARTESIAN_POINT ( 'NONE',  ( 786.4999999999993179, -544.8427095258973623, -369.9999999999999432 ) ) ;
#3966 = CARTESIAN_POINT ( 'NONE',  ( 745.0891759886404770, -316.2709662947832499, 342.4968714119734159 ) ) ;
#3967 = CARTESIAN_POINT ( 'NONE',  ( 808.3070685750230950, -66.99823902205672255, -361.1904061080339261 ) ) ;
#3968 = CARTESIAN_POINT ( 'NONE',  ( 771.1735550268778070, -273.1800572038742985, -316.3353852180827630 ) ) ;
#3969 = DIRECTION ( 'NONE',  ( 4.147566128926363633E-16, 1.000000000000000000, -0.000000000000000000 ) ) ;
#3970 = CARTESIAN_POINT ( 'NONE',  ( 756.3353852180819104, -437.9073299311463074, 331.1735550268788302 ) ) ;
#3971 = CIRCLE ( 'NONE', #15055, 2.749999999999919176 ) ;
#3972 = CARTESIAN_POINT ( 'NONE',  ( 786.5483106153019435, -199.6454272087891582, 364.1601925771022366 ) ) ;
#3973 = CARTESIAN_POINT ( 'NONE',  ( 766.4474001241216001, -67.09997266333506616, -307.3154664389482491 ) ) ;
#3974 = CARTESIAN_POINT ( 'NONE',  ( 780.5290396650775619, -84.35105083532374692, -365.2837595273619513 ) ) ;
#3975 = CARTESIAN_POINT ( 'NONE',  ( 813.9316612368132837, -103.4419599262327836, 348.6739635108323228 ) ) ;
#3976 = CARTESIAN_POINT ( 'NONE',  ( 794.9819416627830151, -420.9982390220555999, 319.9864689768909898 ) ) ;
#3977 = CARTESIAN_POINT ( 'NONE',  ( 756.5762568750052424, -3.180057203875080063, -348.7366044899774238 ) ) ;
#3978 = ORIENTED_EDGE ( 'NONE', *, *, #6649, .F. ) ;
#3979 = CARTESIAN_POINT ( 'NONE',  ( 774.6858677611749044, -81.72551174932937101, -315.5713283507209894 ) ) ;
#3980 = CARTESIAN_POINT ( 'NONE',  ( 789.9200121543843807, -385.9874144716864066, -317.0176451133914384 ) ) ;
#3982 = CARTESIAN_POINT ( 'NONE',  ( 765.0180583372156207, -240.9982390220561683, 360.0135310231089534 ) ) ;
#3981 = CARTESIAN_POINT ( 'NONE',  ( 755.5713283507202505, -245.3618753856925139, 334.6858677611754729 ) ) ;
#3983 = CARTESIAN_POINT ( 'NONE',  ( 808.7758568127978833, -388.1692326535045936, -320.0363995740631822 ) ) ;
#3984 = FACE_OUTER_BOUND ( 'NONE', #23947, .T. ) ;
#3985 = ORIENTED_EDGE ( 'NONE', *, *, #37858, .F. ) ;
#3986 = CARTESIAN_POINT ( 'NONE',  ( 794.9819416627830151, -420.9982390220555999, 319.9864689768909898 ) ) ;
#3987 = AXIS2_PLACEMENT_3D ( 'NONE', #32877, #40697, #44160 ) ;
#3988 = ORIENTED_EDGE ( 'NONE', *, *, #22865, .F. ) ;
#3989 = CARTESIAN_POINT ( 'NONE',  ( 805.0032342141412300, -253.5436935675104735, -314.9967657858571783 ) ) ;
#3990 = CARTESIAN_POINT ( 'NONE',  ( 755.2512626584698410, -151.5436935675109851, 315.2512626584710915 ) ) ;
#3991 = CARTESIAN_POINT ( 'NONE',  ( 760.7433823573367135, -252.0090635724254184, 355.9930595647440441 ) ) ;
#3992 = ORIENTED_EDGE ( 'NONE', *, *, #37651, .F. ) ;
#3993 = CARTESIAN_POINT ( 'NONE',  ( 802.9823548866075953, -49.09997266333511590, -330.0799878456151077 ) ) ;
#3994 = CARTESIAN_POINT ( 'NONE',  ( 774.6858677611749044, -249.7255117493288594, -315.5713283507209894 ) ) ;
#3995 = ORIENTED_EDGE ( 'NONE', *, *, #39851, .F. ) ;
#3996 = CARTESIAN_POINT ( 'NONE',  ( 794.9819416627830151, -348.9982390220558273, -319.9864689768909898 ) ) ;
#3997 = CARTESIAN_POINT ( 'NONE',  ( 765.0180583372156207, -0.9982390220569063999, -360.0135310231089534 ) ) ;
#3998 = CARTESIAN_POINT ( 'NONE',  ( 754.9735926884551418, -234.3510508353232638, 340.5236548041000333 ) ) ;
#3999 = CARTESIAN_POINT ( 'NONE',  ( 989.9999999999992042, 249.9999999999998863, 360.0000000000000000 ) ) ;
#4000 = EDGE_CURVE ( 'NONE', #36366, #39863, #29876, .T. ) ;
#4001 = DIRECTION ( 'NONE',  ( 0.000000000000000000, 0.7651688349527167032, 0.6438296778008156807 ) ) ;
#4002 = ORIENTED_EDGE ( 'NONE', *, *, #13445, .T. ) ;
#4003 = CARTESIAN_POINT ( 'NONE',  ( 759.9864689768902508, -26.08914811296592262, -354.9819416627836404 ) ) ;
#4004 = FACE_OUTER_BOUND ( 'NONE', #29408, .T. ) ;
#4005 = FACE_OUTER_BOUND ( 'NONE', #18702, .T. ) ;
#4006 = AXIS2_PLACEMENT_3D ( 'NONE', #9807, #34741, #34279 ) ;
#4007 = ORIENTED_EDGE ( 'NONE', *, *, #13993, .F. ) ;
#4008 = CARTESIAN_POINT ( 'NONE',  ( 783.7953271457878373, -272.1908817542434917, -375.1787889125761239 ) ) ;
#4009 = COLOUR_RGB ( '',0.7921568627450980005, 0.8196078431372548767, 0.9333333333333333481 ) ;
#4010 = CARTESIAN_POINT ( 'NONE',  ( 745.1792804349281596, -182.1908817542437760, 343.7566961878542884 ) ) ;
#4012 = CARTESIAN_POINT ( 'NONE',  ( 774.6858677611749044, -249.7255117493288594, -315.5713283507209894 ) ) ;
#4011 = DIRECTION ( 'NONE',  ( 0.000000000000000000, 0.000000000000000000, 1.000000000000000000 ) ) ;
#4013 =( NAMED_UNIT ( * ) PLANE_ANGLE_UNIT ( ) SI_UNIT ( $, .RADIAN. ) );
#4014 = CARTESIAN_POINT ( 'NONE',  ( 755.5913626894240451, -109.6454272087894566, -346.6156483768012890 ) ) ;
#4015 = CARTESIAN_POINT ( 'NONE',  ( 776.2046728542105711, -380.1908817542431507, 304.8212110874238761 ) ) ;
#4016 = CARTESIAN_POINT ( 'NONE',  ( 914.9999999999992042, 74.99999999999984368, 360.0000000000000000 ) ) ;
#4017 = CARTESIAN_POINT ( 'NONE',  ( 794.1144889064781864, -442.1692326535044231, -360.9840315886528401 ) ) ;
#4018 = CARTESIAN_POINT ( 'NONE',  ( 805.0032342141413437, -301.5436935675105588, -314.9967657858572352 ) ) ;
#4019 = CARTESIAN_POINT ( 'NONE',  ( 787.4999999999992042, -512.9681489794448908, -350.0000000000000000 ) ) ;
#4020 = CARTESIAN_POINT ( 'NONE',  ( 804.6798772138708955, -15.72551174932958951, 334.6312213355107019 ) ) ;
#4021 = CARTESIAN_POINT ( 'NONE',  ( 744.6391490659812007, -254.7363362996981095, 338.7502325331110455 ) ) ;
#4022 = CARTESIAN_POINT ( 'NONE',  ( 746.0683387631852383, -187.4419599262325278, -331.3260364891676204 ) ) ;
#4023 = CARTESIAN_POINT ( 'NONE',  ( 801.1904061080336987, -236.0891481129651766, 368.3070685750235498 ) ) ;
#4024 = CARTESIAN_POINT ( 'NONE',  ( 805.0032342141412300, -445.5436935675098766, -314.9967657858571783 ) ) ;
#4025 = DIRECTION ( 'NONE',  ( -0.000000000000000000, -1.000000000000000000, -0.000000000000000000 ) ) ;
#4026 = AXIS2_PLACEMENT_3D ( 'NONE', #19087, #1302, #25779 ) ;
#4027 = EDGE_CURVE ( 'NONE', #37165, #1637, #32526, .T. ) ;
#4028 = CARTESIAN_POINT ( 'NONE',  ( 762.1405469898971887, -313.5436935675102745, 357.8594530101015607 ) ) ;
#4029 = AXIS2_PLACEMENT_3D ( 'NONE', #21182, #623, #4093 ) ;
#4030 = CARTESIAN_POINT ( 'NONE',  ( 783.0745993439762742, -104.1908817542440175, 365.1016975059196739 ) ) ;
#4031 = CARTESIAN_POINT ( 'NONE',  ( 784.1219089521767955, -69.28179084515321051, 315.0488828828318333 ) ) ;
#4032 = CARTESIAN_POINT ( 'NONE',  ( 800.7704444035546203, 19.83076734649410966, -326.0291762391768771 ) ) ;
#4033 = CARTESIAN_POINT ( 'NONE',  ( 879.9999999999992042, 259.9999999999998863, -219.9999999999999716 ) ) ;
#4034 = DIRECTION ( 'NONE',  ( -0.000000000000000000, -0.000000000000000000, 1.000000000000000000 ) ) ;
#4036 = CARTESIAN_POINT ( 'NONE',  ( 788.8264449731200330, -357.1800572038739006, 363.6646147819171233 ) ) ;
#4035 = CARTESIAN_POINT ( 'NONE',  ( 765.8855110935204493, -166.1692326535053041, 319.0159684113471599 ) ) ;
#4037 = VERTEX_POINT ( 'NONE', #18447 ) ;
#4038 = CLOSED_SHELL ( 'NONE', ( #31058, #22434, #2960, #37465, #8867, #4331, #31468, #30827, #28338, #25562, #22339, #14811, #10351, #34267, #14270, #3950, #35401, #26673, #27265, #41594, #29738, #38511, #4476, #14559, #23886, #6850, #33445, #43897, #6939, #7678, #5215, #45345, #8096, #19314, #27472, #31110, #41238, #32888, #26409, #34218, #12002, #2156, #24657, #12343, #449, #30335, #30877, #12039, #2630, #42991, #19585, #31775, #1543, #29801, #26516, #34550, #24314, #17624, #43061, #1258 ) ) ;
#4039 = CARTESIAN_POINT ( 'NONE',  ( 805.1016975059191054, -294.8965053807775689, -343.0745993439771837 ) ) ;
#4040 = CARTESIAN_POINT ( 'NONE',  ( 800.2193346964447755, -114.9982390220565236, 355.1360043628815788 ) ) ;
#4041 = VECTOR ( 'NONE', #22643, 1000.000000000000114 ) ;
#4042 = CARTESIAN_POINT ( 'NONE',  ( 748.3538107759620743, -304.7146871989594388, -355.8262568251490165 ) ) ;
#4043 = DIRECTION ( 'NONE',  ( 0.000000000000000000, 0.000000000000000000, -1.000000000000000000 ) ) ;
#4044 = CARTESIAN_POINT ( 'NONE',  ( 773.7943932421234194, -407.8055962898681628, 305.5313806188329409 ) ) ;
#4045 = ORIENTED_EDGE ( 'NONE', *, *, #41678, .F. ) ;
#4046 = CARTESIAN_POINT ( 'NONE',  ( 788.8264449731200330, -309.1800572038740711, 363.6646147819171233 ) ) ;
#4047 = VECTOR ( 'NONE', #8844, 1000.000000000000000 ) ;
#4048 = CARTESIAN_POINT ( 'NONE',  ( 776.9566956441375396, -84.89650538077830788, -364.8461984189686405 ) ) ;
#4049 = CARTESIAN_POINT ( 'NONE',  ( 765.0180583372156207, -168.9982390220563673, -360.0135310231089534 ) ) ;
#4050 = CARTESIAN_POINT ( 'NONE',  ( 800.2193346964447755, -210.9982390220561967, -355.1360043628815788 ) ) ;
#4051 = CARTESIAN_POINT ( 'NONE',  ( 758.0580252608178853, -438.4527844766009821, 328.0187753319985404 ) ) ;
#4052 = EDGE_CURVE ( 'NONE', #40519, #28937, #18128, .T. ) ;
#4053 = CARTESIAN_POINT ( 'NONE',  ( 772.4837098697144029, -143.3618753856927697, -374.5518280994205611 ) ) ;
#4054 = VERTEX_POINT ( 'NONE', #7588 ) ;
#4055 = CARTESIAN_POINT ( 'NONE',  ( 804.4286716492782716, -137.3618753856928265, -345.3141322388244703 ) ) ;
#4056 = ORIENTED_EDGE ( 'NONE', *, *, #11433, .F. ) ;
#4057 = CARTESIAN_POINT ( 'NONE',  ( 784.1219089521767955, -381.2817908451523294, -315.0488828828318333 ) ) ;
#4058 = CIRCLE ( 'NONE', #19533, 2.749999999999919176 ) ;
#4059 = CARTESIAN_POINT ( 'NONE',  ( 805.1927285166397041, 7.183579159761247723, 341.8018195045277707 ) ) ;
#4060 = CARTESIAN_POINT ( 'NONE',  ( 761.2382568024794409, -111.6237781080509279, 356.9571628226838129 ) ) ;
#4063 = CARTESIAN_POINT ( 'NONE',  ( 781.2497674668890113, -396.3510508353228374, 375.3608509340180603 ) ) ;
#4062 = CARTESIAN_POINT ( 'NONE',  ( 571.1634899080285095, 259.9999999999999432, -199.9999999999981526 ) ) ;
#4061 = CYLINDRICAL_SURFACE ( 'NONE', #24012, 10.00000000000000888 ) ;
#4064 = ADVANCED_FACE ( 'NONE', ( #14287 ), #39469, .F. ) ;
#4065 = AXIS2_PLACEMENT_3D ( 'NONE', #36577, #1457, #36799 ) ;
#4066 = AXIS2_PLACEMENT_3D ( 'NONE', #30420, #33670, #44059 ) ;
#4067 = VERTEX_POINT ( 'NONE', #29061 ) ;
#4068 = CARTESIAN_POINT ( 'NONE',  ( 796.9571628226829034, -383.4636090269704596, -321.2382568024804641 ) ) ;
#4069 = CARTESIAN_POINT ( 'NONE',  ( -468.8365100919714337, 256.5000000000001705, -199.9999999999908766 ) ) ;
#4070 = CARTESIAN_POINT ( 'NONE',  ( 750.9282345327678740, -184.9181544815165239, -319.8311093483690115 ) ) ;
#4071 = CARTESIAN_POINT ( 'NONE',  ( 778.7629533639073998, -32.73633629969879877, 375.0009284576466371 ) ) ;
#4073 = CARTESIAN_POINT ( 'NONE',  ( 746.4999999999993179, -365.3551492539851893, -18.13243251470705886 ) ) ;
#4072 = DIRECTION ( 'NONE',  ( -0.000000000000000000, 1.000000000000000000, -0.000000000000000000 ) ) ;
#4074 = CARTESIAN_POINT ( 'NONE',  ( 800.7704444035546203, -340.1692326535047641, -326.0291762391768771 ) ) ;
#4075 = CARTESIAN_POINT ( 'NONE',  ( 755.0636971347428243, -436.2709662947827951, -341.7834795799807353 ) ) ;
#4076 = CARTESIAN_POINT ( 'NONE',  ( 752.7379699480933368, -180.0090635724255890, -361.9858362298580232 ) ) ;
#4077 = CARTESIAN_POINT ( 'NONE',  ( 791.7608162188021197, 205.0000000000000568, 319.9999999999999432 ) ) ;
#4078 = DIRECTION ( 'NONE',  ( 0.000000000000000000, 1.000000000000000000, 0.000000000000000000 ) ) ;
#4079 = CARTESIAN_POINT ( 'NONE',  ( 784.1219089521767955, -357.2817908451523294, 315.0488828828318333 ) ) ;
#4080 = VECTOR ( 'NONE', #42549, 1000.000000000000000 ) ;
#4081 = CARTESIAN_POINT ( 'NONE',  ( 813.5763878283155464, -339.8272453906069472, 351.1614460488615350 ) ) ;
#4082 =( GEOMETRIC_REPRESENTATION_CONTEXT ( 3 ) GLOBAL_UNCERTAINTY_ASSIGNED_CONTEXT ( ( #12105 ) ) GLOBAL_UNIT_ASSIGNED_CONTEXT ( ( #12261, #26559, #8797 ) ) REPRESENTATION_CONTEXT ( 'NONE', 'WORKASPACE' ) );
#4083 = CARTESIAN_POINT ( 'NONE',  ( 763.2262854647970016, -224.6346026584198228, -309.2812353651462445 ) ) ;
#4084 = ADVANCED_FACE ( 'NONE', ( #10827, #656, #18227 ), #25354, .F. ) ;
#4085 = CARTESIAN_POINT ( 'NONE',  ( -789.9999999999992042, 205.0000000000000568, -350.0000000000000000 ) ) ;
#4086 = FACE_OUTER_BOUND ( 'NONE', #29358, .T. ) ;
#4087 = CIRCLE ( 'NONE', #9970, 6.118999999999985562 ) ;
#4088 = CARTESIAN_POINT ( 'NONE',  ( 802.2119215644370342, -150.0090635724257027, 367.5423716828165084 ) ) ;
#4089 = ADVANCED_FACE ( 'NONE', ( #39013 ), #14531, .F. ) ;
#4090 = CARTESIAN_POINT ( 'NONE',  ( 751.2241431872005251, -88.16923265350555994, -359.9636004259367610 ) ) ;
#4091 = CARTESIAN_POINT ( 'NONE',  ( 763.2262854647970016, -104.6346026584202207, 309.2812353651462445 ) ) ;
#4092 = CARTESIAN_POINT ( 'NONE',  ( 801.1904061080336987, -332.0891481129649492, -368.3070685750235498 ) ) ;
#4093 = DIRECTION ( 'NONE',  ( 1.000000000000000000, 0.000000000000000000, 0.000000000000000000 ) ) ;
#4094 = DIRECTION ( 'NONE',  ( 1.000000000000000000, -4.147566128926363633E-16, 0.000000000000000000 ) ) ;
#4095 = CARTESIAN_POINT ( 'NONE',  ( 762.1405469898971887, -217.5436935675107293, 357.8594530101015607 ) ) ;
#4096 = VECTOR ( 'NONE', #2071, 1000.000000000000000 ) ;
#4097 = CARTESIAN_POINT ( 'NONE',  ( 811.3240766477731540, -460.3726999360611103, 355.6651683502462902 ) ) ;
#4098 = CARTESIAN_POINT ( 'NONE',  ( 766.5853460496234675, -397.9874144716864066, -372.3518521366060554 ) ) ;
#4099 = AXIS2_PLACEMENT_3D ( 'NONE', #15118, #4034, #17897 ) ;
#4100 = CARTESIAN_POINT ( 'NONE',  ( 777.5031285880264704, -430.8164208402374129, -374.9108240113588408 ) ) ;
#4101 = CARTESIAN_POINT ( 'NONE',  ( -598.8365100919716042, 230.0000000000001421, -199.9999999999899671 ) ) ;
#4102 = CARTESIAN_POINT ( 'NONE',  ( 749.8865473780648472, 3.467130982857797417, 322.1177392798429082 ) ) ;
#4103 = ORIENTED_EDGE ( 'NONE', *, *, #34208, .T. ) ;
#4104 = VECTOR ( 'NONE', #21357, 1000.000000000000000 ) ;
#4105 = CARTESIAN_POINT ( 'NONE',  ( 805.1927285166397041, -16.81642084023866701, 341.8018195045277707 ) ) ;
#4106 = CARTESIAN_POINT ( 'NONE',  ( 795.6651683502461765, -178.7146871989598083, -371.3240766477733814 ) ) ;
#4107 = SURFACE_STYLE_USAGE ( .BOTH. , #4335 ) ;
#4108 = CARTESIAN_POINT ( 'NONE',  ( 811.6461892240364477, -316.7146871989593819, 324.1737431748509835 ) ) ;
#4109 = CARTESIAN_POINT ( 'NONE',  ( 795.1360043628808398, -164.0891481129654892, 360.2193346964456282 ) ) ;
#4110 = ORIENTED_EDGE ( 'NONE', *, *, #45593, .F. ) ;
#4111 = EDGE_CURVE ( 'NONE', #1382, #39820, #21040, .T. ) ;
#4112 = EDGE_CURVE ( 'NONE', #32155, #33694, #39924, .T. ) ;
#4113 = CARTESIAN_POINT ( 'NONE',  ( 802.1676090361156639, -302.6346026584196238, 327.8955696845344505 ) ) ;
#4114 = EDGE_CURVE ( 'NONE', #1656, #27668, #11278, .T. ) ;
#4115 = CARTESIAN_POINT ( 'NONE',  ( 792.2312462859673587, -35.90732993114770011, -307.2067596250082602 ) ) ;
#4116 = CARTESIAN_POINT ( 'NONE',  ( 808.0189434323515343, -86.08914811296573077, 319.0252816721025511 ) ) ;
#4117 = ORIENTED_EDGE ( 'NONE', *, *, #31446, .T. ) ;
#4118 = CARTESIAN_POINT ( 'NONE',  ( 804.1009440267234822, -431.4636090269702322, -314.0944755984392600 ) ) ;
#4119 = VECTOR ( 'NONE', #8933, 1000.000000000000000 ) ;
#4120 = VERTEX_POINT ( 'NONE', #22332 ) ;
#4121 = SHAPE_DEFINITION_REPRESENTATION ( #14099, #28408 ) ;
#4123 = CARTESIAN_POINT ( 'NONE',  ( 780.5236548040995785, -332.7363362996979390, 314.9735926884559944 ) ) ;
#4122 = CARTESIAN_POINT ( 'NONE',  ( 771.2633955100217236, -71.90732993114760063, 363.4237431249939618 ) ) ;
#4124 = CARTESIAN_POINT ( 'NONE',  ( 788.8264449731200330, -285.1800572038740711, -363.6646147819171233 ) ) ;
#4125 = AXIS2_PLACEMENT_3D ( 'NONE', #17713, #10773, #13327 ) ;
#4127 = CARTESIAN_POINT ( 'NONE',  ( 815.1787889125755555, -270.8965053807777394, 343.7953271457877804 ) ) ;
#4126 = CARTESIAN_POINT ( 'NONE',  ( 758.8095938919644823, -392.0891481129647786, 311.6929314249762797 ) ) ;
#4128 = EDGE_CURVE ( 'NONE', #29032, #40245, #25599, .T. ) ;
#4129 = CARTESIAN_POINT ( 'NONE',  ( 759.8311093483677041, -70.16923265350563099, 310.9282345327691814 ) ) ;
#4130 = CARTESIAN_POINT ( 'NONE',  ( 775.8780910478218402, -297.2817908451526137, -364.9511171171680530 ) ) ;
#4131 = CARTESIAN_POINT ( 'NONE',  ( 804.6798772138708955, -279.7255117493288026, -334.6312213355107019 ) ) ;
#4132 = CARTESIAN_POINT ( 'NONE',  ( 788.7366044899766848, -443.9073299311464780, -316.5762568750059813 ) ) ;
#4133 = CARTESIAN_POINT ( 'NONE',  ( 800.0135310231082713, -134.0891481129655745, -325.0180583372163028 ) ) ;
#4134 = DIRECTION ( 'NONE',  ( 0.000000000000000000, 0.000000000000000000, 1.000000000000000000 ) ) ;
#4135 = CARTESIAN_POINT ( 'NONE',  ( 814.5518280994195948, -399.7255117493283478, 332.4837098697145734 ) ) ;
#4136 = CIRCLE ( 'NONE', #36560, 12.00000000000001066 ) ;
#4138 = DIRECTION ( 'NONE',  ( -0.000000000000000000, -0.000000000000000000, 1.000000000000000000 ) ) ;
#4137 = CARTESIAN_POINT ( 'NONE',  ( 779.9999999999990905, 18.49609980828599376, 309.9999999999999432 ) ) ;
#4139 = CARTESIAN_POINT ( 'NONE',  ( 810.4231160770870019, -96.55451811788039151, -321.9338519418446936 ) ) ;
#4140 = CARTESIAN_POINT ( 'NONE',  ( 759.9999999999992042, -512.9681489794448908, -339.9999999999999432 ) ) ;
#4141 = DIRECTION ( 'NONE',  ( -1.000000000000000000, -0.000000000000000000, 0.000000000000000000 ) ) ;
#4142 = CARTESIAN_POINT ( 'NONE',  ( 755.8894580844503253, -255.8272453906072315, 332.3691319403863531 ) ) ;
#4143 = CARTESIAN_POINT ( 'NONE',  ( 765.0180583372156207, -144.9982390220564525, 360.0135310231089534 ) ) ;
#4144 = ORIENTED_EDGE ( 'NONE', *, *, #30071, .T. ) ;
#4145 = CARTESIAN_POINT ( 'NONE',  ( 800.9840315886518738, -52.91815448151692891, -354.1144889064786412 ) ) ;
#4146 = CARTESIAN_POINT ( 'NONE',  ( 767.7687537140311633, -119.9073299311474443, -372.7932403749916830 ) ) ;
#4147 = CARTESIAN_POINT ( 'NONE',  ( 794.1144889064781864, -322.1692326535048210, 360.9840315886528401 ) ) ;
#4148 = DIRECTION ( 'NONE',  ( 0.000000000000000000, -0.000000000000000000, -1.000000000000000000 ) ) ;
#4149 = CARTESIAN_POINT ( 'NONE',  ( 797.8822607201568644, -54.55451811788054783, 370.1134526219340160 ) ) ;
#4150 = EDGE_CURVE ( 'NONE', #12347, #23226, #9248, .T. ) ;
#4151 = CARTESIAN_POINT ( 'NONE',  ( 815.2698199232961542, -232.8164208402379245, -342.5225473063383106 ) ) ;
#4152 = CARTESIAN_POINT ( 'NONE',  ( 805.0032342141412300, -205.5436935675108430, 314.9967657858571783 ) ) ;
#4153 = CARTESIAN_POINT ( 'NONE',  ( 788.8264449731200330, -117.1800572038746964, 363.6646147819171233 ) ) ;
#4154 = CARTESIAN_POINT ( 'NONE',  ( 919.9999999999993179, 219.9999999999998863, -360.0000000000000000 ) ) ;
#4155 = CARTESIAN_POINT ( 'NONE',  ( 807.5423716828161105, -321.0783235625956991, -362.2119215644372048 ) ) ;
#4156 = VECTOR ( 'NONE', #20629, 1000.000000000000000 ) ;
#4157 = CARTESIAN_POINT ( 'NONE',  ( 795.8262568251477660, -454.3726999360611103, 308.3538107759623585 ) ) ;
#4158 = CARTESIAN_POINT ( 'NONE',  ( 792.2312462859673587, -323.9073299311468190, -307.2067596250082602 ) ) ;
#4159 = CARTESIAN_POINT ( 'NONE',  ( 779.9999999999992042, -462.9681489794448339, -339.9999999999999432 ) ) ;
#4160 = CARTESIAN_POINT ( 'NONE',  ( 802.7791456095903868, -364.7146871989592114, 329.0155153010375102 ) ) ;
#4161 = VECTOR ( 'NONE', #30084, 1000.000000000000114 ) ;
#4162 = CARTESIAN_POINT ( 'NONE',  ( 812.7932403749906598, -39.18005720387496638, 327.7687537140311633 ) ) ;
#4163 = CARTESIAN_POINT ( 'NONE',  ( 762.1405469898971887, -433.5436935675099903, -357.8594530101015607 ) ) ;
#4164 = CARTESIAN_POINT ( 'NONE',  ( 766.7756240680305382, -38.53286901714206891, 361.5560724626415663 ) ) ;
#4165 = CARTESIAN_POINT ( 'NONE',  ( 812.6845335610512393, -79.98741447168740137, -353.5525998758768651 ) ) ;
#4166 = CARTESIAN_POINT ( 'NONE',  ( 759.8311093483677041, -190.1692326535052189, 310.9282345327691814 ) ) ;
#4167 = CARTESIAN_POINT ( 'NONE',  ( 797.6776695296629214, -43.54369356751131903, 357.6776695296636603 ) ) ;
#4168 = AXIS2_PLACEMENT_3D ( 'NONE', #23038, #40839, #9199 ) ;
#4169 = ADVANCED_FACE ( 'NONE', ( #32754 ), #1101, .T. ) ;
#4170 = ORIENTED_EDGE ( 'NONE', *, *, #42160, .F. ) ;
#4171 = CARTESIAN_POINT ( 'NONE',  ( 802.7791456095903868, -196.7146871989598083, -329.0155153010375102 ) ) ;
#4172 = CARTESIAN_POINT ( 'NONE',  ( 774.6312213355099630, -191.3618753856925991, 364.6798772138717482 ) ) ;
#4173 = VECTOR ( 'NONE', #3721, 1000.000000000000000 ) ;
#4174 = CARTESIAN_POINT ( 'NONE',  ( 798.0661480581538854, -26.53286901714210799, -309.5768839229118043 ) ) ;
#4175 = CARTESIAN_POINT ( 'NONE',  ( 800.0135310231082713, -326.0891481129649492, 325.0180583372163028 ) ) ;
#4176 = CARTESIAN_POINT ( 'NONE',  ( 919.9999999999993179, 219.9999999999998863, -359.9749999999999659 ) ) ;
#4177 = DIRECTION ( 'NONE',  ( -1.058954862565134068E-16, 0.6438296778008191223, -0.7651688349527137056 ) ) ;
#4178 = ORIENTED_EDGE ( 'NONE', *, *, #40459, .T. ) ;
#4179 = CARTESIAN_POINT ( 'NONE',  ( 761.2382568024794409, -63.62377810805107714, 356.9571628226838129 ) ) ;
#4180 = CARTESIAN_POINT ( 'NONE',  ( 791.0478386215596629, -333.8272453906070041, -306.7653713866226326 ) ) ;
#4181 = CARTESIAN_POINT ( 'NONE',  ( 814.9108240113580450, -280.2709662947833067, 337.5031285880265273 ) ) ;
#4182 = CARTESIAN_POINT ( 'NONE',  ( 801.9858362298568863, -3.078323562596726681, 312.7379699480935642 ) ) ;
#4183 = CARTESIAN_POINT ( 'NONE',  ( 775.8780910478218402, -201.2817908451528126, -364.9511171171680530 ) ) ;
#4184 = CARTESIAN_POINT ( 'NONE',  ( 771.2633955100217236, -191.9073299311471885, -363.4237431249939618 ) ) ;
#4185 = CARTESIAN_POINT ( 'NONE',  ( 781.8018195045267476, -358.2709662947830225, -365.1927285166407273 ) ) ;
#4186 = ORIENTED_EDGE ( 'NONE', *, *, #41613, .F. ) ;
#4187 = VECTOR ( 'NONE', #5345, 1000.000000000000000 ) ;
#4188 = CARTESIAN_POINT ( 'NONE',  ( 811.0346526505616112, -302.6346026584196238, 323.0537975583477532 ) ) ;
#4189 = DIRECTION ( 'NONE',  ( -2.750100768424433062E-32, 1.672022627447525240E-16, 1.000000000000000000 ) ) ;
#4190 = CARTESIAN_POINT ( 'NONE',  ( 787.5531968255692163, -213.8272453906073167, 316.1348686366205811 ) ) ;
#4191 = VECTOR ( 'NONE', #11167, 1000.000000000000114 ) ;
#4192 = CARTESIAN_POINT ( 'NONE',  ( -728.8365100919714905, 240.0000000000001990, -197.2499999999891998 ) ) ;
#4193 = CARTESIAN_POINT ( 'NONE',  ( 796.9571628226829034, -167.4636090269711133, 321.2382568024804641 ) ) ;
#4194 = CARTESIAN_POINT ( 'NONE',  ( 774.6858677611749044, -33.72551174932952733, 315.5713283507209894 ) ) ;
#4195 = EDGE_LOOP ( 'NONE', ( #34713, #2219 ) ) ;
#4196 = CARTESIAN_POINT ( 'NONE',  ( 776.2046728542105711, -428.1908817542430938, -304.8212110874238761 ) ) ;
#4197 = VECTOR ( 'NONE', #23243, 1000.000000000000000 ) ;
#4198 = CARTESIAN_POINT ( 'NONE',  ( 758.8095938919644823, -8.089148112965974136, -311.6929314249762797 ) ) ;
#4199 = CARTESIAN_POINT ( 'NONE',  ( 745.5313806188320314, -255.2817908451526705, 333.7943932421247268 ) ) ;
#4200 = CARTESIAN_POINT ( 'NONE',  ( 757.2208543904082489, -208.7146871989596946, 350.9844846989624330 ) ) ;
#4201 = CARTESIAN_POINT ( 'NONE',  ( 805.1927285166397041, -352.8164208402374129, -341.8018195045277707 ) ) ;
#4202 = CARTESIAN_POINT ( 'NONE',  ( -200.7583438952259485, 394.6698570112193920, -274.9999999999999432 ) ) ;
#4203 = CARTESIAN_POINT ( 'NONE',  ( 778.1981804954714335, 13.72903370521577138, 314.8072714833589885 ) ) ;
#4204 = DIRECTION ( 'NONE',  ( -0.000000000000000000, -0.000000000000000000, 1.000000000000000000 ) ) ;
#4205 = CARTESIAN_POINT ( 'NONE',  ( 793.0897708529556667, -270.5545181178798657, -361.3366627262616362 ) ) ;
#4206 = CARTESIAN_POINT ( 'NONE',  ( 747.2067596250078623, -3.180057203875080063, 352.2312462859687230 ) ) ;
#4207 = CARTESIAN_POINT ( 'NONE',  ( 758.8095938919642549, -104.0891481129656881, 311.6929314249763365 ) ) ;
#4208 = DIRECTION ( 'NONE',  ( -0.000000000000000000, -0.000000000000000000, 1.000000000000000000 ) ) ;
#4209 = CARTESIAN_POINT ( 'NONE',  ( 808.0189434323515343, -446.0891481129646081, -319.0252816721025511 ) ) ;
#4210 = DIRECTION ( 'NONE',  ( 0.000000000000000000, 1.000000000000000000, 0.000000000000000000 ) ) ;
#4211 = CARTESIAN_POINT ( 'NONE',  ( 799.9636004259356241, -382.9181544815159555, 311.2241431872006956 ) ) ;
#4212 = CARTESIAN_POINT ( 'NONE',  ( 794.9999999999993179, 205.0000000000000568, -274.9999999999999432 ) ) ;
#4213 = CARTESIAN_POINT ( 'NONE',  ( 745.7998596910086917, -317.3618753856922581, 332.5602148656461168 ) ) ;
#4214 = CARTESIAN_POINT ( 'NONE',  ( 767.6429770376289525, -105.1800572038747248, -306.8695393053162093 ) ) ;
#4215 = CARTESIAN_POINT ( 'NONE',  ( 755.0636971347428243, -268.2709662947833067, -341.7834795799807353 ) ) ;
#4216 = DIRECTION ( 'NONE',  ( 0.000000000000000000, -0.000000000000000000, -1.000000000000000000 ) ) ;
#4217 = CARTESIAN_POINT ( 'NONE',  ( 788.7366044899766848, -443.9073299311464780, 316.5762568750059813 ) ) ;
#4218 = CARTESIAN_POINT ( 'NONE',  ( 755.8894580844503253, -183.8272453906074020, 332.3691319403863531 ) ) ;
#4219 = CARTESIAN_POINT ( 'NONE',  ( 754.3581564841646241, -65.46360902697142592, -316.1443688327762516 ) ) ;
#4220 = CARTESIAN_POINT ( 'NONE',  ( 775.9200461376533440, -95.80559628986917176, -315.3028492785443291 ) ) ;
#4221 = CARTESIAN_POINT ( 'NONE',  ( 771.2368401574024119, -109.4419599262327836, 374.2805881961240857 ) ) ;
#4222 = CARTESIAN_POINT ( 'NONE',  ( 755.5713283507202505, -413.3618753856920307, 334.6858677611754729 ) ) ;
#4223 = VECTOR ( 'NONE', #36106, 1000.000000000000000 ) ;
#4224 = CARTESIAN_POINT ( 'NONE',  ( 795.1360043628807261, 3.910851887033985896, -360.2193346964456282 ) ) ;
#4226 = ORIENTED_EDGE ( 'NONE', *, *, #132, .T. ) ;
#4225 = CARTESIAN_POINT ( 'NONE',  ( 764.0069404352550464, -111.0783235625964096, -359.2566176426627180 ) ) ;
#4227 = CARTESIAN_POINT ( 'NONE',  ( 804.4286716492782716, -89.36187538569299704, -345.3141322388244703 ) ) ;
#4228 = AXIS2_PLACEMENT_3D ( 'NONE', #19562, #44748, #44506 ) ;
#4229 = CARTESIAN_POINT ( 'NONE',  ( 804.1601925771018387, -415.4419599262318457, -346.5483106153029098 ) ) ;
#4231 = CARTESIAN_POINT ( 'NONE',  ( 803.4237431249931660, -231.1800572038743553, 331.2633955100225194 ) ) ;
#4230 = CARTESIAN_POINT ( 'NONE',  ( 804.6798772138708955, -231.7255117493288310, 334.6312213355107019 ) ) ;
#4232 = CARTESIAN_POINT ( 'NONE',  ( 781.2497674668890113, -396.3510508353228374, -375.3608509340180603 ) ) ;
#4233 = CARTESIAN_POINT ( 'NONE',  ( 799.9999999999993179, 205.0000000000000568, 255.0000000000000000 ) ) ;
#4234 = ORIENTED_EDGE ( 'NONE', *, *, #22360, .F. ) ;
#4235 = CARTESIAN_POINT ( 'NONE',  ( 754.8072714833581358, -412.8164208402372992, 338.1981804954720587 ) ) ;
#4236 = VECTOR ( 'NONE', #31435, 1000.000000000000000 ) ;
#4237 = ORIENTED_EDGE ( 'NONE', *, *, #5197, .T. ) ;
#4238 = VECTOR ( 'NONE', #23176, 1000.000000000000000 ) ;
#4239 = CARTESIAN_POINT ( 'NONE',  ( 763.0537975583476964, -192.4527844766017211, 371.0346526505628617 ) ) ;
#4240 = CARTESIAN_POINT ( 'NONE',  ( 769.9779781133707957, -259.0999726633343698, 316.7813123517150871 ) ) ;
#4241 = ORIENTED_EDGE ( 'NONE', *, *, #14801, .F. ) ;
#4242 = CARTESIAN_POINT ( 'NONE',  ( 796.9571628226829034, -71.46360902697141171, -321.2382568024804641 ) ) ;
#4243 = CARTESIAN_POINT ( 'NONE',  ( 808.7758568127978833, -220.1692326535051052, 320.0363995740631822 ) ) ;
#4244 = CARTESIAN_POINT ( 'NONE',  ( 791.9812246680005501, -260.6346026584197375, -361.9419747391813189 ) ) ;
#4245 = ORIENTED_EDGE ( 'NONE', *, *, #4281, .T. ) ;
#4246 = CARTESIAN_POINT ( 'NONE',  ( 755.3201227861273992, -411.7255117493282910, -345.3687786644892981 ) ) ;
#4247 = CARTESIAN_POINT ( 'NONE',  ( 803.6646147819161570, -41.90732993114767169, -348.8264449731210561 ) ) ;
#4248 = CARTESIAN_POINT ( 'NONE',  ( 801.3366627262608972, -248.5328690171414223, 353.0897708529566899 ) ) ;
#4249 = CARTESIAN_POINT ( 'NONE',  ( 879.9999999999992042, 259.9999999999998863, -179.9999999999999716 ) ) ;
#4250 = DIRECTION ( 'NONE',  ( -0.000000000000000000, -0.000000000000000000, 1.000000000000000000 ) ) ;
#4251 = CARTESIAN_POINT ( 'NONE',  ( 778.2165204200184689, -22.81642084023865280, -364.9363028652563230 ) ) ;
#4252 = CARTESIAN_POINT ( 'NONE',  ( -858.8365100919713768, 260.0000000000002274, -199.9999999999881481 ) ) ;
#4253 = DIRECTION ( 'NONE',  ( 0.000000000000000000, 0.000000000000000000, 1.000000000000000000 ) ) ;
#4254 = ORIENTED_EDGE ( 'NONE', *, *, #42215, .F. ) ;
#4255 = CARTESIAN_POINT ( 'NONE',  ( 771.3260364891663130, -307.6454272087888171, -306.0683387631859773 ) ) ;
#4256 = CARTESIAN_POINT ( 'NONE',  ( 771.3260364891663130, -187.6454272087892434, 306.0683387631859773 ) ) ;
#4258 = CARTESIAN_POINT ( 'NONE',  ( 778.2165204200184689, -262.8164208402379245, -364.9363028652563230 ) ) ;
#4257 = LINE ( 'NONE', #18348, #1013 ) ;
#4259 =( NAMED_UNIT ( * ) SI_UNIT ( $, .STERADIAN. ) SOLID_ANGLE_UNIT ( ) );
#4260 = CARTESIAN_POINT ( 'NONE',  ( 755.1538015810308480, -110.1908817542440033, -343.0433043558613804 ) ) ;
#4261 = DIRECTION ( 'NONE',  ( 0.000000000000000000, 0.000000000000000000, -1.000000000000000000 ) ) ;
#4262 = CARTESIAN_POINT ( 'NONE',  ( 804.7487373415286811, -331.5436935675104451, -364.7487373415288516 ) ) ;
#4263 = DIRECTION ( 'NONE',  ( -1.880165489482579047E-16, -1.000000000000000000, -0.000000000000000000 ) ) ;
#4264 = CARTESIAN_POINT ( 'NONE',  ( 797.8594530101008786, -13.54369356751140785, 322.1405469898980982 ) ) ;
#4265 = AXIS2_PLACEMENT_3D ( 'NONE', #26627, #44191, #15789 ) ;
#4266 = CARTESIAN_POINT ( 'NONE',  ( 815.3608509340175488, -242.7363362996980811, 341.2497674668889545 ) ) ;
#4267 = CARTESIAN_POINT ( 'NONE',  ( 788.7631598425961101, -193.4419599262325278, -305.7194118038759143 ) ) ;
#4268 = CARTESIAN_POINT ( 'NONE',  ( 810.7187646348534145, -210.4527844766016926, 356.7737145352016341 ) ) ;
#4269 = CARTESIAN_POINT ( 'NONE',  ( 781.2370466360911223, 3.263663700301089765, -304.9990715423533629 ) ) ;
#4270 = DIRECTION ( 'NONE',  ( -1.000000000000000000, -0.000000000000000000, -0.000000000000000000 ) ) ;
#4271 = ORIENTED_EDGE ( 'NONE', *, *, #20771, .T. ) ;
#4272 = CARTESIAN_POINT ( 'NONE',  ( 755.5713283507202505, -317.3618753856922581, 334.6858677611754729 ) ) ;
#4273 = CARTESIAN_POINT ( 'NONE',  ( 755.8894580844503253, -87.82724539060770041, 332.3691319403863531 ) ) ;
#4274 = CARTESIAN_POINT ( 'NONE',  ( 795.1360043628807261, -452.0891481129646650, -360.2193346964456282 ) ) ;
#4275 = DIRECTION ( 'NONE',  ( 1.000000000000000000, -0.000000000000000000, -0.000000000000000000 ) ) ;
#4276 = DIRECTION ( 'NONE',  ( 0.000000000000000000, 0.000000000000000000, 1.000000000000000000 ) ) ;
#4278 = CARTESIAN_POINT ( 'NONE',  ( 778.1981804954714335, -346.2709662947830793, 314.8072714833589885 ) ) ;
#4277 = CARTESIAN_POINT ( 'NONE',  ( 765.8855110935204493, -142.1692326535054178, 319.0159684113471599 ) ) ;
#4279 = EDGE_LOOP ( 'NONE', ( #11514, #37775, #36088, #40359, #36090, #1787 ) ) ;
#4280 = CARTESIAN_POINT ( 'NONE',  ( 761.2382568024794409, -279.6237781080503737, -356.9571628226838129 ) ) ;
#4281 = EDGE_CURVE ( 'NONE', #33261, #44892, #11744, .T. ) ;
#4282 = CARTESIAN_POINT ( 'NONE',  ( 747.3154664389472828, -307.9874144716866340, -326.4474001241230781 ) ) ;
#4283 = DIRECTION ( 'NONE',  ( 1.000000000000000000, 0.000000000000000000, -0.000000000000000000 ) ) ;
#4284 = CARTESIAN_POINT ( 'NONE',  ( 813.2346286133761168, -437.2601417444135450, 328.9521613784389160 ) ) ;
#4285 = ORIENTED_EDGE ( 'NONE', *, *, #33494, .F. ) ;
#4286 = CARTESIAN_POINT ( 'NONE',  ( 804.4286716492782716, -329.3618753856922581, 345.3141322388244703 ) ) ;
#4287 = CARTESIAN_POINT ( 'NONE',  ( 780.5290396650775619, -84.35105083532374692, -365.2837595273619513 ) ) ;
#4288 = FACE_OUTER_BOUND ( 'NONE', #809, .T. ) ;
#4289 = CARTESIAN_POINT ( 'NONE',  ( 745.0891759886404770, -148.2709662947837330, -342.4968714119734159 ) ) ;
#4290 = EDGE_LOOP ( 'NONE', ( #8058, #41150 ) ) ;
#4291 = CARTESIAN_POINT ( 'NONE',  ( 767.8955696845334842, -144.4527844766018632, -362.1676090361161755 ) ) ;
#4292 = ORIENTED_EDGE ( 'NONE', *, *, #2348, .F. ) ;
#4293 = AXIS2_PLACEMENT_3D ( 'NONE', #11828, #43461, #29389 ) ;
#4294 = CARTESIAN_POINT ( 'NONE',  ( 802.5472867521000353, -436.3726999360612240, -350.8726784830461156 ) ) ;
#4295 = CARTESIAN_POINT ( 'NONE',  ( 800.9840315886518738, -460.9181544815156713, 354.1144889064786412 ) ) ;
#4296 = CARTESIAN_POINT ( 'NONE',  ( 765.8855110935204493, -142.1692326535054178, 319.0159684113471599 ) ) ;
#4299 = CARTESIAN_POINT ( 'NONE',  ( 761.9338519418445230, -398.5328690171409107, 370.4231160770881957 ) ) ;
#4298 = CARTESIAN_POINT ( 'NONE',  ( 999.9999999999992042, 239.9999999999998863, -350.0000000000000000 ) ) ;
#4297 = CARTESIAN_POINT ( 'NONE',  ( 773.4999999999993179, -544.8427095258973623, -369.9999999999999432 ) ) ;
#4300 = ORIENTED_EDGE ( 'NONE', *, *, #37389, .T. ) ;
#4301 = CARTESIAN_POINT ( 'NONE',  ( 783.0745993439762742, -392.1908817542432075, -365.1016975059196739 ) ) ;
#4302 = CARTESIAN_POINT ( 'NONE',  ( 441.1634899080286232, 259.9999999999999432, -199.9999999999972431 ) ) ;
#4303 = CARTESIAN_POINT ( 'NONE',  ( 810.4231160770870019, -168.5545181178802352, -321.9338519418446936 ) ) ;
#4304 = CARTESIAN_POINT ( 'NONE',  ( 788.6739635108323228, -79.64542720878957027, 373.9316612368139090 ) ) ;
#4305 = CARTESIAN_POINT ( 'NONE',  ( 799.9999999999993179, 166.4563064324884465, -319.9999999999999432 ) ) ;
#4306 = CARTESIAN_POINT ( 'NONE',  ( 799.4546378042377910, -321.0783235625956991, -356.1575198192848006 ) ) ;
#4307 = DIRECTION ( 'NONE',  ( -1.880165489482579047E-16, -1.000000000000000000, 0.000000000000000000 ) ) ;
#4308 = CARTESIAN_POINT ( 'NONE',  ( 762.1177392798416577, -186.5545181178801215, -309.8865473780659272 ) ) ;
#4309 = LINE ( 'NONE', #11695, #44390 ) ;
#4310 = DIRECTION ( 'NONE',  ( 0.000000000000000000, 0.000000000000000000, 1.000000000000000000 ) ) ;
#4311 = CARTESIAN_POINT ( 'NONE',  ( 787.5531968255692163, -405.8272453906067199, 316.1348686366205811 ) ) ;
#4312 = CARTESIAN_POINT ( 'NONE',  ( 764.1737431748507561, -346.3726999360614514, 371.6461892240376415 ) ) ;
#4313 = CARTESIAN_POINT ( 'NONE',  ( 801.1904061080338124, -212.0891481129653187, -368.3070685750236066 ) ) ;
#4314 = CARTESIAN_POINT ( 'NONE',  ( 441.1634899080286232, 240.0000000000000000, -197.2499999999973852 ) ) ;
#4315 = CARTESIAN_POINT ( 'NONE',  ( 803.4237431249931660, -15.18005720387504631, -331.2633955100225194 ) ) ;
#4316 = CARTESIAN_POINT ( 'NONE',  ( 783.7953271457878373, -128.1908817542439465, 375.1787889125761239 ) ) ;
#4317 = CARTESIAN_POINT ( 'NONE',  ( 814.8230680027162407, -101.8055962898691718, -333.7305795820267917 ) ) ;
#4318 = CARTESIAN_POINT ( 'NONE',  ( 747.2067596250078623, -123.1800572038747106, 352.2312462859687230 ) ) ;
#4319 = CARTESIAN_POINT ( 'NONE',  ( 796.9462024416508257, -324.4527844766013231, -308.9653473494370246 ) ) ;
#4320 = EDGE_CURVE ( 'NONE', #14349, #36535, #20311, .T. ) ;
#4321 = DIRECTION ( 'NONE',  ( 0.000000000000000000, 0.000000000000000000, 1.000000000000000000 ) ) ;
#4322 = CARTESIAN_POINT ( 'NONE',  ( -468.8365100919714337, 256.5000000000001705, -206.1189999999908764 ) ) ;
#4323 = CARTESIAN_POINT ( 'NONE',  ( 759.9864689768902508, -218.0891481129653187, 354.9819416627836404 ) ) ;
#4324 = CARTESIAN_POINT ( 'NONE',  ( 754.3581564841646241, -449.4636090269702322, 316.1443688327762516 ) ) ;
#4325 = CARTESIAN_POINT ( 'NONE',  ( 803.8556311672234642, -417.6237781080499190, -365.6418435158340117 ) ) ;
#4326 = AXIS2_PLACEMENT_3D ( 'NONE', #28800, #38984, #43109 ) ;
#4327 = CARTESIAN_POINT ( 'NONE',  ( 815.2698199232961542, -424.8164208402372992, -342.5225473063383106 ) ) ;
#4328 = DIRECTION ( 'NONE',  ( -0.000000000000000000, 1.000000000000000000, -0.000000000000000000 ) ) ;
#4329 = CARTESIAN_POINT ( 'NONE',  ( 768.8385539511368734, -47.26014174441477422, 306.4236121716840557 ) ) ;
#4330 = VERTEX_POINT ( 'NONE', #12790 ) ;
#4331 = ADVANCED_FACE ( 'NONE', ( #8499 ), #20180, .F. ) ;
#4332 = CARTESIAN_POINT ( 'NONE',  ( 801.3366627262608972, -176.5328690171416213, -353.0897708529566899 ) ) ;
#4333 = CARTESIAN_POINT ( 'NONE',  ( 804.6798772138708955, -15.72551174932958951, 334.6312213355107019 ) ) ;
#4334 = CARTESIAN_POINT ( 'NONE',  ( 754.0944755984390895, -183.6237781080507148, -364.1009440267246760 ) ) ;
#4335 = SURFACE_SIDE_STYLE ('',( #21643 ) ) ;
#4336 = CARTESIAN_POINT ( 'NONE',  ( 748.3538107759620743, -328.7146871989592682, 355.8262568251490165 ) ) ;
#4337 = CARTESIAN_POINT ( 'NONE',  ( 762.1405469898973024, -145.5436935675109851, 357.8594530101016176 ) ) ;
#4338 = ORIENTED_EDGE ( 'NONE', *, *, #32534, .F. ) ;
#4339 = CARTESIAN_POINT ( 'NONE',  ( 785.3141322388236176, -333.7255117493286320, 364.4286716492789537 ) ) ;
#4340 = CARTESIAN_POINT ( 'NONE',  ( 814.2001403089898304, -41.36187538569314626, -347.4397851343538264 ) ) ;
#4341 = VERTEX_POINT ( 'NONE', #41669 ) ;
#4342 = CARTESIAN_POINT ( 'NONE',  ( 755.8990559732751535, -443.4636090269702322, -365.9055244015606831 ) ) ;
#4343 = ORIENTED_EDGE ( 'NONE', *, *, #8870, .T. ) ;
#4344 = ITEM_DEFINED_TRANSFORMATION ( 'NONE', 'NONE', #26044,  #26858 ) ;
#4345 = EDGE_CURVE ( 'NONE', #66, #19810, #34259, .T. ) ;
#4347 = CARTESIAN_POINT ( 'NONE',  ( 798.5707757039680246, -365.4636090269705164, 356.7845633553585003 ) ) ;
#4346 = CARTESIAN_POINT ( 'NONE',  ( 755.5713283507202505, -53.36187538569310362, 334.6858677611754729 ) ) ;
#4348 = CARTESIAN_POINT ( 'NONE',  ( 792.1044303154645831, -300.4527844766012663, -317.8323909638837677 ) ) ;
#4350 = CARTESIAN_POINT ( 'NONE',  ( 744.8212110874229666, -282.8965053807776258, 336.2046728542121627 ) ) ;
#4349 = CARTESIAN_POINT ( 'NONE',  ( 792.3570229623691148, -381.1800572038739006, 373.1304606946836770 ) ) ;
#4351 = CARTESIAN_POINT ( 'NONE',  ( 747.3154664389472828, -67.98741447168742980, 326.4474001241230781 ) ) ;
#4352 = EDGE_CURVE ( 'NONE', #30163, #19609, #2865, .T. ) ;
#4353 = CARTESIAN_POINT ( 'NONE',  ( 761.4292242960306112, -305.4636090269706870, -323.2154366446414429 ) ) ;
#4354 = CARTESIAN_POINT ( 'NONE',  ( 771.2633955100217236, -287.9073299311468759, -363.4237431249939618 ) ) ;
#4355 = FACE_BOUND ( 'NONE', #4290, .T. ) ;
#4356 = CARTESIAN_POINT ( 'NONE',  ( 774.6858677611749044, -129.7255117493292289, -315.5713283507209894 ) ) ;
#4357 = CARTESIAN_POINT ( 'NONE',  ( -858.8365100919713768, 240.0000000000002274, -199.9999999999881481 ) ) ;
#4358 = VERTEX_POINT ( 'NONE', #23170 ) ;
#4359 = CIRCLE ( 'NONE', #27193, 4.999999999999982236 ) ;
#4360 = CARTESIAN_POINT ( 'NONE',  ( 777.5031285880264704, -430.8164208402374129, 374.9108240113588408 ) ) ;
#4361 = CARTESIAN_POINT ( 'NONE',  ( 989.9999999999992042, -590.0000000000001137, 360.0000000000000000 ) ) ;
#4362 = CARTESIAN_POINT ( 'NONE',  ( 799.9636004259356241, -70.91815448151683654, -311.2241431872006956 ) ) ;
#4363 = CARTESIAN_POINT ( 'NONE',  ( 799.9999999999993179, -512.9681489794448908, -339.9999999999999432 ) ) ;
#4364 = FACE_OUTER_BOUND ( 'NONE', #3074, .T. ) ;
#4365 = CARTESIAN_POINT ( 'NONE',  ( 801.5560724626406000, -264.5545181178798657, 326.7756240680316182 ) ) ;
#4366 = CARTESIAN_POINT ( 'NONE',  ( 804.9363028652555840, -136.2709662947837330, 338.2165204200192079 ) ) ;
#4367 = ORIENTED_EDGE ( 'NONE', *, *, #29445, .F. ) ;
#4368 = CARTESIAN_POINT ( 'NONE',  ( 759.0252816721024374, -120.9982390220565378, -368.0189434323527280 ) ) ;
#4369 = CARTESIAN_POINT ( 'NONE',  ( 803.2186876482843445, -319.9874144716866340, 350.0220218866286928 ) ) ;
#4370 = CARTESIAN_POINT ( 'NONE',  ( 789.5670355615794733, -453.0432664090020012, -363.0970091259334822 ) ) ;
#4371 = EDGE_CURVE ( 'NONE', #30631, #35503, #14730, .T. ) ;
#4372 = CARTESIAN_POINT ( 'NONE',  ( 788.6739635108323228, -55.64542720878963422, 373.9316612368139090 ) ) ;
#4373 = CARTESIAN_POINT ( 'NONE',  ( 792.3570229623688874, -237.1800572038742985, -373.1304606946836202 ) ) ;
#4374 = EDGE_CURVE ( 'NONE', #28460, #35455, #44677, .T. ) ;
#4375 = CARTESIAN_POINT ( 'NONE',  ( 759.7806653035534055, -126.9982390220565094, 324.8639956371180801 ) ) ;
#4376 = CARTESIAN_POINT ( 'NONE',  ( 879.9999999999990905, 479.9999999999998863, -360.0000000000000000 ) ) ;
#4377 = CARTESIAN_POINT ( 'NONE',  ( 771.2368401574024119, -301.4419599262320730, -374.2805881961240857 ) ) ;
#4378 = CARTESIAN_POINT ( 'NONE',  ( 776.2046728542105711, -452.1908817542428665, 304.8212110874238761 ) ) ;
#4379 = CARTESIAN_POINT ( 'NONE',  ( 815.2698199232961542, -328.8164208402375834, -342.5225473063383106 ) ) ;
#4380 = PLANE ( 'NONE',  #16549 ) ;
#4381 = CARTESIAN_POINT ( 'NONE',  ( 802.7791456095903868, -388.7146871989592114, 329.0155153010375102 ) ) ;
#4382 = ORIENTED_EDGE ( 'NONE', *, *, #14505, .T. ) ;
#4383 = LINE ( 'NONE', #23199, #26921 ) ;
#4384 = CARTESIAN_POINT ( 'NONE',  ( 785.3687786644884454, -419.3618753856918033, -315.3201227861279676 ) ) ;
#4385 = EDGE_CURVE ( 'NONE', #42899, #637, #19732, .T. ) ;
#4386 = CARTESIAN_POINT ( 'NONE',  ( 770.0799878456142551, -61.98741447168745822, 362.9823548866085616 ) ) ;
#4387 = CARTESIAN_POINT ( 'NONE',  ( 795.6651683502461765, -82.71468719896012090, -371.3240766477733814 ) ) ;
#4388 = LINE ( 'NONE', #28217, #21097 ) ;
#4389 = CARTESIAN_POINT ( 'NONE',  ( 752.4576283171824116, -189.0783235625961822, 317.7880784355627952 ) ) ;
#4390 = CARTESIAN_POINT ( 'NONE',  ( 801.9419747391806368, -42.45278447660223264, 351.9812246680014027 ) ) ;
#4391 = AXIS2_PLACEMENT_3D ( 'NONE', #36742, #36069, #5101 ) ;
#4392 = ORIENTED_EDGE ( 'NONE', *, *, #41885, .F. ) ;
#4393 = CARTESIAN_POINT ( 'NONE',  ( 761.2382568024794409, -231.6237781080504874, -356.9571628226838129 ) ) ;
#4394 = CARTESIAN_POINT ( 'NONE',  ( 758.0580252608178853, -246.4527844766016074, 328.0187753319985404 ) ) ;
#4395 = CARTESIAN_POINT ( 'NONE',  ( 815.1787889125755555, -78.89650538077832209, -343.7953271457877804 ) ) ;
#4396 = CARTESIAN_POINT ( 'NONE',  ( 792.1044303154646968, -348.4527844766012095, 317.8323909638837677 ) ) ;
#4397 = CARTESIAN_POINT ( 'NONE',  ( -786.4999999999993179, -496.5085659523897448, -356.8883017825714319 ) ) ;
#4398 = ADVANCED_FACE ( 'NONE', ( #2173 ), #18900, .F. ) ;
#4399 = VERTEX_POINT ( 'NONE', #16265 ) ;
#4400 = CARTESIAN_POINT ( 'NONE',  ( 786.2694204179717872, -333.2817908451523863, -305.1769319972829067 ) ) ;
#4401 = EDGE_CURVE ( 'NONE', #13363, #45720, #2634, .T. ) ;
#4402 = CARTESIAN_POINT ( 'NONE',  ( 796.9462024416508257, -276.4527844766014368, 308.9653473494370246 ) ) ;
#4403 = CARTESIAN_POINT ( 'NONE',  ( 808.7758568127978833, -4.169232653505813069, 320.0363995740631822 ) ) ;
#4404 = CARTESIAN_POINT ( 'NONE',  ( 790.9844846989617508, -190.3726999360619629, -317.2208543904092721 ) ) ;
#4405 = CARTESIAN_POINT ( 'NONE',  ( 781.8018195045266339, -166.2709662947835909, -365.1927285166406705 ) ) ;
#4406 = CARTESIAN_POINT ( 'NONE',  ( 805.1927285166399315, -376.8164208402375834, -341.8018195045277707 ) ) ;
#4407 = ORIENTED_EDGE ( 'NONE', *, *, #14833, .F. ) ;
#4408 = ORIENTED_EDGE ( 'NONE', *, *, #39387, .F. ) ;
#4409 = CARTESIAN_POINT ( 'NONE',  ( 808.3070685750230950, -282.9982390220558841, 361.1904061080339261 ) ) ;
#4410 = LINE ( 'NONE', #18501, #43969 ) ;
#4411 = CARTESIAN_POINT ( 'NONE',  ( 769.9779781133707957, -211.0999726633346540, 316.7813123517150871 ) ) ;
#4412 = DIRECTION ( 'NONE',  ( 0.000000000000000000, 0.000000000000000000, 1.000000000000000000 ) ) ;
#4413 = CARTESIAN_POINT ( 'NONE',  ( 755.3028492785439312, -159.2817908451529547, 335.9200461376539693 ) ) ;
#4414 = CARTESIAN_POINT ( 'NONE',  ( 762.1405469898971887, -49.54369356751129061, 357.8594530101015607 ) ) ;
#4415 = ORIENTED_EDGE ( 'NONE', *, *, #23048, .T. ) ;
#4416 = CARTESIAN_POINT ( 'NONE',  ( 788.6739635108323228, -415.6454272087885897, -373.9316612368139090 ) ) ;
#4417 = EDGE_CURVE ( 'NONE', #5332, #27330, #8529, .T. ) ;
#4418 = CARTESIAN_POINT ( 'NONE',  ( 772.5602148656447525, -9.725511749329603717, -305.7998596910095443 ) ) ;
#4419 = CARTESIAN_POINT ( 'NONE',  ( 786.2694204179717872, -261.2817908451526705, 305.1769319972829067 ) ) ;
#4420 = VECTOR ( 'NONE', #39707, 1000.000000000000000 ) ;
#4421 = CARTESIAN_POINT ( 'NONE',  ( 793.2243759319678702, -218.5328690171414792, 318.4439275373583200 ) ) ;
#4422 = CARTESIAN_POINT ( 'NONE',  ( 797.8594530101008786, -373.5436935675101040, -322.1405469898980982 ) ) ;
#4423 = DIRECTION ( 'NONE',  ( 8.659560562354807133E-17, 0.7071067811865578978, -0.7071067811865372477 ) ) ;
#4424 = EDGE_CURVE ( 'NONE', #12399, #24210, #3389, .T. ) ;
#4425 = CARTESIAN_POINT ( 'NONE',  ( 804.1105419155481968, -459.8272453906066062, 347.6308680596136469 ) ) ;
#4426 = CARTESIAN_POINT ( 'NONE',  ( 772.4999999999993179, -462.9681489794447771, -310.9526249034443026 ) ) ;
#4427 = CARTESIAN_POINT ( 'NONE',  ( 804.6971507214547046, -243.2817908451526705, -344.0799538623459739 ) ) ;
#4428 = EDGE_CURVE ( 'NONE', #44892, #44015, #21080, .T. ) ;
#4429 = CARTESIAN_POINT ( 'NONE',  ( 815.2698199232961542, -40.81642084023859951, 342.5225473063383106 ) ) ;
#4430 = CARTESIAN_POINT ( 'NONE',  ( 792.3570229623688874, -117.1800572038746964, 373.1304606946836202 ) ) ;
#4431 = DIRECTION ( 'NONE',  ( -0.000000000000000000, 1.000000000000000000, -0.000000000000000000 ) ) ;
#4432 = PLANE ( 'NONE',  #22454 ) ;
#4433 = CARTESIAN_POINT ( 'NONE',  ( 744.6391490659812007, -398.7363362996976548, 338.7502325331110455 ) ) ;
#4434 = CARTESIAN_POINT ( 'NONE',  ( 879.9999999999990905, 479.9999999999998863, 360.0000000000000000 ) ) ;
#4435 = CARTESIAN_POINT ( 'NONE',  ( 763.2262854647970016, -344.6346026584195101, 309.2812353651462445 ) ) ;
#4436 = ADVANCED_FACE ( 'NONE', ( #45133 ), #13034, .T. ) ;
#4437 = CARTESIAN_POINT ( 'NONE',  ( 795.1360043628807261, -308.0891481129650629, -360.2193346964456282 ) ) ;
#4438 = CARTESIAN_POINT ( 'NONE',  ( 911.9749999999993406, 219.9999999999998863, 350.0000000000000000 ) ) ;
#4439 = PRODUCT_RELATED_PRODUCT_CATEGORY ( 'part', '', ( #79 ) ) ;
#4440 = CARTESIAN_POINT ( 'NONE',  ( 785.3687786644884454, -419.3618753856918033, 315.3201227861279676 ) ) ;
#4441 = CARTESIAN_POINT ( 'NONE',  ( 796.1575198192839480, -198.0090635724255606, 359.4546378042384163 ) ) ;
#4442 = CARTESIAN_POINT ( 'NONE',  ( 797.8822607201568644, -54.55451811788054783, -370.1134526219340160 ) ) ;
#4443 = CARTESIAN_POINT ( 'NONE',  ( 775.9200461376533440, -119.8055962898690865, -315.3028492785443291 ) ) ;
#4444 = CARTESIAN_POINT ( 'NONE',  ( 783.7566961878529810, -96.89650538077825104, 305.1792804349288417 ) ) ;
#4445 = CARTESIAN_POINT ( 'NONE',  ( 801.9419747391806368, -450.4527844766009821, 351.9812246680014027 ) ) ;
#4446 = CARTESIAN_POINT ( 'NONE',  ( 764.8639956371174549, -8.089148112965974136, -319.7806653035542013 ) ) ;
#4448 = EDGE_LOOP ( 'NONE', ( #44211, #4584 ) ) ;
#4447 = CARTESIAN_POINT ( 'NONE',  ( 783.0433043558608688, -144.8965053807781089, -315.1538015810313027 ) ) ;
#4449 = CARTESIAN_POINT ( 'NONE',  ( 800.0135310231082713, -110.0891481129656597, -325.0180583372163028 ) ) ;
#4450 = CARTESIAN_POINT ( 'NONE',  ( 755.0488828828309806, -401.8055962898681059, -344.1219089521771934 ) ) ;
#4452 = CARTESIAN_POINT ( 'NONE',  ( 792.1044303154646968, -276.4527844766014368, 317.8323909638837677 ) ) ;
#4451 = CARTESIAN_POINT ( 'NONE',  ( 764.8639956371174549, -248.0891481129651481, 319.7806653035542013 ) ) ;
#4453 = CYLINDRICAL_SURFACE ( 'NONE', #27857, 9.999999999999980460 ) ;
#4454 = VERTEX_POINT ( 'NONE', #37972 ) ;
#4455 = CARTESIAN_POINT ( 'NONE',  ( 805.1927285166397041, -424.8164208402372992, 341.8018195045277707 ) ) ;
#4456 = ORIENTED_EDGE ( 'NONE', *, *, #28091, .T. ) ;
#4457 = CARTESIAN_POINT ( 'NONE',  ( 749.2812353651451076, -198.4527844766017495, 323.2262854647983090 ) ) ;
#4458 = CARTESIAN_POINT ( 'NONE',  ( 799.2566176426618085, -264.0090635724253616, 324.0069404352559559 ) ) ;
#4459 = EDGE_LOOP ( 'NONE', ( #13895, #29449, #40745, #13582, #31975, #23501, #38647, #21754, #20248, #27040, #17573, #26011, #11888 ) ) ;
#4460 = CARTESIAN_POINT ( 'NONE',  ( 787.5531968255692163, -69.82724539060775726, -316.1348686366205811 ) ) ;
#4461 = CARTESIAN_POINT ( 'NONE',  ( 795.6651683502461765, -202.7146871989597514, 371.3240766477733814 ) ) ;
#4462 = CARTESIAN_POINT ( 'NONE',  ( 785.3141322388236176, -261.7255117493288026, -364.4286716492789537 ) ) ;
#4463 = VERTEX_POINT ( 'NONE', #37740 ) ;
#4464 = CARTESIAN_POINT ( 'NONE',  ( 802.1676090361156639, -398.6346026584193396, -327.8955696845344505 ) ) ;
#4465 = CARTESIAN_POINT ( 'NONE',  ( 785.3141322388236176, -45.72551174932949181, -364.4286716492789537 ) ) ;
#4466 = CARTESIAN_POINT ( 'NONE',  ( 799.4546378042377910, -273.0783235625958696, 356.1575198192848006 ) ) ;
#4467 = CARTESIAN_POINT ( 'NONE',  ( 786.4999999999993179, 262.9227088301245203, 634.7515695135432452 ) ) ;
#4468 = DIRECTION ( 'NONE',  ( 0.000000000000000000, -1.000000000000000000, 0.000000000000000000 ) ) ;
#4469 = CARTESIAN_POINT ( 'NONE',  ( 755.5713283507202505, -5.361875385693257279, -334.6858677611754729 ) ) ;
#4470 = FACE_OUTER_BOUND ( 'NONE', #11164, .T. ) ;
#4471 = ORIENTED_EDGE ( 'NONE', *, *, #27831, .T. ) ;
#4472 = CARTESIAN_POINT ( 'NONE',  ( 793.5525998758768083, -295.0999726633343698, -372.6845335610516941 ) ) ;
#4473 = CARTESIAN_POINT ( 'NONE',  ( 752.7379699480933368, -156.0090635724256742, 361.9858362298580232 ) ) ;
#4475 = CARTESIAN_POINT ( 'NONE',  ( 755.3201227861273992, -243.7255117493287742, -345.3687786644892981 ) ) ;
#4474 = CYLINDRICAL_SURFACE ( 'NONE', #18007, 9.999999999999980460 ) ;
#4476 = ADVANCED_FACE ( 'NONE', ( #27345 ), #6329, .F. ) ;
#4477 = CARTESIAN_POINT ( 'NONE',  ( 804.8461984189677878, -146.1908817542438896, -336.9566956441385628 ) ) ;
#4478 = CARTESIAN_POINT ( 'NONE',  ( 745.4481719005789273, -27.72551174932954510, 347.5162901302853129 ) ) ;
#4479 = DIRECTION ( 'NONE',  ( 0.000000000000000000, 0.000000000000000000, -1.000000000000000000 ) ) ;
#4480 = CARTESIAN_POINT ( 'NONE',  ( 756.1443688327750579, -21.62377810805121570, -314.3581564841659315 ) ) ;
#4481 = CARTESIAN_POINT ( 'NONE',  ( 801.1904061080338124, -356.0891481129648355, -368.3070685750236066 ) ) ;
#4482 = DIRECTION ( 'NONE',  ( 0.9164815115825537539, 0.1263042864341373805, 0.3796167358741193709 ) ) ;
#4483 = CARTESIAN_POINT ( 'NONE',  ( 804.4286716492782716, -17.36187538569322086, 345.3141322388244703 ) ) ;
#4484 = CARTESIAN_POINT ( 'NONE',  ( 788.6739635108323228, -271.6454272087889876, 373.9316612368139090 ) ) ;
#4485 = CARTESIAN_POINT ( 'NONE',  ( 811.6461892240364477, -244.7146871989596093, -324.1737431748509835 ) ) ;
#4486 = CARTESIAN_POINT ( 'NONE',  ( 745.7998596910086917, -221.3618753856925707, 332.5602148656461168 ) ) ;
#4487 = CARTESIAN_POINT ( 'NONE',  ( 752.4576283171824116, -429.0783235625953580, -317.7880784355627952 ) ) ;
#4488 = CARTESIAN_POINT ( 'NONE',  ( 786.4999999999993179, -110.5936016518799221, 750.6326042729449455 ) ) ;
#4489 = EDGE_LOOP ( 'NONE', ( #21907, #19475, #16357, #6946 ) ) ;
#4490 = CARTESIAN_POINT ( 'NONE',  ( 756.3353852180819104, -317.9073299311468190, 331.1735550268788302 ) ) ;
#4491 = CARTESIAN_POINT ( 'NONE',  ( 802.9823548866075953, -97.09997266333496668, 330.0799878456151077 ) ) ;
#4492 = CARTESIAN_POINT ( 'NONE',  ( 793.2243759319678702, 21.46713098285774279, -318.4439275373583200 ) ) ;
#4493 = DIRECTION ( 'NONE',  ( -1.880165489482579047E-16, -1.000000000000000000, -0.000000000000000000 ) ) ;
#4494 = PLANE ( 'NONE',  #23255 ) ;
#4496 = CARTESIAN_POINT ( 'NONE',  ( 804.4286716492782716, -377.3618753856920875, 345.3141322388244703 ) ) ;
#4495 = CARTESIAN_POINT ( 'NONE',  ( 760.5453621957607311, -165.0783235625962391, 323.8424801807151425 ) ) ;
#4497 = ORIENTED_EDGE ( 'NONE', *, *, #11378, .T. ) ;
#4498 = CARTESIAN_POINT ( 'NONE',  ( 756.7813123517142913, -307.9874144716866340, -329.9779781133712504 ) ) ;
#4499 = CARTESIAN_POINT ( 'NONE',  ( 762.3223304703356007, -175.5436935675108998, 322.3223304703362828 ) ) ;
#4500 = CARTESIAN_POINT ( 'NONE',  ( 800.1688906516307043, -346.1692326535047641, -369.0717654672308186 ) ) ;
#4501 = DIRECTION ( 'NONE',  ( -0.000000000000000000, -0.000000000000000000, -1.000000000000000000 ) ) ;
#4502 = CARTESIAN_POINT ( 'NONE',  ( 787.5162901302840055, 12.63812461430668321, 305.4481719005792684 ) ) ;
#4503 = ORIENTED_EDGE ( 'NONE', *, *, #34012, .T. ) ;
#4504 = CARTESIAN_POINT ( 'NONE',  ( 756.5762568750052424, -315.1800572038740711, 348.7366044899774238 ) ) ;
#4505 = CARTESIAN_POINT ( 'NONE',  ( 764.0069404352550464, -87.07832356259646645, -359.2566176426627180 ) ) ;
#4506 = DIRECTION ( 'NONE',  ( -0.000000000000000000, 1.000000000000000000, -0.000000000000000000 ) ) ;
#4507 = CARTESIAN_POINT ( 'NONE',  ( 782.5225473063381969, -142.2709662947837330, -375.2698199232970637 ) ) ;
#4508 = VERTEX_POINT ( 'NONE', #15438 ) ;
#4509 = CARTESIAN_POINT ( 'NONE',  ( 803.4237431249931660, -159.1800572038746111, -331.2633955100225194 ) ) ;
#4510 = VERTEX_POINT ( 'NONE', #4798 ) ;
#4511 = CARTESIAN_POINT ( 'NONE',  ( 804.8461984189677878, -434.1908817542430370, -336.9566956441385628 ) ) ;
#4512 = CARTESIAN_POINT ( 'NONE',  ( 764.8639956371174549, 15.91085188703394238, 319.7806653035542013 ) ) ;
#4513 = CARTESIAN_POINT ( 'NONE',  ( 804.7487373415286811, -235.5436935675107293, 364.7487373415288516 ) ) ;
#4514 = CARTESIAN_POINT ( 'NONE',  ( 803.2186876482843445, -175.9874144716871172, 350.0220218866286928 ) ) ;
#4517 = CARTESIAN_POINT ( 'NONE',  ( 805.9055244015594326, -411.6237781080499758, 315.8990559732753240 ) ) ;
#4516 = CARTESIAN_POINT ( 'NONE',  ( 779.9999999999992042, -462.9681489794448339, -339.9999999999999432 ) ) ;
#4515 = CARTESIAN_POINT ( 'NONE',  ( 51.16348990802859475, 230.0000000000000284, -199.9999999999945146 ) ) ;
#4518 = ORIENTED_EDGE ( 'NONE', *, *, #32275, .T. ) ;
#4519 = CARTESIAN_POINT ( 'NONE',  ( 804.4086373105744769, -409.6454272087884760, -333.3843516231986541 ) ) ;
#4520 = CARTESIAN_POINT ( 'NONE',  ( 799.9999999999993179, 205.0000000000000568, -329.9999999999999432 ) ) ;
#4521 = CARTESIAN_POINT ( 'NONE',  ( 778.7629533639073998, -200.7363362996982801, -375.0009284576466371 ) ) ;
#4522 = CARTESIAN_POINT ( 'NONE',  ( 752.7379699480933368, -60.00906357242598688, 361.9858362298580232 ) ) ;
#4524 = CARTESIAN_POINT ( 'NONE',  ( 831.1634899080286232, 259.9999999999998863, -199.9999999999999432 ) ) ;
#4523 = CYLINDRICAL_SURFACE ( 'NONE', #21937, 2.749999999999835687 ) ;
#4525 = CARTESIAN_POINT ( 'NONE',  ( 804.1601925771018387, -319.4419599262320730, -346.5483106153029098 ) ) ;
#4526 = CARTESIAN_POINT ( 'NONE',  ( 200.7583438952258916, 294.6698570112193920, -274.9999999999999432 ) ) ;
#4527 = CARTESIAN_POINT ( 'NONE',  ( 781.2370466360911223, -188.7363362996983085, -304.9990715423533629 ) ) ;
#4528 = PLANE ( 'NONE',  #30383 ) ;
#4529 = FACE_OUTER_BOUND ( 'NONE', #29351, .T. ) ;
#4530 = CARTESIAN_POINT ( 'NONE',  ( 804.6971507214547046, -411.2817908451521589, 344.0799538623459739 ) ) ;
#4531 = CARTESIAN_POINT ( 'NONE',  ( 814.9108240113580450, -232.2709662947834488, -337.5031285880265273 ) ) ;
#4532 = LINE ( 'NONE', #22295, #34179 ) ;
#4533 = CARTESIAN_POINT ( 'NONE',  ( 803.6646147819161570, -17.90732993114776406, -348.8264449731210561 ) ) ;
#4534 = CARTESIAN_POINT ( 'NONE',  ( 814.2805881961230625, -169.6454272087892718, 331.2368401574024119 ) ) ;
#4535 = CARTESIAN_POINT ( 'NONE',  ( 800.1688906516307043, -106.1692326535054889, -369.0717654672308186 ) ) ;
#4536 = CARTESIAN_POINT ( 'NONE',  ( 745.4481719005789273, -123.7255117493292147, 347.5162901302853129 ) ) ;
#4537 = CARTESIAN_POINT ( 'NONE',  ( 814.2001403089898304, -377.3618753856920875, -347.4397851343538264 ) ) ;
#4538 = DIRECTION ( 'NONE',  ( -0.000000000000000000, 1.000000000000000000, -0.000000000000000000 ) ) ;
#4539 = DIRECTION ( 'NONE',  ( -0.000000000000000000, 1.000000000000000000, -0.000000000000000000 ) ) ;
#4540 = CARTESIAN_POINT ( 'NONE',  ( 758.0580252608178853, -222.4527844766016642, 328.0187753319985404 ) ) ;
#4541 = CARTESIAN_POINT ( 'NONE',  ( 760.0363995740630116, -442.9181544815157849, 368.7758568127991907 ) ) ;
#4542 = CARTESIAN_POINT ( 'NONE',  ( 771.2368401574024119, -397.4419599262317320, -374.2805881961240857 ) ) ;
#4543 = CARTESIAN_POINT ( 'NONE',  ( 815.2698199232961542, -448.8164208402371855, -342.5225473063383106 ) ) ;
#4544 = DIRECTION ( 'NONE',  ( -1.000000000000000000, -0.000000000000000000, -0.000000000000000000 ) ) ;
#4545 = CARTESIAN_POINT ( 'NONE',  ( 758.0141637701419768, -15.07832356259669560, 367.2620300519063790 ) ) ;
#4546 = ORIENTED_EDGE ( 'NONE', *, *, #26712, .T. ) ;
#4547 = CARTESIAN_POINT ( 'NONE',  ( 804.9511171171677688, -197.8055962898688733, -335.8780910478229202 ) ) ;
#4548 = CARTESIAN_POINT ( 'NONE',  ( 788.8264449731200330, -21.18005720387502677, 363.6646147819171233 ) ) ;
#4549 = AXIS2_PLACEMENT_3D ( 'NONE', #35131, #31666, #20131 ) ;
#4550 = CARTESIAN_POINT ( 'NONE',  ( 758.0141637701419768, -183.0783235625961538, -367.2620300519063790 ) ) ;
#4551 = CARTESIAN_POINT ( 'NONE',  ( 914.9999999999992042, 74.99999999999984368, 350.0000000000000000 ) ) ;
#4552 = CARTESIAN_POINT ( 'NONE',  ( 808.7758568127978833, -340.1692326535047641, 320.0363995740631822 ) ) ;
#4553 = CARTESIAN_POINT ( 'NONE',  ( 804.9363028652555840, -160.2709662947836762, 338.2165204200192079 ) ) ;
#4554 = CARTESIAN_POINT ( 'NONE',  ( 768.0187753319979720, -80.63460265842029173, -318.0580252608186242 ) ) ;
#4555 = ORIENTED_EDGE ( 'NONE', *, *, #16239, .T. ) ;
#4556 = CARTESIAN_POINT ( 'NONE',  ( 746.7653713866222915, -425.2601417444136018, 351.0478386215610271 ) ) ;
#4557 = CARTESIAN_POINT ( 'NONE',  ( 755.3201227861273992, -147.7255117493291152, -345.3687786644892981 ) ) ;
#4558 = CARTESIAN_POINT ( 'NONE',  ( 788.7366044899766848, -323.9073299311468190, 316.5762568750059813 ) ) ;
#4559 = CARTESIAN_POINT ( 'NONE',  ( 755.2512626584698410, -55.54369356751127640, -315.2512626584710915 ) ) ;
#4560 = EDGE_LOOP ( 'NONE', ( #35172, #23960, #35397, #20708 ) ) ;
#4561 = CARTESIAN_POINT ( 'NONE',  ( 771.3260364891663130, -451.6454272087884192, -306.0683387631859773 ) ) ;
#4562 = ORIENTED_EDGE ( 'NONE', *, *, #23842, .T. ) ;
#4563 = CARTESIAN_POINT ( 'NONE',  ( 793.0897708529556667, -318.5545181178796952, -361.3366627262616362 ) ) ;
#4565 = CARTESIAN_POINT ( 'NONE',  ( 758.4439275373578084, -372.5545181178796383, 353.2243759319684386 ) ) ;
#4564 = CARTESIAN_POINT ( 'NONE',  ( 804.6798772138708955, -63.72551174932939233, 334.6312213355107019 ) ) ;
#4566 = CARTESIAN_POINT ( 'NONE',  ( 785.3687786644884454, -299.3618753856922581, -315.3201227861279676 ) ) ;
#4568 = CARTESIAN_POINT ( 'NONE',  ( 748.3538107759620743, -280.7146871989594956, 355.8262568251490165 ) ) ;
#4567 = CARTESIAN_POINT ( 'NONE',  ( 796.7737145352015204, -380.6346026584192828, 370.7187646348536987 ) ) ;
#4569 = CARTESIAN_POINT ( 'NONE',  ( 755.3028492785439312, -279.2817908451526137, -335.9200461376539693 ) ) ;
#4570 = CARTESIAN_POINT ( 'NONE',  ( 804.4286716492782716, -281.3618753856923718, -345.3141322388244703 ) ) ;
#4571 = CARTESIAN_POINT ( 'NONE',  ( 775.4999999999993179, -365.3551492539851893, -28.13243251470704109 ) ) ;
#4572 = CARTESIAN_POINT ( 'NONE',  ( 771.2633955100217236, -167.9073299311473022, -363.4237431249939618 ) ) ;
#4573 = DIRECTION ( 'NONE',  ( -0.000000000000000000, 1.000000000000000000, -0.000000000000000000 ) ) ;
#4574 = VERTEX_POINT ( 'NONE', #11956 ) ;
#4575 = CARTESIAN_POINT ( 'NONE',  ( 763.0537975583475827, -408.4527844766009252, 371.0346526505627480 ) ) ;
#4577 = DIRECTION ( 'NONE',  ( 1.000000000000000000, -0.000000000000000000, -0.000000000000000000 ) ) ;
#4576 = LINE ( 'NONE', #32529, #15283 ) ;
#4578 = CARTESIAN_POINT ( 'NONE',  ( 766.4474001241216001, -91.09997266333496668, -307.3154664389482491 ) ) ;
#4579 = CARTESIAN_POINT ( 'NONE',  ( 441.1634899080286232, 259.9999999999999432, -191.9749999999972374 ) ) ;
#4580 = LINE ( 'NONE', #26498, #3876 ) ;
#4581 = EDGE_CURVE ( 'NONE', #22016, #14103, #43589, .T. ) ;
#4582 = CARTESIAN_POINT ( 'NONE',  ( 800.9840315886518738, -292.9181544815162397, 354.1144889064786412 ) ) ;
#4583 = CARTESIAN_POINT ( 'NONE',  ( 774.6312213355099630, -143.3618753856927697, 364.6798772138717482 ) ) ;
#4584 = ORIENTED_EDGE ( 'NONE', *, *, #17975, .T. ) ;
#4585 = CARTESIAN_POINT ( 'NONE',  ( 745.7998596910086917, -125.3618753856928834, -332.5602148656461168 ) ) ;
#4586 = CARTESIAN_POINT ( 'NONE',  ( 765.8855110935204493, -310.1692326535048778, 319.0159684113471599 ) ) ;
#4587 = CARTESIAN_POINT ( 'NONE',  ( -959.5497976682736407, 120.6654763175833693, 350.0000000000000000 ) ) ;
#4588 = CARTESIAN_POINT ( 'NONE',  ( 802.2119215644370342, -78.00906357242591582, 367.5423716828165084 ) ) ;
#4589 = CARTESIAN_POINT ( 'NONE',  ( 814.2001403089898304, -281.3618753856923718, -347.4397851343538264 ) ) ;
#4590 = CARTESIAN_POINT ( 'NONE',  ( 778.2165204200184689, -118.8164208402383508, 364.9363028652563230 ) ) ;
#4591 = CARTESIAN_POINT ( 'NONE',  ( 749.8865473780648472, -308.5328690171412518, -322.1177392798429082 ) ) ;
#4592 = CARTESIAN_POINT ( 'NONE',  ( 793.0897708529556667, -6.554518117880697048, 361.3366627262616362 ) ) ;
#4593 = CARTESIAN_POINT ( 'NONE',  ( 787.4397851343537695, -357.7255117493285184, -374.2001403089903988 ) ) ;
#4594 = CARTESIAN_POINT ( 'NONE',  ( 759.9999999999992042, -512.9681489794448908, -329.9999999999999432 ) ) ;
#4595 = CARTESIAN_POINT ( 'NONE',  ( 795.9930595647434757, -387.0783235625955285, 320.7433823573372820 ) ) ;
#4596 = ORIENTED_EDGE ( 'NONE', *, *, #18756, .T. ) ;
#4597 = CARTESIAN_POINT ( 'NONE',  ( 794.9819416627830151, -420.9982390220555999, -319.9864689768909898 ) ) ;
#4598 = CARTESIAN_POINT ( 'NONE',  ( 792.1044303154645831, -228.4527844766015789, -317.8323909638837677 ) ) ;
#4599 = CARTESIAN_POINT ( 'NONE',  ( 766.5853460496234675, -85.98741447168738716, -372.3518521366060554 ) ) ;
#4600 = CARTESIAN_POINT ( 'NONE',  ( -598.8365100919716042, 260.0000000000001705, -199.9999999999899671 ) ) ;
#4601 = CARTESIAN_POINT ( 'NONE',  ( 810.1134526219336749, -248.5328690171414223, 357.8822607201570349 ) ) ;
#4602 = CARTESIAN_POINT ( 'NONE',  ( 791.9812246680005501, -44.63460265842040542, 361.9419747391813189 ) ) ;
#4603 = CARTESIAN_POINT ( 'NONE',  ( 786.6156483768007774, -241.4419599262322720, -315.5913626894246136 ) ) ;
#4604 = CARTESIAN_POINT ( 'NONE',  ( 794.9819416627830151, -228.9982390220561683, 319.9864689768909898 ) ) ;
#4605 = CARTESIAN_POINT ( 'NONE',  ( 815.0009284576459549, -78.35105083532376113, -338.7629533639073429 ) ) ;
#4606 = CARTESIAN_POINT ( 'NONE',  ( 809.2691622578233819, -452.9681489794448908, -335.3267997378328005 ) ) ;
#4607 = ORIENTED_EDGE ( 'NONE', *, *, #43372, .F. ) ;
#4608 = CARTESIAN_POINT ( 'NONE',  ( 783.7953271457878373, -344.1908817542433212, -375.1787889125761239 ) ) ;
#4609 = CARTESIAN_POINT ( 'NONE',  ( 767.6429770376291799, -297.1800572038741279, 306.8695393053162093 ) ) ;
#4610 = ADVANCED_FACE ( 'NONE', ( #4004 ), #6555, .T. ) ;
#4611 = CARTESIAN_POINT ( 'NONE',  ( 786.2056067578752163, -35.80559628986934229, 374.4686193811670023 ) ) ;
#4612 = CARTESIAN_POINT ( 'NONE',  ( 760.7433823573367135, -180.0090635724255890, -355.9930595647440441 ) ) ;
#4613 = CARTESIAN_POINT ( 'NONE',  ( 758.0580252608178853, -174.4527844766018063, -328.0187753319985404 ) ) ;
#4614 = CARTESIAN_POINT ( 'NONE',  ( 803.4237431249931660, -375.1800572038739574, -331.2633955100225194 ) ) ;
#4615 = ORIENTED_EDGE ( 'NONE', *, *, #44639, .T. ) ;
#4616 = CARTESIAN_POINT ( 'NONE',  ( 783.0433043558608688, 23.10349461922137237, -315.1538015810313027 ) ) ;
#4617 = EDGE_LOOP ( 'NONE', ( #37789, #37136, #11659, #3650 ) ) ;
#4618 = CARTESIAN_POINT ( 'NONE',  ( 804.7487373415286811, -307.5436935675104451, 364.7487373415288516 ) ) ;
#4619 = FACE_OUTER_BOUND ( 'NONE', #21389, .T. ) ;
#4620 = CARTESIAN_POINT ( 'NONE',  ( 804.1105419155481968, -219.8272453906073167, 347.6308680596136469 ) ) ;
#4621 = CARTESIAN_POINT ( 'NONE',  ( 804.1601925771018387, -367.4419599262319025, 346.5483106153029098 ) ) ;
#4622 = EDGE_CURVE ( 'NONE', #10881, #28279, #27703, .T. ) ;
#4623 = CARTESIAN_POINT ( 'NONE',  ( 919.9999999999993179, 219.9999999999998863, 360.0000000000000000 ) ) ;
#4624 = EDGE_CURVE ( 'NONE', #33095, #38247, #27804, .T. ) ;
#4625 = CARTESIAN_POINT ( 'NONE',  ( 805.2837595273609850, -194.7363362996982517, 340.5290396650784714 ) ) ;
#4626 = CARTESIAN_POINT ( 'NONE',  ( 781.7834795799800531, -58.81642084023854267, 315.0636971347436202 ) ) ;
#4627 = EDGE_LOOP ( 'NONE', ( #36019, #24779, #36652, #33925, #45163, #24094 ) ) ;
#4628 = CARTESIAN_POINT ( 'NONE',  ( 766.4474001241216001, -403.0999726633339719, -307.3154664389482491 ) ) ;
#4629 = VECTOR ( 'NONE', #39478, 1000.000000000000000 ) ;
#4630 = CARTESIAN_POINT ( 'NONE',  ( 746.8695393053151292, -5.907329931147799584, -327.6429770376306578 ) ) ;
#4631 = CARTESIAN_POINT ( 'NONE',  ( 814.2805881961230625, -265.6454272087889876, 331.2368401574024119 ) ) ;
#4632 = CARTESIAN_POINT ( 'NONE',  ( 754.8983024940795303, -210.8965053807778816, 336.9254006560228163 ) ) ;
#4633 = CARTESIAN_POINT ( 'NONE',  ( 778.2165204200184689, -406.8164208402375266, -364.9363028652563230 ) ) ;
#4634 = CARTESIAN_POINT ( 'NONE',  ( -26.63011601220122060, -513.1383975375929367, -349.9999999999999432 ) ) ;
#4635 = CARTESIAN_POINT ( 'NONE',  ( 803.4237431249931660, 8.819942796124882634, 331.2633955100225194 ) ) ;
#4636 = FILL_AREA_STYLE_COLOUR ( '', #7524 ) ;
#4637 = CARTESIAN_POINT ( 'NONE',  ( 769.0155153010367712, -250.3726999360618208, -362.7791456095907279 ) ) ;
#4638 = CARTESIAN_POINT ( 'NONE',  ( 758.8095938919642549, -56.08914811296580893, 311.6929314249763365 ) ) ;
#4639 = CARTESIAN_POINT ( 'NONE',  ( 747.2067596250078623, -123.1800572038747106, 352.2312462859687230 ) ) ;
#4640 = FACE_OUTER_BOUND ( 'NONE', #16546, .T. ) ;
#4641 = CARTESIAN_POINT ( 'NONE',  ( 799.9999999999993179, 205.0000000000000568, 360.0000000000000000 ) ) ;
#4642 = EDGE_CURVE ( 'NONE', #6318, #39517, #7809, .T. ) ;
#4643 = CARTESIAN_POINT ( 'NONE',  ( 746.4236121716829757, -399.8272453906067767, 328.8385539511384650 ) ) ;
#4644 = CARTESIAN_POINT ( 'NONE',  ( 745.7194118038753459, -397.6454272087885329, 348.7631598425976449 ) ) ;
#4645 = EDGE_CURVE ( 'NONE', #13769, #7179, #33603, .T. ) ;
#4646 = CARTESIAN_POINT ( 'NONE',  ( 919.9999999999993179, 154.9999999999998863, 360.0000000000000000 ) ) ;
#4647 = CARTESIAN_POINT ( 'NONE',  ( 814.2001403089898304, -377.3618753856920875, 347.4397851343538264 ) ) ;
#4648 = CARTESIAN_POINT ( 'NONE',  ( 803.4237431249931660, -303.1800572038740711, -331.2633955100225194 ) ) ;
#4649 = CARTESIAN_POINT ( 'NONE',  ( 754.8072714833581358, -412.8164208402372992, 338.1981804954720587 ) ) ;
#4650 = CARTESIAN_POINT ( 'NONE',  ( 790.0220218866281812, -175.0999726633346825, 363.2186876482849129 ) ) ;
#4651 = CARTESIAN_POINT ( 'NONE',  ( 793.5525998758768083, -79.09997266333503774, -372.6845335610516941 ) ) ;
#4652 = CARTESIAN_POINT ( 'NONE',  ( 803.8651313633788504, -125.2601417444145255, -332.4468031744301015 ) ) ;
#4653 = CARTESIAN_POINT ( 'NONE',  ( 801.9858362298568863, -147.0783235625962959, 312.7379699480935642 ) ) ;
#4654 = CARTESIAN_POINT ( 'NONE',  ( 788.7366044899766848, -443.9073299311464780, 316.5762568750059813 ) ) ;
#4655 = CARTESIAN_POINT ( 'NONE',  ( 802.1676090361156639, -38.63460265842041252, -327.8955696845344505 ) ) ;
#4656 = CARTESIAN_POINT ( 'NONE',  ( 760.5453621957607311, -141.0783235625962959, -323.8424801807151425 ) ) ;
#4657 = CARTESIAN_POINT ( 'NONE',  ( 804.4286716492782716, -113.3618753856929260, -345.3141322388244703 ) ) ;
#4658 = CARTESIAN_POINT ( 'NONE',  ( 780.5290396650775619, -420.3510508353225532, -365.2837595273619513 ) ) ;
#4660 = CARTESIAN_POINT ( 'NONE',  ( 797.8594530101009923, -253.5436935675105588, 322.1405469898982119 ) ) ;
#4659 = CARTESIAN_POINT ( 'NONE',  ( 785.3141322388236176, -261.7255117493288026, 364.4286716492789537 ) ) ;
#4661 = CIRCLE ( 'NONE', #30461, 7.999999999999785061 ) ;
#4662 = DIRECTION ( 'NONE',  ( -0.000000000000000000, 1.000000000000000000, -0.000000000000000000 ) ) ;
#4663 = ORIENTED_EDGE ( 'NONE', *, *, #37891, .T. ) ;
#4664 = CARTESIAN_POINT ( 'NONE',  ( 798.7617431975189675, 20.37622189194865285, 323.0428371773161871 ) ) ;
#4665 = AXIS2_PLACEMENT_3D ( 'NONE', #6019, #16420, #40468 ) ;
#4666 = EDGE_CURVE ( 'NONE', #18328, #5387, #37183, .T. ) ;
#4667 = ORIENTED_EDGE ( 'NONE', *, *, #6862, .F. ) ;
#4668 =( NAMED_UNIT ( * ) SI_UNIT ( $, .STERADIAN. ) SOLID_ANGLE_UNIT ( ) );
#4669 = CARTESIAN_POINT ( 'NONE',  ( 814.2001403089898304, -185.3618753856926844, 347.4397851343538264 ) ) ;
#4670 = ADVANCED_FACE ( 'NONE', ( #28490 ), #42807, .F. ) ;
#4671 = CARTESIAN_POINT ( 'NONE',  ( 757.0176451133909268, -277.0999726633344267, 349.9200121543848354 ) ) ;
#4672 = ORIENTED_EDGE ( 'NONE', *, *, #59, .T. ) ;
#4673 = CARTESIAN_POINT ( 'NONE',  ( 757.4527132478984868, -88.37269993606226137, -329.1273215169538844 ) ) ;
#4674 = CARTESIAN_POINT ( 'NONE',  ( 788.7631598425961101, -217.4419599262324141, 305.7194118038759143 ) ) ;
#4675 = CARTESIAN_POINT ( 'NONE',  ( 762.1405469898973024, -265.5436935675106156, -357.8594530101016176 ) ) ;
#4676 = ORIENTED_EDGE ( 'NONE', *, *, #36243, .T. ) ;
#4677 = CARTESIAN_POINT ( 'NONE',  ( 788.8264449731200330, -405.1800572038737300, -363.6646147819171233 ) ) ;
#4678 = CARTESIAN_POINT ( 'NONE',  ( 804.9363028652555840, -40.27096629478405987, -338.2165204200192079 ) ) ;
#4679 = VECTOR ( 'NONE', #30619, 1000.000000000000000 ) ;
#4680 = CARTESIAN_POINT ( 'NONE',  ( 790.8726784830453198, -250.7146871989595809, 362.5472867521010585 ) ) ;
#4681 = DIRECTION ( 'NONE',  ( 1.000000000000000000, 0.000000000000000000, 0.000000000000000000 ) ) ;
#4682 = FACE_BOUND ( 'NONE', #31928, .T. ) ;
#4683 = EDGE_CURVE ( 'NONE', #30422, #8509, #29098, .T. ) ;
#4684 = CARTESIAN_POINT ( 'NONE',  ( 814.2805881961230625, -25.64542720878973014, -331.2368401574024119 ) ) ;
#4685 = DIRECTION ( 'NONE',  ( 1.000000000000000000, 0.000000000000000000, 0.000000000000000000 ) ) ;
#4686 = ORIENTED_EDGE ( 'NONE', *, *, #26628, .F. ) ;
#4687 = CARTESIAN_POINT ( 'NONE',  ( 814.4686193811664907, -315.2817908451525000, -346.2056067578752732 ) ) ;
#4688 = CARTESIAN_POINT ( 'NONE',  ( 814.4686193811664907, -171.2817908451529263, 346.2056067578752732 ) ) ;
#4690 = CARTESIAN_POINT ( 'NONE',  ( 803.6646147819161570, -257.9073299311469896, -348.8264449731210561 ) ) ;
#4689 = DIRECTION ( 'NONE',  ( 1.000000000000000000, 0.000000000000000000, -0.000000000000000000 ) ) ;
#4691 = DIRECTION ( 'NONE',  ( -0.000000000000000000, 1.000000000000000000, -0.000000000000000000 ) ) ;
#4692 = CARTESIAN_POINT ( 'NONE',  ( 796.9571628226829034, -143.4636090269711701, -321.2382568024804641 ) ) ;
#4693 = LINE ( 'NONE', #17881, #18176 ) ;
#4694 = CARTESIAN_POINT ( 'NONE',  ( 787.4397851343537695, -357.7255117493285184, -374.2001403089903988 ) ) ;
#4695 = DIRECTION ( 'NONE',  ( 1.000000000000000000, 0.000000000000000000, 0.000000000000000000 ) ) ;
#4696 = CARTESIAN_POINT ( 'NONE',  ( 804.9363028652555840, -40.27096629478405987, 338.2165204200192079 ) ) ;
#4697 = CIRCLE ( 'NONE', #30499, 2.749999999999863665 ) ;
#4698 = CARTESIAN_POINT ( 'NONE',  ( 815.3608509340175488, -290.7363362996980527, 341.2497674668889545 ) ) ;
#4699 = CARTESIAN_POINT ( 'NONE',  ( 764.3348316497523456, -238.7146871989596661, -308.6759233522265617 ) ) ;
#4700 = CARTESIAN_POINT ( 'NONE',  ( 777.4774526936600978, -274.2709662947833067, 304.7301800767027657 ) ) ;
#4701 = CARTESIAN_POINT ( 'NONE',  ( 758.8095938919642549, 15.91085188703394238, -311.6929314249763365 ) ) ;
#4702 = DIRECTION ( 'NONE',  ( 0.000000000000000000, -1.000000000000000000, 0.000000000000000000 ) ) ;
#4703 = VERTEX_POINT ( 'NONE', #24544 ) ;
#4704 = CARTESIAN_POINT ( 'NONE',  ( 774.6312213355099630, -335.3618753856920307, 364.6798772138717482 ) ) ;
#4705 = CARTESIAN_POINT ( 'NONE',  ( 805.2837595273609850, -74.73633629969866377, 340.5290396650784714 ) ) ;
#4706 = CARTESIAN_POINT ( 'NONE',  ( 765.8855110935204493, -22.16923265350575889, -319.0159684113471599 ) ) ;
#4707 = DIRECTION ( 'NONE',  ( -0.000000000000000000, 1.000000000000000000, -0.000000000000000000 ) ) ;
#4708 = CIRCLE ( 'NONE', #30512, 8.000000000000007105 ) ;
#4709 = DIRECTION ( 'NONE',  ( -0.000000000000000000, -0.000000000000000000, 1.000000000000000000 ) ) ;
#4711 = CARTESIAN_POINT ( 'NONE',  ( 795.1360043628807261, -380.0891481129646650, 360.2193346964456282 ) ) ;
#4710 = CARTESIAN_POINT ( 'NONE',  ( 769.1273215169530886, -142.7146871989599219, 317.4527132478988847 ) ) ;
#4712 = ORIENTED_EDGE ( 'NONE', *, *, #26956, .T. ) ;
#4713 = CARTESIAN_POINT ( 'NONE',  ( 794.9819416627830151, -36.99823902205679360, -319.9864689768909898 ) ) ;
#4714 = CARTESIAN_POINT ( 'NONE',  ( 763.2154366446407039, -333.6237781080502600, -321.4292242960311228 ) ) ;
#4715 = CARTESIAN_POINT ( 'NONE',  ( 805.1927285166397041, -160.8164208402382371, 341.8018195045277707 ) ) ;
#4716 = CARTESIAN_POINT ( 'NONE',  ( 744.8212110874229666, -330.8965053807774552, -336.2046728542121627 ) ) ;
#4717 = LINE ( 'NONE', #32913, #7931 ) ;
#4718 = CARTESIAN_POINT ( 'NONE',  ( 805.9055244015594326, -435.6237781080499190, 315.8990559732753240 ) ) ;
#4719 = ORIENTED_EDGE ( 'NONE', *, *, #26079, .F. ) ;
#4720 = CARTESIAN_POINT ( 'NONE',  ( 781.8018195045266339, -358.2709662947829088, 365.1927285166406705 ) ) ;
#4721 = SHAPE_REPRESENTATION ( 'Foot Treadle Lever Assembly', ( #26858 ), #34210 ) ;
#4722 = EDGE_CURVE ( 'NONE', #42387, #22673, #38657, .T. ) ;
#4723 = CARTESIAN_POINT ( 'NONE',  ( 760.5453621957607311, -69.07832356259653750, -323.8424801807151425 ) ) ;
#4724 = ORIENTED_EDGE ( 'NONE', *, *, #38163, .F. ) ;
#4725 = CARTESIAN_POINT ( 'NONE',  ( 757.8323909638827445, -434.6346026584190554, 352.1044303154654358 ) ) ;
#4726 = CARTESIAN_POINT ( 'NONE',  ( 747.2067596250078623, -171.1800572038745543, -352.2312462859687230 ) ) ;
#4727 = EDGE_LOOP ( 'NONE', ( #41516, #15746, #36210, #41308 ) ) ;
#4728 = AXIS2_PLACEMENT_3D ( 'NONE', #30831, #20871, #44925 ) ;
#4729 = CARTESIAN_POINT ( 'NONE',  ( 792.1044303154646968, -180.4527844766017495, -317.8323909638837677 ) ) ;
#4730 = AXIS2_PLACEMENT_3D ( 'NONE', #23873, #5200, #37296 ) ;
#4731 = ORIENTED_EDGE ( 'NONE', *, *, #1735, .F. ) ;
#4732 = CARTESIAN_POINT ( 'NONE',  ( 793.9708237608222134, -430.9181544815157849, -319.2295555964448681 ) ) ;
#4733 = CARTESIAN_POINT ( 'NONE',  ( 759.7806653035534055, -6.998239022056885972, 324.8639956371180801 ) ) ;
#4734 = CARTESIAN_POINT ( 'NONE',  ( 779.4709603349208464, -144.3510508353235764, 314.7162404726379918 ) ) ;
#4735 = EDGE_CURVE ( 'NONE', #23669, #34939, #13949, .T. ) ;
#4737 = LINE ( 'NONE', #25067, #39541 ) ;
#4736 = CARTESIAN_POINT ( 'NONE',  ( 441.1634899080286232, 259.9999999999999432, -199.9999999999972431 ) ) ;
#4738 = ORIENTED_EDGE ( 'NONE', *, *, #25587, .F. ) ;
#4739 = CARTESIAN_POINT ( 'NONE',  ( 758.4439275373578084, -444.5545181178792973, -353.2243759319684386 ) ) ;
#4740 = DIRECTION ( 'NONE',  ( 0.000000000000000000, 0.000000000000000000, 1.000000000000000000 ) ) ;
#4741 = CARTESIAN_POINT ( 'NONE',  ( 768.9521613784389729, -201.8272453906073451, -373.2346286133773106 ) ) ;
#4742 = CARTESIAN_POINT ( 'NONE',  ( 807.2620300519052989, -72.00906357242594424, 318.0141637701419768 ) ) ;
#4744 = DIRECTION ( 'NONE',  ( 0.000000000000000000, 0.000000000000000000, 1.000000000000000000 ) ) ;
#4743 = FACE_OUTER_BOUND ( 'NONE', #11728, .T. ) ;
#4745 = CARTESIAN_POINT ( 'NONE',  ( 793.2243759319678702, -314.5328690171411949, -318.4439275373583200 ) ) ;
#4746 = LINE ( 'NONE', #39656, #17406 ) ;
#4747 = CARTESIAN_POINT ( 'NONE',  ( 744.6391490659812007, -182.7363362996983369, -338.7502325331110455 ) ) ;
#4748 = CARTESIAN_POINT ( 'NONE',  ( 311.1634899080286232, 256.5000000000000000, -199.9999999999963336 ) ) ;
#4749 = DIRECTION ( 'NONE',  ( 1.892425610156518354E-16, 1.000000000000000000, -0.000000000000000000 ) ) ;
#4750 = CARTESIAN_POINT ( 'NONE',  ( 801.5560724626406000, -408.5545181178794110, 326.7756240680316182 ) ) ;
#4751 = VECTOR ( 'NONE', #28100, 1000.000000000000000 ) ;
#4752 = CARTESIAN_POINT ( 'NONE',  ( 815.2698199232962679, -256.8164208402379245, -342.5225473063383674 ) ) ;
#4753 = CARTESIAN_POINT ( 'NONE',  ( 763.8424801807145741, -234.0090635724255037, 320.5453621957614700 ) ) ;
#4754 = CARTESIAN_POINT ( 'NONE',  ( 51.16348990802859475, 240.0000000000000568, -199.9999999999945146 ) ) ;
#4755 = CARTESIAN_POINT ( 'NONE',  ( 785.3141322388236176, -21.72551174932956641, -364.4286716492789537 ) ) ;
#4756 = CARTESIAN_POINT ( 'NONE',  ( 812.3518521366052028, -169.0999726633347393, 326.5853460496235243 ) ) ;
#4757 = CARTESIAN_POINT ( 'NONE',  ( 749.8865473780648472, -116.5328690171418202, -322.1177392798429082 ) ) ;
#4758 = CARTESIAN_POINT ( 'NONE',  ( 787.4397851343537695, -117.7255117493292715, 374.2001403089903988 ) ) ;
#4759 = CARTESIAN_POINT ( 'NONE',  ( 758.8095938919642549, -368.0891481129647786, -311.6929314249763365 ) ) ;
#4760 = CARTESIAN_POINT ( 'NONE',  ( -208.8365100919714052, 260.0000000000001137, -191.9749999999926899 ) ) ;
#4761 = CARTESIAN_POINT ( 'NONE',  ( 919.9999999999993179, 154.9999999999998863, -360.0000000000000000 ) ) ;
#4762 = CARTESIAN_POINT ( 'NONE',  ( 797.6776695296629214, -235.5436935675107293, 357.6776695296636603 ) ) ;
#4763 = VECTOR ( 'NONE', #3276, 1000.000000000000000 ) ;
#4764 = CARTESIAN_POINT ( 'NONE',  ( 760.7433823573367135, -36.00906357242605793, 355.9930595647440441 ) ) ;
#4765 = CARTESIAN_POINT ( 'NONE',  ( 762.3223304703356007, -391.5436935675101608, -322.3223304703362828 ) ) ;
#4766 = CARTESIAN_POINT ( 'NONE',  ( 815.3608509340175488, -2.736336299698892027, -341.2497674668889545 ) ) ;
#4767 = CARTESIAN_POINT ( 'NONE',  ( 1238.921997096861332, 240.0000000000000568, -244.9999999999999716 ) ) ;
#4768 = CARTESIAN_POINT ( 'NONE',  ( 756.1443688327750579, -21.62377810805121570, 314.3581564841659315 ) ) ;
#4769 = ORIENTED_EDGE ( 'NONE', *, *, #9705, .F. ) ;
#4770 = CARTESIAN_POINT ( 'NONE',  ( 770.0799878456142551, -205.9874144716870035, -362.9823548866085616 ) ) ;
#4771 = CARTESIAN_POINT ( 'NONE',  ( 792.1044303154645831, -36.45278447660223975, 317.8323909638837677 ) ) ;
#4772 = CARTESIAN_POINT ( 'NONE',  ( 815.1787889125755555, -222.8965053807778531, -343.7953271457877804 ) ) ;
#4773 = PRESENTATION_STYLE_ASSIGNMENT (( #11719 ) ) ;
#4774 = CARTESIAN_POINT ( 'NONE',  ( 768.8385539511368734, -359.2601417444137724, 306.4236121716840557 ) ) ;
#4775 = CARTESIAN_POINT ( 'NONE',  ( 797.8594530101008786, -85.54369356751118403, -322.1405469898980982 ) ) ;
#4776 = EDGE_LOOP ( 'NONE', ( #38412, #25645 ) ) ;
#4777 = AXIS2_PLACEMENT_3D ( 'NONE', #19582, #20038, #34115 ) ;
#4778 = CARTESIAN_POINT ( 'NONE',  ( 749.8865473780648472, -428.5328690171409107, 322.1177392798429082 ) ) ;
#4779 = CARTESIAN_POINT ( 'NONE',  ( 800.0135310231082713, -350.0891481129648923, 325.0180583372163028 ) ) ;
#4780 = AXIS2_PLACEMENT_3D ( 'NONE', #5364, #25726, #15110 ) ;
#4781 = CARTESIAN_POINT ( 'NONE',  ( 801.1904061080336987, -92.08914811296568814, -368.3070685750235498 ) ) ;
#4782 = ADVANCED_FACE ( 'NONE', ( #3778 ), #11166, .T. ) ;
#4783 = ORIENTED_EDGE ( 'NONE', *, *, #20154, .T. ) ;
#4784 = CARTESIAN_POINT ( 'NONE',  ( 759.0159684113467620, -16.91815448151702839, -325.8855110935213020 ) ) ;
#4785 = VERTEX_POINT ( 'NONE', #32186 ) ;
#4786 = CARTESIAN_POINT ( 'NONE',  ( 804.4086373105744769, -313.6454272087888171, -333.3843516231986541 ) ) ;
#4788 = CARTESIAN_POINT ( 'NONE',  ( 766.0291762391763086, -370.9181544815159555, 360.7704444035551319 ) ) ;
#4787 = CARTESIAN_POINT ( 'NONE',  ( 759.9864689768902508, -50.08914811296584446, 354.9819416627836404 ) ) ;
#4789 = CARTESIAN_POINT ( 'NONE',  ( 781.8018195045266339, -334.2709662947829656, -365.1927285166406705 ) ) ;
#4791 = CARTESIAN_POINT ( 'NONE',  ( 744.8212110874229666, -306.8965053807775689, 336.2046728542121627 ) ) ;
#4790 = CARTESIAN_POINT ( 'NONE',  ( 812.7932403749906598, -399.1800572038738437, 327.7687537140311633 ) ) ;
#4792 = CARTESIAN_POINT ( 'NONE',  ( 783.7566961878529810, -96.89650538077825104, 305.1792804349288417 ) ) ;
#4793 = CARTESIAN_POINT ( 'NONE',  ( 804.8461984189677878, -290.1908817542434349, -336.9566956441385628 ) ) ;
#4794 = CARTESIAN_POINT ( 'NONE',  ( 781.7834795799800531, -298.8164208402377540, -315.0636971347436202 ) ) ;
#4795 = FACE_BOUND ( 'NONE', #34607, .T. ) ;
#4796 = CARTESIAN_POINT ( 'NONE',  ( 767.8955696845333705, -144.4527844766018632, -362.1676090361162323 ) ) ;
#4797 = AXIS2_PLACEMENT_3D ( 'NONE', #31895, #12938, #19635 ) ;
#4798 = CARTESIAN_POINT ( 'NONE',  ( 571.1634899080285095, 256.4999999999999432, -202.7499999999980673 ) ) ;
#4799 = CARTESIAN_POINT ( 'NONE',  ( 763.2262854647970016, -416.6346026584192259, 309.2812353651462445 ) ) ;
#4801 = DIRECTION ( 'NONE',  ( 0.000000000000000000, 1.000000000000000000, 0.000000000000000000 ) ) ;
#4800 = CARTESIAN_POINT ( 'NONE',  ( 787.4999999999992042, -462.9681489794448339, 370.0000000000000568 ) ) ;
#4802 = CARTESIAN_POINT ( 'NONE',  ( 804.1009440267234822, -95.46360902697132644, -314.0944755984392600 ) ) ;
#4803 = LINE ( 'NONE', #26272, #24105 ) ;
#4804 = DIRECTION ( 'NONE',  ( 1.000000000000000000, 0.000000000000000000, -0.000000000000000000 ) ) ;
#4805 = CARTESIAN_POINT ( 'NONE',  ( 796.1575198192839480, -294.0090635724253048, 359.4546378042384163 ) ) ;
#4806 = CARTESIAN_POINT ( 'NONE',  ( 795.1360043628807261, -140.0891481129654892, 360.2193346964456282 ) ) ;
#4807 = ORIENTED_EDGE ( 'NONE', *, *, #43927, .F. ) ;
#4808 = CIRCLE ( 'NONE', #34301, 30.00000000000008171 ) ;
#4809 = CARTESIAN_POINT ( 'NONE',  ( 767.6429770376291799, -129.1800572038746679, -306.8695393053162093 ) ) ;
#4810 = CARTESIAN_POINT ( 'NONE',  ( 804.9511171171677688, -317.8055962898684470, 335.8780910478229202 ) ) ;
#4811 = DIRECTION ( 'NONE',  ( 1.000000000000000000, -0.000000000000000000, -0.000000000000000000 ) ) ;
#4812 = CIRCLE ( 'NONE', #1148, 8.024999999999948841 ) ;
#4813 = CARTESIAN_POINT ( 'NONE',  ( 747.6481478633932056, -61.09997266333506616, 353.4146539503763620 ) ) ;
#4814 = CARTESIAN_POINT ( 'NONE',  ( 745.0891759886404770, -268.2709662947833067, -342.4968714119734159 ) ) ;
#4815 = AXIS2_PLACEMENT_3D ( 'NONE', #27835, #17202, #41930 ) ;
#4816 = AXIS2_PLACEMENT_3D ( 'NONE', #43754, #4978, #25975 ) ;
#4817 = CARTESIAN_POINT ( 'NONE',  ( 804.7487373415286811, -211.5436935675107861, 364.7487373415288516 ) ) ;
#4818 = CARTESIAN_POINT ( 'NONE',  ( 771.1735550268778070, -129.1800572038746111, 316.3353852180827630 ) ) ;
#4819 = ORIENTED_EDGE ( 'NONE', *, *, #30930, .T. ) ;
#4820 = CARTESIAN_POINT ( 'NONE',  ( 783.7566961878529810, -312.8965053807775689, -305.1792804349288417 ) ) ;
#4821 = CARTESIAN_POINT ( 'NONE',  ( 760.7433823573367135, -12.00906357242613609, 355.9930595647440441 ) ) ;
#4822 = CARTESIAN_POINT ( 'NONE',  ( 810.7187646348534145, -354.4527844766012095, -356.7737145352016341 ) ) ;
#4823 = LINE ( 'NONE', #26048, #23213 ) ;
#4824 = CARTESIAN_POINT ( 'NONE',  ( 801.3366627262608972, -392.5328690171409107, 353.0897708529566899 ) ) ;
#4825 = ORIENTED_EDGE ( 'NONE', *, *, #26674, .F. ) ;
#4826 = CARTESIAN_POINT ( 'NONE',  ( 803.4237431249931660, -423.1800572038737300, -331.2633955100225194 ) ) ;
#4827 = AXIS2_PLACEMENT_3D ( 'NONE', #39235, #28358, #14976 ) ;
#4828 = CARTESIAN_POINT ( 'NONE',  ( 793.4146539503750546, -121.9874144716872593, -307.6481478633938877 ) ) ;
#4829 = DIRECTION ( 'NONE',  ( 0.000000000000000000, 0.000000000000000000, 1.000000000000000000 ) ) ;
#4830 = CARTESIAN_POINT ( 'NONE',  ( 748.3538107759620743, -232.7146871989596377, 355.8262568251490165 ) ) ;
#4831 = CARTESIAN_POINT ( 'NONE',  ( 771.1735550268780344, -57.18005720387490243, 316.3353852180828198 ) ) ;
#4832 = CARTESIAN_POINT ( 'NONE',  ( 755.8398074228967971, -235.4419599262323857, -333.4516893846970333 ) ) ;
#4833 = CARTESIAN_POINT ( 'NONE',  ( 768.0187753319979720, -248.6346026584197659, 318.0580252608186242 ) ) ;
#4834 = CIRCLE ( 'NONE', #6313, 30.00000000000008171 ) ;
#4835 = CARTESIAN_POINT ( 'NONE',  ( 786.2056067578752163, -59.80559628986927834, -374.4686193811670023 ) ) ;
#4836 = CARTESIAN_POINT ( 'NONE',  ( 808.2983282543862060, -452.9681489794448908, -337.2950253338145785 ) ) ;
#4837 = ORIENTED_EDGE ( 'NONE', *, *, #10015, .F. ) ;
#4838 = ORIENTED_EDGE ( 'NONE', *, *, #29496, .T. ) ;
#4839 = CARTESIAN_POINT ( 'NONE',  ( 763.2154366446407039, -69.62377810805107003, 321.4292242960311228 ) ) ;
#4840 = CARTESIAN_POINT ( 'NONE',  ( 744.6391490659812007, -326.7363362996979390, -338.7502325331110455 ) ) ;
#4841 = CIRCLE ( 'NONE', #29926, 2.749999999999919176 ) ;
#4842 = CIRCLE ( 'NONE', #2629, 8.025000000000003908 ) ;
#4843 = CARTESIAN_POINT ( 'NONE',  ( 814.2001403089898304, -305.3618753856922581, 347.4397851343538264 ) ) ;
#4844 = CARTESIAN_POINT ( 'NONE',  ( 801.9858362298568863, -27.07832356259665474, 312.7379699480935642 ) ) ;
#4845 = APPLICATION_CONTEXT ( 'automotive_design' ) ;
#4846 = CARTESIAN_POINT ( 'NONE',  ( 796.1575198192839480, -198.0090635724255606, -359.4546378042384163 ) ) ;
#4847 = CARTESIAN_POINT ( 'NONE',  ( 764.8639956371174549, -200.0891481129653187, -319.7806653035542013 ) ) ;
#4848 = CARTESIAN_POINT ( 'NONE',  ( 774.6858677611749044, -393.7255117493283478, -315.5713283507209894 ) ) ;
#4849 = ORIENTED_EDGE ( 'NONE', *, *, #38917, .F. ) ;
#4850 = CARTESIAN_POINT ( 'NONE',  ( 795.9930595647434757, 20.92167643740319605, -320.7433823573372820 ) ) ;
#4851 = EDGE_LOOP ( 'NONE', ( #36463, #27555, #7077, #13940, #1219, #41795, #40284, #31017, #25069, #41649, #42787 ) ) ;
#4852 = CARTESIAN_POINT ( 'NONE',  ( 745.7998596910086917, -317.3618753856922581, 332.5602148656461168 ) ) ;
#4853 = DIRECTION ( 'NONE',  ( -1.000000000000000000, -0.000000000000000000, 0.000000000000000000 ) ) ;
#4854 = CARTESIAN_POINT ( 'NONE',  ( -66.63011601220125613, -365.3551492539851893, -18.13243251470705886 ) ) ;
#4855 = CARTESIAN_POINT ( 'NONE',  ( 775.8780910478218402, -201.2817908451528126, 364.9511171171680530 ) ) ;
#4856 = CARTESIAN_POINT ( 'NONE',  ( 792.1044303154645831, -36.45278447660223975, 317.8323909638837677 ) ) ;
#4857 = ORIENTED_EDGE ( 'NONE', *, *, #3479, .F. ) ;
#4858 = CARTESIAN_POINT ( 'NONE',  ( 781.2370466360911223, -428.7363362996975980, -304.9990715423533629 ) ) ;
#4859 = CARTESIAN_POINT ( 'NONE',  ( 767.7687537140311633, -23.90732993114773919, -372.7932403749916830 ) ) ;
#4860 = CARTESIAN_POINT ( 'NONE',  ( 756.1348686366196716, -233.2601417444141987, 347.5531968255698416 ) ) ;
#4861 = CIRCLE ( 'NONE', #30681, 8.024999999999948841 ) ;
#4862 = CARTESIAN_POINT ( 'NONE',  ( 800.0135310231082713, -398.0891481129647218, -325.0180583372163028 ) ) ;
#4863 = CARTESIAN_POINT ( 'NONE',  ( 792.1044303154646968, -12.45278447660232324, -317.8323909638837677 ) ) ;
#4864 = CARTESIAN_POINT ( 'NONE',  ( 796.7737145352015204, -428.6346026584192259, 370.7187646348536987 ) ) ;
#4865 = CARTESIAN_POINT ( 'NONE',  ( 311.1634899080286232, 260.0000000000000000, -191.9749999999963279 ) ) ;
#4866 = CARTESIAN_POINT ( 'NONE',  ( 796.9571628226829034, -239.4636090269709143, -321.2382568024804641 ) ) ;
#4867 = CARTESIAN_POINT ( 'NONE',  ( 767.7687537140311633, -167.9073299311473022, -372.7932403749916830 ) ) ;
#4868 = CARTESIAN_POINT ( 'NONE',  ( 810.7187646348534145, -66.45278447660216159, 356.7737145352016341 ) ) ;
#4869 = CARTESIAN_POINT ( 'NONE',  ( 801.1904061080336987, -116.0891481129656029, 368.3070685750235498 ) ) ;
#4870 = CARTESIAN_POINT ( 'NONE',  ( 794.9298647675502707, 16.45630643248849978, -314.4833286358118016 ) ) ;
#4871 = DIRECTION ( 'NONE',  ( -0.000000000000000000, -0.000000000000000000, 1.000000000000000000 ) ) ;
#4872 = PRESENTATION_LAYER_ASSIGNMENT (  '', '', ( #8579 ) ) ;
#4873 = CARTESIAN_POINT ( 'NONE',  ( 802.2119215644370342, -390.0090635724249069, 367.5423716828165084 ) ) ;
#4874 = DIRECTION ( 'NONE',  ( -0.000000000000000000, -0.000000000000000000, 1.000000000000000000 ) ) ;
#4875 = CARTESIAN_POINT ( 'NONE',  ( 751.6929314249748586, -366.9982390220556567, 318.8095938919659034 ) ) ;
#4876 = CARTESIAN_POINT ( 'NONE',  ( 805.1927285166397041, -304.8164208402376403, -341.8018195045277707 ) ) ;
#4877 = ADVANCED_FACE ( 'NONE', ( #21106 ), #42118, .T. ) ;
#4878 = CARTESIAN_POINT ( 'NONE',  ( 800.2193346964447755, -450.9982390220554294, 355.1360043628815788 ) ) ;
#4879 = CARTESIAN_POINT ( 'NONE',  ( 813.5763878283155464, -99.82724539060768620, -351.1614460488615350 ) ) ;
#4880 = CARTESIAN_POINT ( 'NONE',  ( 764.0069404352550464, -111.0783235625964096, -359.2566176426627180 ) ) ;
#4881 = CARTESIAN_POINT ( 'NONE',  ( 759.8311093483677041, -142.1692326535054178, 310.9282345327691814 ) ) ;
#4882 = CARTESIAN_POINT ( 'NONE',  ( 795.1360043628808398, -452.0891481129646081, 360.2193346964456282 ) ) ;
#4883 = CARTESIAN_POINT ( 'NONE',  ( 759.7806653035534055, -30.99823902205680071, -324.8639956371180801 ) ) ;
#4884 = CARTESIAN_POINT ( 'NONE',  ( 800.7704444035546203, -124.1692326535054463, -326.0291762391768771 ) ) ;
#4885 = CARTESIAN_POINT ( 'NONE',  ( 774.6312213355099630, -143.3618753856927697, -364.6798772138717482 ) ) ;
#4886 = CARTESIAN_POINT ( 'NONE',  ( 767.8955696845333705, -120.4527844766019484, 362.1676090361162323 ) ) ;
#4887 = EDGE_CURVE ( 'NONE', #966, #11789, #14409, .T. ) ;
#4888 = CARTESIAN_POINT ( 'NONE',  ( 801.9858362298568863, 20.92167643740319605, -312.7379699480935642 ) ) ;
#4890 = CARTESIAN_POINT ( 'NONE',  ( 765.0180583372156207, -264.9982390220561115, 360.0135310231089534 ) ) ;
#4889 = CARTESIAN_POINT ( 'NONE',  ( 800.0135310231082713, -254.0891481129652334, 325.0180583372163028 ) ) ;
#4891 = EDGE_CURVE ( 'NONE', #1429, #37268, #16571, .T. ) ;
#4892 = CARTESIAN_POINT ( 'NONE',  ( -78.83651009197140525, 240.0000000000000568, -199.9999999999936051 ) ) ;
#4893 = EDGE_LOOP ( 'NONE', ( #22004, #21958, #27948, #5004 ) ) ;
#4894 = CARTESIAN_POINT ( 'NONE',  ( 783.0433043558608688, 23.10349461922137237, 315.1538015810313027 ) ) ;
#4895 = ORIENTED_EDGE ( 'NONE', *, *, #17095, .T. ) ;
#4896 =( NAMED_UNIT ( * ) PLANE_ANGLE_UNIT ( ) SI_UNIT ( $, .RADIAN. ) );
#4897 = CIRCLE ( 'NONE', #14513, 9.999999999999982236 ) ;
#4898 = CARTESIAN_POINT ( 'NONE',  ( 763.2262854647970016, -200.6346026584199365, 309.2812353651462445 ) ) ;
#4899 = CARTESIAN_POINT ( 'NONE',  ( 763.8424801807145741, -306.0090635724252479, 320.5453621957614700 ) ) ;
#4900 = CARTESIAN_POINT ( 'NONE',  ( 803.2186876482843445, -415.9874144716862361, 350.0220218866286928 ) ) ;
#4901 = ORIENTED_EDGE ( 'NONE', *, *, #1802, .F. ) ;
#4902 = CARTESIAN_POINT ( 'NONE',  ( 796.9571628226829034, -95.46360902697132644, -321.2382568024804641 ) ) ;
#4903 = CARTESIAN_POINT ( 'NONE',  ( 759.7806653035535192, -270.9982390220561115, -324.8639956371181370 ) ) ;
#4904 = ORIENTED_EDGE ( 'NONE', *, *, #19574, .F. ) ;
#4905 = CARTESIAN_POINT ( 'NONE',  ( 804.9363028652555840, -400.2709662947828519, -338.2165204200192079 ) ) ;
#4906 = CARTESIAN_POINT ( 'NONE',  ( 768.0187753319979720, -32.63460265842044095, -318.0580252608186242 ) ) ;
#4907 = ADVANCED_FACE ( 'NONE', ( #28024 ), #22684, .T. ) ;
#4908 = CARTESIAN_POINT ( 'NONE',  ( 789.9200121543843807, -265.9874144716867477, 317.0176451133914384 ) ) ;
#4909 = DIRECTION ( 'NONE',  ( -1.000000000000000000, 0.000000000000000000, 0.000000000000000000 ) ) ;
#4910 = DIRECTION ( 'NONE',  ( -0.000000000000000000, 1.000000000000000000, -0.000000000000000000 ) ) ;
#4911 = VECTOR ( 'NONE', #29518, 1000.000000000000000 ) ;
#4912 = CARTESIAN_POINT ( 'NONE',  ( 815.3608509340175488, -26.73633629969882008, -341.2497674668889545 ) ) ;
#4913 = CARTESIAN_POINT ( 'NONE',  ( 911.9999999999993179, 154.9999999999998863, 350.0000000000000000 ) ) ;
#4914 = ORIENTED_EDGE ( 'NONE', *, *, #13446, .T. ) ;
#4915 = CARTESIAN_POINT ( 'NONE',  ( 755.8990559732751535, -323.4636090269706301, -365.9055244015606831 ) ) ;
#4916 = CARTESIAN_POINT ( 'NONE',  ( 793.5525998758768083, -175.0999726633346825, 372.6845335610516941 ) ) ;
#4918 = CARTESIAN_POINT ( 'NONE',  ( 800.0135310231082713, -302.0891481129650629, -325.0180583372163028 ) ) ;
#4917 = CARTESIAN_POINT ( 'NONE',  ( 181.1634899080285948, 256.5000000000000000, -199.9999999999953957 ) ) ;
#4919 = CARTESIAN_POINT ( 'NONE',  ( 989.9999999999992042, 249.9999999999998863, -350.0000000000000000 ) ) ;
#4920 = CARTESIAN_POINT ( 'NONE',  ( 793.9708237608222134, -142.9181544815166376, -319.2295555964448681 ) ) ;
#4921 = CARTESIAN_POINT ( 'NONE',  ( 796.7737145352015204, -20.63460265842048003, 370.7187646348536987 ) ) ;
#4922 = DIRECTION ( 'NONE',  ( 1.000000000000000000, 0.000000000000000000, -0.000000000000000000 ) ) ;
#4923 = CARTESIAN_POINT ( 'NONE',  ( 813.2346286133761168, -5.260141744414903897, -328.9521613784389160 ) ) ;
#4924 = CARTESIAN_POINT ( 'NONE',  ( 744.7301800767020268, -340.8164208402376403, -337.4774526936615189 ) ) ;
#4925 = LINE ( 'NONE', #22028, #32023 ) ;
#4926 = CARTESIAN_POINT ( 'NONE',  ( 785.3141322388236176, -45.72551174932949181, 364.4286716492789537 ) ) ;
#4927 = EDGE_CURVE ( 'NONE', #44845, #9329, #18884, .T. ) ;
#4928 = CARTESIAN_POINT ( 'NONE',  ( 783.7953271457878373, -272.1908817542434917, 375.1787889125761239 ) ) ;
#4929 = CARTESIAN_POINT ( 'NONE',  ( 795.6651683502461765, -250.7146871989595809, -371.3240766477733814 ) ) ;
#4930 = CARTESIAN_POINT ( 'NONE',  ( 804.7487373415286811, -259.5436935675106156, 364.7487373415288516 ) ) ;
#4931 = CARTESIAN_POINT ( 'NONE',  ( 800.1688906516307043, -442.1692326535044231, -369.0717654672308186 ) ) ;
#4932 = AXIS2_PLACEMENT_3D ( 'NONE', #38324, #14069, #28141 ) ;
#4933 = CYLINDRICAL_SURFACE ( 'NONE', #4780, 2.749999999999863665 ) ;
#4934 = ADVANCED_FACE ( 'NONE', ( #40265, #32871 ), #18781, .F. ) ;
#4935 = ORIENTED_EDGE ( 'NONE', *, *, #12607, .F. ) ;
#4936 = CARTESIAN_POINT ( 'NONE',  ( 768.0187753319979720, -344.6346026584195101, 318.0580252608186242 ) ) ;
#4937 = CARTESIAN_POINT ( 'NONE',  ( 796.9571628226829034, -71.46360902697141171, 321.2382568024804641 ) ) ;
#4938 = CARTESIAN_POINT ( 'NONE',  ( 803.2186876482843445, -31.98741447168754348, -350.0220218866286928 ) ) ;
#4939 = AXIS2_PLACEMENT_3D ( 'NONE', #43926, #18779, #15992 ) ;
#4940 = CARTESIAN_POINT ( 'NONE',  ( 772.4999999999993179, -512.9681489794448908, 329.9999999999999432 ) ) ;
#4941 = CARTESIAN_POINT ( 'NONE',  ( 939.9999999999993179, 62.79977829742944095, 207.3621835540873235 ) ) ;
#4942 = CARTESIAN_POINT ( 'NONE',  ( 797.8594530101008786, -397.5436935675100472, 322.1405469898980982 ) ) ;
#4943 = ORIENTED_EDGE ( 'NONE', *, *, #11926, .F. ) ;
#4944 = CARTESIAN_POINT ( 'NONE',  ( 800.2193346964447755, -42.99823902205675807, -355.1360043628815788 ) ) ;
#4945 = EDGE_CURVE ( 'NONE', #40516, #41324, #35818, .T. ) ;
#4946 = CIRCLE ( 'NONE', #1252, 2.749999999999863665 ) ;
#4947 = ADVANCED_FACE ( 'NONE', ( #22451 ), #32643, .F. ) ;
#4948 = CARTESIAN_POINT ( 'NONE',  ( 786.6156483768007774, -313.4419599262320730, -315.5913626894246136 ) ) ;
#4949 = CARTESIAN_POINT ( 'NONE',  ( 781.8018195045266339, -166.2709662947835909, 365.1927285166406705 ) ) ;
#4950 = CARTESIAN_POINT ( 'NONE',  ( 805.9055244015594326, -339.6237781080502600, -315.8990559732753240 ) ) ;
#4951 = DIRECTION ( 'NONE',  ( 0.000000000000000000, 1.000000000000000000, 0.000000000000000000 ) ) ;
#4952 = ORIENTED_EDGE ( 'NONE', *, *, #25815, .F. ) ;
#4953 = CARTESIAN_POINT ( 'NONE',  ( 778.2165204200184689, -358.8164208402375834, 364.9363028652563230 ) ) ;
#4954 = CARTESIAN_POINT ( 'NONE',  ( 759.2295555964440155, -88.16923265350555994, -353.9708237608231229 ) ) ;
#4955 = ORIENTED_EDGE ( 'NONE', *, *, #28981, .F. ) ;
#4956 = CARTESIAN_POINT ( 'NONE',  ( 803.4237431249931660, -447.1800572038736732, 331.2633955100225194 ) ) ;
#4957 = CARTESIAN_POINT ( 'NONE',  ( 754.9967657858570647, -193.5436935675108714, -365.0032342141425374 ) ) ;
#4958 = CARTESIAN_POINT ( 'NONE',  ( 763.0537975583476964, -96.45278447660204790, 371.0346526505628617 ) ) ;
#4959 = ORIENTED_EDGE ( 'NONE', *, *, #14494, .F. ) ;
#4960 = CARTESIAN_POINT ( 'NONE',  ( 791.9812246680005501, -188.6346026584199365, -361.9419747391813189 ) ) ;
#4961 = EDGE_LOOP ( 'NONE', ( #26851, #11042, #642, #17255 ) ) ;
#4962 = VECTOR ( 'NONE', #41227, 1000.000000000000000 ) ;
#4963 = CARTESIAN_POINT ( 'NONE',  ( 796.1575198192839480, -414.0090635724249637, -359.4546378042384163 ) ) ;
#4964 = EDGE_CURVE ( 'NONE', #45518, #8411, #15757, .T. ) ;
#4965 = CARTESIAN_POINT ( 'NONE',  ( 755.3201227861273992, -3.725511749329622813, 345.3687786644892981 ) ) ;
#4966 = CARTESIAN_POINT ( 'NONE',  ( 745.0891759886404770, -220.2709662947834772, 342.4968714119734159 ) ) ;
#4967 = CARTESIAN_POINT ( 'NONE',  ( 760.5453621957607311, -165.0783235625962391, 323.8424801807151425 ) ) ;
#4968 = DIRECTION ( 'NONE',  ( 0.000000000000000000, 0.7071067811865578978, 0.7071067811865372477 ) ) ;
#4969 = ORIENTED_EDGE ( 'NONE', *, *, #2102, .F. ) ;
#4970 = CARTESIAN_POINT ( 'NONE',  ( 804.1105419155481968, -435.8272453906066062, -347.6308680596136469 ) ) ;
#4971 = PLANE ( 'NONE',  #8603 ) ;
#4972 = CARTESIAN_POINT ( 'NONE',  ( 776.2046728542105711, -212.1908817542436623, -304.8212110874238761 ) ) ;
#4973 = CARTESIAN_POINT ( 'NONE',  ( 752.7379699480933368, -84.00906357242590161, 361.9858362298580232 ) ) ;
#4974 = CIRCLE ( 'NONE', #12362, 8.024999999999948841 ) ;
#4976 = CARTESIAN_POINT ( 'NONE',  ( 771.1735550268778070, -201.1800572038744690, -316.3353852180827630 ) ) ;
#4975 = LINE ( 'NONE', #37049, #24120 ) ;
#4977 = CARTESIAN_POINT ( 'NONE',  ( 765.8855110935204493, -334.1692326535047073, -319.0159684113471599 ) ) ;
#4978 = DIRECTION ( 'NONE',  ( -0.000000000000000000, 1.000000000000000000, -0.000000000000000000 ) ) ;
#4979 = CARTESIAN_POINT ( 'NONE',  ( 786.2694204179717872, -213.2817908451527842, -305.1769319972829067 ) ) ;
#4980 = DIRECTION ( 'NONE',  ( -1.000000000000000000, 0.000000000000000000, 0.000000000000000000 ) ) ;
#4981 = CARTESIAN_POINT ( 'NONE',  ( 4.917854562272160638E-14, 260.0000000000000568, 0.000000000000000000 ) ) ;
#4982 = CARTESIAN_POINT ( 'NONE',  ( 805.2837595273609850, -50.73633629969874193, -340.5290396650784714 ) ) ;
#4983 = CARTESIAN_POINT ( 'NONE',  ( 775.8780910478218402, -393.2817908451522726, 364.9511171171680530 ) ) ;
#4984 = CARTESIAN_POINT ( 'NONE',  ( 749.2812353651451076, -246.4527844766016074, -323.2262854647983090 ) ) ;
#4985 = CARTESIAN_POINT ( 'NONE',  ( 784.1219089521767955, -237.2817908451526421, 315.0488828828318333 ) ) ;
#4986 = CARTESIAN_POINT ( 'NONE',  ( -265.7583438952258916, 430.0000000000002842, -244.9999999999999716 ) ) ;
#4987 = CARTESIAN_POINT ( 'NONE',  ( 800.0135310231082713, -14.08914811296595460, -325.0180583372163028 ) ) ;
#4988 = ADVANCED_FACE ( 'NONE', ( #39819 ), #29407, .T. ) ;
#4989 = CARTESIAN_POINT ( 'NONE',  ( 783.7953271457878373, -176.1908817542438328, 375.1787889125761239 ) ) ;
#4990 = CARTESIAN_POINT ( 'NONE',  ( 773.7943932421234194, -119.8055962898690865, -305.5313806188329409 ) ) ;
#4991 = CARTESIAN_POINT ( 'NONE',  ( 782.5225473063381969, -166.2709662947835909, 375.2698199232970637 ) ) ;
#4992 = CARTESIAN_POINT ( 'NONE',  ( 805.0032342141412300, -373.5436935675101040, -314.9967657858571783 ) ) ;
#4993 = DIRECTION ( 'NONE',  ( 0.000000000000000000, 1.000000000000000000, 0.000000000000000000 ) ) ;
#4995 = EDGE_CURVE ( 'NONE', #16409, #17231, #985, .T. ) ;
#4994 = DIRECTION ( 'NONE',  ( 1.000000000000000000, 0.000000000000000000, 0.000000000000000000 ) ) ;
#4996 = CARTESIAN_POINT ( 'NONE',  ( 781.7834795799800531, -226.8164208402380098, 315.0636971347436202 ) ) ;
#4997 = CARTESIAN_POINT ( 'NONE',  ( 761.4292242960306112, -17.46360902697157513, 323.2154366446414429 ) ) ;
#4998 = CARTESIAN_POINT ( 'NONE',  ( 781.7834795799800531, -394.8164208402374697, -315.0636971347436202 ) ) ;
#4999 =( BOUNDED_CURVE ( )  B_SPLINE_CURVE ( 3, ( #44055, #30196, #26957, #16336 ),
 .UNSPECIFIED., .F., .T. ) 
 B_SPLINE_CURVE_WITH_KNOTS ( ( 4, 4 ),
 ( 4.712388980384714543, 4.733441231200429478 ),
 .UNSPECIFIED. ) 
 CURVE ( )  GEOMETRIC_REPRESENTATION_ITEM ( )  RATIONAL_B_SPLINE_CURVE ( ( 1.000000000000000000, 0.9999630672356449868, 0.9999630672356449868, 1.000000000000000000 ) ) 
 REPRESENTATION_ITEM ( '' )  );
#5000 = CARTESIAN_POINT ( 'NONE',  ( 760.0363995740630116, -10.91815448151704793, -368.7758568127991907 ) ) ;
#5001 = CARTESIAN_POINT ( 'NONE',  ( 793.3938497862117174, -453.0432664090020580, -372.3358127763067955 ) ) ;
#5002 = CARTESIAN_POINT ( 'NONE',  ( 747.3154664389472828, -19.98741447168758256, 326.4474001241230781 ) ) ;
#5003 = CARTESIAN_POINT ( 'NONE',  ( 804.6798772138708955, -303.7255117493287457, 334.6312213355107019 ) ) ;
#5004 = ORIENTED_EDGE ( 'NONE', *, *, #26661, .F. ) ;
#5005 = PRODUCT_RELATED_PRODUCT_CATEGORY ( 'part', '', ( #38425 ) ) ;
#5006 = CARTESIAN_POINT ( 'NONE',  ( 770.0799878456142551, -229.9874144716869466, -362.9823548866085616 ) ) ;
#5007 = CARTESIAN_POINT ( 'NONE',  ( 803.4237431249931660, -39.18005720387496638, 331.2633955100225194 ) ) ;
#5008 = CARTESIAN_POINT ( 'NONE',  ( 795.6651683502461765, -226.7146871989596661, -371.3240766477733814 ) ) ;
#5009 = PRESENTATION_STYLE_ASSIGNMENT (( #40572 ) ) ;
#5010 = CARTESIAN_POINT ( 'NONE',  ( 786.2056067578752163, -347.8055962898683333, 374.4686193811670023 ) ) ;
#5011 = EDGE_LOOP ( 'NONE', ( #3763, #40780, #25792, #15417 ) ) ;
#5012 = AXIS2_PLACEMENT_3D ( 'NONE', #28929, #32405, #10686 ) ;
#5013 = CARTESIAN_POINT ( 'NONE',  ( 810.1134526219336749, -416.5328690171409107, 357.8822607201570349 ) ) ;
#5014 = CARTESIAN_POINT ( 'NONE',  ( 804.9363028652555840, -136.2709662947837330, -338.2165204200192079 ) ) ;
#5015 = CARTESIAN_POINT ( 'NONE',  ( 803.6646147819161570, -329.9073299311467053, 348.8264449731210561 ) ) ;
#5016 = CARTESIAN_POINT ( 'NONE',  ( 746.8695393053150156, -77.90732993114757221, -327.6429770376306010 ) ) ;
#5017 = CARTESIAN_POINT ( 'NONE',  ( 804.6798772138710092, -87.72551174932935680, -334.6312213355106451 ) ) ;
#5018 = VERTEX_POINT ( 'NONE', #43479 ) ;
#5019 = CARTESIAN_POINT ( 'NONE',  ( 779.4763451958990572, -8.736336299698871599, -365.0264073115438919 ) ) ;
#5020 = VERTEX_POINT ( 'NONE', #29176 ) ;
#5021 = CARTESIAN_POINT ( 'NONE',  ( 783.0745993439762742, -320.1908817542434349, -365.1016975059196739 ) ) ;
#5022 = CONTEXT_DEPENDENT_SHAPE_REPRESENTATION ( #1343, #38056 ) ;
#5024 = CARTESIAN_POINT ( 'NONE',  ( 804.8461984189677878, -386.1908817542432075, 336.9566956441385628 ) ) ;
#5023 = CARTESIAN_POINT ( 'NONE',  ( 797.6776695296629214, -67.54369356751125508, 357.6776695296636603 ) ) ;
#5027 = CARTESIAN_POINT ( 'NONE',  ( 814.8230680027162407, -317.8055962898684470, 333.7305795820267917 ) ) ;
#5026 = CARTESIAN_POINT ( 'NONE',  ( -786.4999999999993179, -512.9681489794448908, -329.9999999999999432 ) ) ;
#5025 = CARTESIAN_POINT ( 'NONE',  ( 792.2312462859673587, -419.9073299311465348, 307.2067596250082602 ) ) ;
#5028 = CARTESIAN_POINT ( 'NONE',  ( 803.8556311672234642, -105.6237781080509421, 365.6418435158340117 ) ) ;
#5029 = CARTESIAN_POINT ( 'NONE',  ( 772.4468031744293057, -321.8272453906070609, -363.8651313633793620 ) ) ;
#5030 = CARTESIAN_POINT ( 'NONE',  ( 774.6858677611749044, -273.7255117493288026, -315.5713283507209894 ) ) ;
#5031 = CARTESIAN_POINT ( 'NONE',  ( 800.0135310231082713, -158.0891481129655176, -325.0180583372163028 ) ) ;
#5032 = CARTESIAN_POINT ( 'NONE',  ( 796.9462024416508257, -420.4527844766009252, 308.9653473494370246 ) ) ;
#5034 = CARTESIAN_POINT ( 'NONE',  ( 999.9999999999992042, -599.0000000000001137, 359.0000000000000000 ) ) ;
#5033 = CARTESIAN_POINT ( 'NONE',  ( 793.2534793918160858, 16.75597696963228955, 312.9842977579731382 ) ) ;
#5035 = CARTESIAN_POINT ( 'NONE',  ( 745.7194118038753459, -109.6454272087894566, -348.7631598425976449 ) ) ;
#5036 = FACE_OUTER_BOUND ( 'NONE', #40726, .T. ) ;
#5037 = CARTESIAN_POINT ( 'NONE',  ( -200.7583438952259485, 394.6698570112193920, -274.9999999999999432 ) ) ;
#5038 = CARTESIAN_POINT ( 'NONE',  ( 769.0155153010367712, -298.3726999360616787, 362.7791456095907279 ) ) ;
#5039 = ORIENTED_EDGE ( 'NONE', *, *, #37944, .F. ) ;
#5040 = CARTESIAN_POINT ( 'NONE',  ( 812.7932403749906598, -135.1800572038746679, -327.7687537140311633 ) ) ;
#5041 = CARTESIAN_POINT ( 'NONE',  ( 799.9999999999993179, -365.3551492539851893, -18.13243251470705886 ) ) ;
#5042 = VECTOR ( 'NONE', #10545, 1000.000000000000000 ) ;
#5043 = CARTESIAN_POINT ( 'NONE',  ( 744.6391490659812007, -86.73633629969862113, 338.7502325331110455 ) ) ;
#5044 = CARTESIAN_POINT ( 'NONE',  ( 800.9747183278959710, -276.9982390220559978, -311.9810565676471583 ) ) ;
#5045 = CARTESIAN_POINT ( 'NONE',  ( 805.0032342141413437, -445.5436935675099335, -314.9967657858572352 ) ) ;
#5046 = CARTESIAN_POINT ( 'NONE',  ( 762.3223304703356007, -103.5436935675111272, 322.3223304703362828 ) ) ;
#5047 = ORIENTED_EDGE ( 'NONE', *, *, #16809, .T. ) ;
#5048 = CARTESIAN_POINT ( 'NONE',  ( 758.0141637701419768, -327.0783235625956991, -367.2620300519063790 ) ) ;
#5049 = CARTESIAN_POINT ( 'NONE',  ( 767.7687537140311633, -71.90732993114760063, -372.7932403749916830 ) ) ;
#5050 = CARTESIAN_POINT ( 'NONE',  ( 804.6971507214547046, -27.28179084515336328, 344.0799538623459739 ) ) ;
#5051 = CARTESIAN_POINT ( 'NONE',  ( 772.5602148656447525, -345.7255117493285184, -305.7998596910095443 ) ) ;
#5052 = CARTESIAN_POINT ( 'NONE',  ( 311.1634899080286232, 260.0000000000000000, -206.1189999999963050 ) ) ;
#5053 = CARTESIAN_POINT ( 'NONE',  ( 779.4709603349208464, -408.3510508353227806, 314.7162404726379918 ) ) ;
#5054 = ORIENTED_EDGE ( 'NONE', *, *, #31723, .F. ) ;
#5055 = CARTESIAN_POINT ( 'NONE',  ( 786.2056067578752163, -107.8055962898691433, -374.4686193811670023 ) ) ;
#5056 = CARTESIAN_POINT ( 'NONE',  ( 784.4999999999993179, -513.1383975375929367, -369.9999999999999432 ) ) ;
#5057 = CARTESIAN_POINT ( 'NONE',  ( 758.0141637701419768, -255.0783235625958980, 367.2620300519063790 ) ) ;
#5058 = CARTESIAN_POINT ( 'NONE',  ( 804.6798772138710092, -39.72551174932951312, 334.6312213355106451 ) ) ;
#5059 = VERTEX_POINT ( 'NONE', #11629 ) ;
#5060 = CARTESIAN_POINT ( 'NONE',  ( 784.0799538623451781, -227.8055962898687596, -364.6971507214555572 ) ) ;
#5061 = CARTESIAN_POINT ( 'NONE',  ( 767.8955696845333705, -240.4527844766015221, 362.1676090361162323 ) ) ;
#5062 = CARTESIAN_POINT ( 'NONE',  ( 807.5423716828161105, -417.0783235625954148, -362.2119215644372048 ) ) ;
#5063 = CARTESIAN_POINT ( 'NONE',  ( 793.4146539503750546, -73.98741447168741558, -307.6481478633938877 ) ) ;
#5064 = CARTESIAN_POINT ( 'NONE',  ( 799.9999999999993179, 205.0000000000000568, 265.0000000000000000 ) ) ;
#5065 = EDGE_LOOP ( 'NONE', ( #3924, #20115 ) ) ;
#5066 = VERTEX_POINT ( 'NONE', #11847 ) ;
#5067 = CARTESIAN_POINT ( 'NONE',  ( 747.6481478633932056, -373.0999726633340856, -353.4146539503763620 ) ) ;
#5068 = AXIS2_PLACEMENT_3D ( 'NONE', #45558, #1621, #33275 ) ;
#5069 = CARTESIAN_POINT ( 'NONE',  ( 797.8594530101008786, -229.5436935675106440, -322.1405469898980982 ) ) ;
#5070 = CARTESIAN_POINT ( 'NONE',  ( 796.7737145352015204, -308.6346026584195670, 370.7187646348536987 ) ) ;
#5071 = CARTESIAN_POINT ( 'NONE',  ( 814.8230680027162407, -29.80559628986937781, 333.7305795820267917 ) ) ;
#5072 = CARTESIAN_POINT ( 'NONE',  ( 784.1219089521767955, -213.2817908451527842, -315.0488828828318333 ) ) ;
#5073 = CARTESIAN_POINT ( 'NONE',  ( 785.3687786644884454, -179.3618753856927128, -315.3201227861279676 ) ) ;
#5074 = CARTESIAN_POINT ( 'NONE',  ( 805.1927285166399315, -400.8164208402374697, -341.8018195045277707 ) ) ;
#5075 = EDGE_LOOP ( 'NONE', ( #31549, #6184 ) ) ;
#5076 = CARTESIAN_POINT ( 'NONE',  ( 778.1981804954714335, -226.2709662947834204, 314.8072714833589885 ) ) ;
#5077 = ORIENTED_EDGE ( 'NONE', *, *, #5773, .F. ) ;
#5078 = CARTESIAN_POINT ( 'NONE',  ( 751.9810565676468741, -314.0891481129650629, 360.9747183278973921 ) ) ;
#5079 = FACE_OUTER_BOUND ( 'NONE', #5281, .T. ) ;
#5080 = CARTESIAN_POINT ( 'NONE',  ( 783.0433043558608688, -360.8965053807773984, 315.1538015810313027 ) ) ;
#5081 = DIRECTION ( 'NONE',  ( 0.000000000000000000, 0.000000000000000000, 1.000000000000000000 ) ) ;
#5082 = DIRECTION ( 'NONE',  ( -1.000000000000000000, -0.000000000000000000, -0.000000000000000000 ) ) ;
#5083 = CARTESIAN_POINT ( 'NONE',  ( 755.8894580844503253, -207.8272453906073451, 332.3691319403863531 ) ) ;
#5084 = CARTESIAN_POINT ( 'NONE',  ( 771.1735550268778070, -33.18005720387498769, 316.3353852180827630 ) ) ;
#5085 = EDGE_LOOP ( 'NONE', ( #40187, #7693 ) ) ;
#5086 = CARTESIAN_POINT ( 'NONE',  ( 748.6759233522253680, -400.3726999360612808, -324.3348316497537098 ) ) ;
#5087 = CARTESIAN_POINT ( 'NONE',  ( 796.9462024416508257, -36.45278447660224685, -308.9653473494370246 ) ) ;
#5088 = CARTESIAN_POINT ( 'NONE',  ( 764.0069404352550464, -231.0783235625960401, 359.2566176426627180 ) ) ;
#5089 = CARTESIAN_POINT ( 'NONE',  ( 755.0636971347428243, -412.2709662947829088, -341.7834795799807353 ) ) ;
#5090 = CARTESIAN_POINT ( 'NONE',  ( 774.6312213355098493, 0.6381246143067237364, -364.6798772138717482 ) ) ;
#5091 = CARTESIAN_POINT ( 'NONE',  ( 744.7301800767019131, -436.8164208402372992, 337.4774526936615757 ) ) ;
#5092 = DIRECTION ( 'NONE',  ( -0.000000000000000000, 1.000000000000000000, -0.000000000000000000 ) ) ;
#5093 = CARTESIAN_POINT ( 'NONE',  ( 804.4086373105744769, -265.6454272087889876, -333.3843516231986541 ) ) ;
#5094 = CARTESIAN_POINT ( 'NONE',  ( 805.0032342141412300, -157.5436935675108998, -314.9967657858571783 ) ) ;
#5095 = CARTESIAN_POINT ( 'NONE',  ( 782.5225473063381969, -46.27096629478404566, 375.2698199232970637 ) ) ;
#5096 = CARTESIAN_POINT ( 'NONE',  ( 748.9653473494363425, -122.6346026584201354, 356.9462024416521331 ) ) ;
#5097 = CARTESIAN_POINT ( 'NONE',  ( 799.9999999999993179, -512.9681489794448908, 329.9999999999999432 ) ) ;
#5098 = EDGE_CURVE ( 'NONE', #12788, #16603, #29845, .T. ) ;
#5099 = DIRECTION ( 'NONE',  ( 0.000000000000000000, 0.000000000000000000, 1.000000000000000000 ) ) ;
#5100 = VECTOR ( 'NONE', #1406, 1000.000000000000114 ) ;
#5101 = DIRECTION ( 'NONE',  ( 0.000000000000000000, 0.000000000000000000, 1.000000000000000000 ) ) ;
#5102 = CARTESIAN_POINT ( 'NONE',  ( 777.4774526936600978, -370.2709662947831362, 304.7301800767027657 ) ) ;
#5103 = CARTESIAN_POINT ( 'NONE',  ( 756.5762568750052424, -315.1800572038740711, -348.7366044899774238 ) ) ;
#5104 = CARTESIAN_POINT ( 'NONE',  ( 773.3843516231979720, 10.55804007376686826, 364.4086373105754433 ) ) ;
#5105 = CARTESIAN_POINT ( 'NONE',  ( 814.2805881961230625, -97.64542720878949922, -331.2368401574024119 ) ) ;
#5106 = CARTESIAN_POINT ( 'NONE',  ( 803.2186876482843445, -127.9874144716872308, -350.0220218866286928 ) ) ;
#5107 = CARTESIAN_POINT ( 'NONE',  ( 813.2346286133761168, -125.2601417444145255, 328.9521613784389160 ) ) ;
#5108 = CARTESIAN_POINT ( 'NONE',  ( 803.6646147819162707, -425.9073299311463643, 348.8264449731211130 ) ) ;
#5109 = CARTESIAN_POINT ( 'NONE',  ( 759.9864689768902508, -26.08914811296592262, -354.9819416627836404 ) ) ;
#5110 = CARTESIAN_POINT ( 'NONE',  ( 755.8398074228967971, -139.4419599262326699, -333.4516893846970333 ) ) ;
#5111 = CARTESIAN_POINT ( 'NONE',  ( 765.0180583372156207, -120.9982390220565378, 360.0135310231089534 ) ) ;
#5112 = CARTESIAN_POINT ( 'NONE',  ( 754.8983024940795303, -426.8965053807771142, -336.9254006560228163 ) ) ;
#5113 = EDGE_CURVE ( 'NONE', #11672, #33458, #33310, .T. ) ;
#5115 = CARTESIAN_POINT ( 'NONE',  ( 762.3223304703356007, -247.5436935675106724, 322.3223304703362828 ) ) ;
#5114 = CARTESIAN_POINT ( 'NONE',  ( 804.9363028652555840, -256.2709662947834204, 338.2165204200192079 ) ) ;
#5116 = CYLINDRICAL_SURFACE ( 'NONE', #44096, 30.00000000000008171 ) ;
#5117 = VERTEX_POINT ( 'NONE', #43700 ) ;
#5118 = CARTESIAN_POINT ( 'NONE',  ( 791.9812246680005501, -452.6346026584191691, 361.9419747391813189 ) ) ;
#5119 = CARTESIAN_POINT ( 'NONE',  ( 815.3608509340175488, -266.7363362996981095, -341.2497674668889545 ) ) ;
#5120 = ORIENTED_EDGE ( 'NONE', *, *, #17979, .T. ) ;
#5121 = CARTESIAN_POINT ( 'NONE',  ( 0.000000000000000000, 0.000000000000000000, 0.000000000000000000 ) ) ;
#5122 = CARTESIAN_POINT ( 'NONE',  ( 759.0252816721024374, -192.9982390220562820, 368.0189434323527280 ) ) ;
#5123 = CARTESIAN_POINT ( 'NONE',  ( 755.8894580844503253, -303.8272453906071178, 332.3691319403863531 ) ) ;
#5124 = CARTESIAN_POINT ( 'NONE',  ( 798.7617431975189675, -387.6237781080499758, 323.0428371773161871 ) ) ;
#5125 = VERTEX_POINT ( 'NONE', #15541 ) ;
#5126 = CARTESIAN_POINT ( 'NONE',  ( 754.7162404726377645, -86.73633629969862113, -339.4709603349214717 ) ) ;
#5127 = CARTESIAN_POINT ( 'NONE',  ( 759.7806653035535192, -294.9982390220559978, -324.8639956371181370 ) ) ;
#5128 = EDGE_LOOP ( 'NONE', ( #31025, #26277, #29605, #7705 ) ) ;
#5129 = CIRCLE ( 'NONE', #1433, 2.749999999999835687 ) ;
#5130 = CARTESIAN_POINT ( 'NONE',  ( 785.3141322388236176, -405.7255117493283478, -364.4286716492789537 ) ) ;
#5131 = CARTESIAN_POINT ( 'NONE',  ( 795.1360043628807261, -44.08914811296584446, -360.2193346964456282 ) ) ;
#5132 = CARTESIAN_POINT ( 'NONE',  ( 790.8726784830453198, -274.7146871989594388, 362.5472867521010585 ) ) ;
#5133 = CARTESIAN_POINT ( 'NONE',  ( 989.9999999999992042, 62.79977829742938411, 207.3621835540872951 ) ) ;
#5134 = FACE_OUTER_BOUND ( 'NONE', #13937, .T. ) ;
#5135 = CARTESIAN_POINT ( 'NONE',  ( 760.0363995740630116, -10.91815448151704793, -368.7758568127991907 ) ) ;
#5136 = CARTESIAN_POINT ( 'NONE',  ( 772.4999999999993179, -462.9681489794447202, 270.0000000000000568 ) ) ;
#5137 = ORIENTED_EDGE ( 'NONE', *, *, #25151, .F. ) ;
#5138 = CARTESIAN_POINT ( 'NONE',  ( 805.6418435158337843, -317.4636090269706301, -363.8556311672236916 ) ) ;
#5139 = EDGE_CURVE ( 'NONE', #34173, #10227, #7948, .T. ) ;
#5140 = CARTESIAN_POINT ( 'NONE',  ( 766.4474001241216001, -211.0999726633346540, 307.3154664389482491 ) ) ;
#5142 = CARTESIAN_POINT ( 'NONE',  ( 792.1044303154645831, -300.4527844766012663, -317.8323909638837677 ) ) ;
#5141 = LINE ( 'NONE', #19227, #14310 ) ;
#5143 = DIRECTION ( 'NONE',  ( -1.000000000000000000, -0.000000000000000000, -0.000000000000000000 ) ) ;
#5144 = CARTESIAN_POINT ( 'NONE',  ( 755.8894580844503253, -159.8272453906075157, -332.3691319403863531 ) ) ;
#5145 = EDGE_CURVE ( 'NONE', #21201, #6854, #40028, .T. ) ;
#5146 = CARTESIAN_POINT ( 'NONE',  ( 787.5162901302840055, -11.36187538569323863, 305.4481719005792684 ) ) ;
#5147 = CARTESIAN_POINT ( 'NONE',  ( -2.220446049250310809E-13, 479.9999999999994884, 0.000000000000000000 ) ) ;
#5148 = CARTESIAN_POINT ( 'NONE',  ( 745.1769319972822814, -17.80559628986940979, -346.2694204179732083 ) ) ;
#5149 = CARTESIAN_POINT ( 'NONE',  ( 814.9108240113580450, -352.2709662947830225, -337.5031285880265273 ) ) ;
#5150 = CARTESIAN_POINT ( 'NONE',  ( -784.4999999999993179, -110.5936016518799221, 750.6326042729449455 ) ) ;
#5151 = CARTESIAN_POINT ( 'NONE',  ( 755.0636971347428243, -52.27096629478401724, 341.7834795799807353 ) ) ;
#5152 = CARTESIAN_POINT ( 'NONE',  ( 745.5313806188320314, -279.2817908451526137, 333.7943932421247268 ) ) ;
#5153 = CARTESIAN_POINT ( 'NONE',  ( 787.5162901302840055, -275.3618753856923149, 305.4481719005792684 ) ) ;
#5154 = CARTESIAN_POINT ( 'NONE',  ( 814.2001403089898304, 6.638124614306706306, -347.4397851343538264 ) ) ;
#5155 = CARTESIAN_POINT ( 'NONE',  ( -72.71751009197140547, 256.5000000000000568, -199.9999999999936051 ) ) ;
#5156 = CARTESIAN_POINT ( 'NONE',  ( 959.5497976682736407, 239.9999999999998863, -2132.806278688367456 ) ) ;
#5157 = CARTESIAN_POINT ( 'NONE',  ( 778.1981804954714335, -370.2709662947831362, 314.8072714833589885 ) ) ;
#5158 = CARTESIAN_POINT ( 'NONE',  ( 755.8894580844503253, -111.8272453906076151, 332.3691319403863531 ) ) ;
#5159 = CARTESIAN_POINT ( 'NONE',  ( 759.2295555964440155, -16.16923265350578021, -353.9708237608231229 ) ) ;
#5160 = DIRECTION ( 'NONE',  ( 1.000000000000000000, 0.000000000000000000, 0.000000000000000000 ) ) ;
#5161 = CARTESIAN_POINT ( 'NONE',  ( 939.9999999999993179, -600.0000000000001137, -360.0000000000000000 ) ) ;
#5162 = CARTESIAN_POINT ( 'NONE',  ( 778.1981804954714335, -394.2709662947827951, 314.8072714833589885 ) ) ;
#5163 = ORIENTED_EDGE ( 'NONE', *, *, #18237, .F. ) ;
#5164 = CARTESIAN_POINT ( 'NONE',  ( 801.3366627262608972, -344.5328690171410813, -353.0897708529566899 ) ) ;
#5165 = CARTESIAN_POINT ( 'NONE',  ( 774.6312213355099630, -167.3618753856927412, 364.6798772138717482 ) ) ;
#5166 = UNCERTAINTY_MEASURE_WITH_UNIT (LENGTH_MEASURE( 1.000000000000000082E-05 ), #31589, 'distance_accuracy_value', 'NONE');
#5167 = CARTESIAN_POINT ( 'NONE',  ( 749.8865473780648472, -332.5328690171411381, -322.1177392798429082 ) ) ;
#5168 = CARTESIAN_POINT ( 'NONE',  ( -37.63011601220122770, -496.5085659523897448, -356.8883017825714319 ) ) ;
#5169 = VERTEX_POINT ( 'NONE', #4913 ) ;
#5170 = CARTESIAN_POINT ( 'NONE',  ( 788.8264449731200330, -357.1800572038739006, 363.6646147819171233 ) ) ;
#5171 = ORIENTED_EDGE ( 'NONE', *, *, #43893, .T. ) ;
#5172 = CARTESIAN_POINT ( 'NONE',  ( 767.7687537140311633, -167.9073299311473022, -372.7932403749916830 ) ) ;
#5173 = CARTESIAN_POINT ( 'NONE',  ( 747.2067596250078623, -75.18005720387485269, 352.2312462859687230 ) ) ;
#5174 = EDGE_LOOP ( 'NONE', ( #28986, #24546, #35045, #12721 ) ) ;
#5175 = CARTESIAN_POINT ( 'NONE',  ( 755.5713283507202505, -173.3618753856927128, -334.6858677611754729 ) ) ;
#5176 = EDGE_LOOP ( 'NONE', ( #31986, #24199, #30497 ) ) ;
#5177 = CARTESIAN_POINT ( 'NONE',  ( 787.5531968255692163, -429.8272453906067199, -316.1348686366205811 ) ) ;
#5178 = CARTESIAN_POINT ( 'NONE',  ( 810.7187646348534145, -258.4527844766016074, 356.7737145352016341 ) ) ;
#5179 = CARTESIAN_POINT ( 'NONE',  ( 758.6633372737375112, -164.5328690171416781, 326.9102291470432533 ) ) ;
#5181 = DIRECTION ( 'NONE',  ( -1.000000000000000000, -0.000000000000000000, -0.000000000000000000 ) ) ;
#5180 = LINE ( 'NONE', #11892, #8545 ) ;
#5182 = EDGE_CURVE ( 'NONE', #36107, #601, #1655, .T. ) ;
#5183 = EDGE_LOOP ( 'NONE', ( #43149, #44103, #43067, #16129, #38130, #1310 ) ) ;
#5184 = CARTESIAN_POINT ( 'NONE',  ( 769.0155153010367712, -442.3726999360611103, -362.7791456095907279 ) ) ;
#5185 = FACE_OUTER_BOUND ( 'NONE', #13079, .T. ) ;
#5186 = CARTESIAN_POINT ( 'NONE',  ( 781.2370466360911223, -212.7363362996982232, -304.9990715423533629 ) ) ;
#5187 = CARTESIAN_POINT ( 'NONE',  ( 746.4236121716829757, -63.82724539060779279, 328.8385539511384650 ) ) ;
#5189 = CARTESIAN_POINT ( 'NONE',  ( 771.1735550268778070, -177.1800572038744690, -316.3353852180827630 ) ) ;
#5188 = CARTESIAN_POINT ( 'NONE',  ( 779.9999999999992042, -462.9681489794448339, -339.9999999999999432 ) ) ;
#5190 = CARTESIAN_POINT ( 'NONE',  ( 754.9735926884551418, -354.3510508353228943, -340.5236548041000333 ) ) ;
#5191 = DIRECTION ( 'NONE',  ( 0.000000000000000000, 0.000000000000000000, 1.000000000000000000 ) ) ;
#5192 = CARTESIAN_POINT ( 'NONE',  ( 795.8262568251477660, -214.3726999360618493, -308.3538107759623585 ) ) ;
#5193 = CARTESIAN_POINT ( 'NONE',  ( 799.9999999999993179, -462.9681489794448339, -309.9999999999998863 ) ) ;
#5195 = EDGE_CURVE ( 'NONE', #5495, #22719, #39348, .T. ) ;
#5194 = FACE_BOUND ( 'NONE', #1912, .T. ) ;
#5196 = CARTESIAN_POINT ( 'NONE',  ( 766.0291762391763086, -58.91815448151690759, -360.7704444035551319 ) ) ;
#5197 = EDGE_CURVE ( 'NONE', #44027, #33524, #21919, .T. ) ;
#5198 = CARTESIAN_POINT ( 'NONE',  ( 759.0159684113467620, -400.9181544815159555, 325.8855110935213020 ) ) ;
#5199 = CARTESIAN_POINT ( 'NONE',  ( 787.5162901302840055, -251.3618753856923718, -305.4481719005793252 ) ) ;
#5200 = DIRECTION ( 'NONE',  ( 0.000000000000000000, 0.000000000000000000, -1.000000000000000000 ) ) ;
#5201 = DIRECTION ( 'NONE',  ( 1.000000000000000000, 0.000000000000000000, 0.000000000000000000 ) ) ;
#5202 = CARTESIAN_POINT ( 'NONE',  ( 804.9363028652555840, -64.27096629478397460, -338.2165204200192079 ) ) ;
#5203 = CARTESIAN_POINT ( 'NONE',  ( 766.4474001241216001, -163.0999726633347677, 307.3154664389482491 ) ) ;
#5204 = CARTESIAN_POINT ( 'NONE',  ( 798.0661480581538854, -122.5328690171417918, -309.5768839229118043 ) ) ;
#5205 = CARTESIAN_POINT ( 'NONE',  ( 792.3570229623688874, -141.1800572038746395, 373.1304606946836202 ) ) ;
#5206 = CARTESIAN_POINT ( 'NONE',  ( 749.2812353651451076, -390.4527844766011526, -323.2262854647983090 ) ) ;
#5207 = LINE ( 'NONE', #11707, #23915 ) ;
#5208 = CARTESIAN_POINT ( 'NONE',  ( 762.1405469898971887, -241.5436935675106156, 357.8594530101015607 ) ) ;
#5209 = CARTESIAN_POINT ( 'NONE',  ( 805.2837595273609850, -26.73633629969882008, 340.5290396650784714 ) ) ;
#5210 = EDGE_CURVE ( 'NONE', #11422, #28329, #14873, .T. ) ;
#5211 = CARTESIAN_POINT ( 'NONE',  ( 756.5762568750052424, -387.1800572038738437, -348.7366044899774238 ) ) ;
#5212 = DIRECTION ( 'NONE',  ( 0.000000000000000000, 0.000000000000000000, 1.000000000000000000 ) ) ;
#5213 = CARTESIAN_POINT ( 'NONE',  ( 752.7379699480933368, -12.00906357242613609, -361.9858362298580232 ) ) ;
#5215 = ADVANCED_FACE ( 'NONE', ( #4470 ), #26380, .T. ) ;
#5214 = FACE_OUTER_BOUND ( 'NONE', #22702, .T. ) ;
#5216 = CARTESIAN_POINT ( 'NONE',  ( 803.2186876482843445, -103.9874144716873161, 350.0220218866286928 ) ) ;
#5217 = ORIENTED_EDGE ( 'NONE', *, *, #39667, .T. ) ;
#5218 = CARTESIAN_POINT ( 'NONE',  ( 769.1273215169530886, -214.7146871989597230, -317.4527132478988847 ) ) ;
#5219 = CARTESIAN_POINT ( 'NONE',  ( 805.1927285166397041, -64.81642084023852135, 341.8018195045277707 ) ) ;
#5220 = CARTESIAN_POINT ( 'NONE',  ( 808.7758568127978833, -220.1692326535051052, -320.0363995740631822 ) ) ;
#5221 = FACE_OUTER_BOUND ( 'NONE', #31032, .T. ) ;
#5222 = CARTESIAN_POINT ( 'NONE',  ( 781.2497674668890113, -348.3510508353228943, 375.3608509340180603 ) ) ;
#5223 = ORIENTED_EDGE ( 'NONE', *, *, #1014, .T. ) ;
#5224 = CARTESIAN_POINT ( 'NONE',  ( 766.5853460496234675, -421.9874144716863498, 372.3518521366060554 ) ) ;
#5225 = CARTESIAN_POINT ( 'NONE',  ( 804.9511171171677688, -29.80559628986937781, -335.8780910478229202 ) ) ;
#5226 = CARTESIAN_POINT ( 'NONE',  ( 785.3687786644884454, -323.3618753856923149, 315.3201227861279676 ) ) ;
#5227 = CARTESIAN_POINT ( 'NONE',  ( 808.0189434323515343, -62.08914811296580183, -319.0252816721025511 ) ) ;
#5228 = CARTESIAN_POINT ( 'NONE',  ( 765.0180583372156207, -72.99823902205667991, -360.0135310231089534 ) ) ;
#5229 = EDGE_LOOP ( 'NONE', ( #15133, #26425 ) ) ;
#5230 = CARTESIAN_POINT ( 'NONE',  ( 780.5236548040995785, 3.263663700301089765, -314.9735926884559944 ) ) ;
#5231 = EDGE_LOOP ( 'NONE', ( #30202, #34802, #39527, #43738 ) ) ;
#5232 = CARTESIAN_POINT ( 'NONE',  ( 773.4516893846965786, -331.6454272087888171, -315.8398074228977066 ) ) ;
#5233 = EDGE_CURVE ( 'NONE', #42700, #9048, #40360, .T. ) ;
#5235 = CARTESIAN_POINT ( 'NONE',  ( 755.5913626894240451, -373.6454272087887034, 346.6156483768012890 ) ) ;
#5234 = CARTESIAN_POINT ( 'NONE',  ( 764.8639956371174549, -104.0891481129656881, 319.7806653035542013 ) ) ;
#5238 = CARTESIAN_POINT ( 'NONE',  ( 807.5423716828161105, -321.0783235625956991, 362.2119215644372048 ) ) ;
#5237 = CARTESIAN_POINT ( 'NONE',  ( 914.9999999999992042, 46.15097736693707020, 350.0000000000000000 ) ) ;
#5236 = CARTESIAN_POINT ( 'NONE',  ( 772.4837098697145166, -431.3618753856918602, 374.5518280994205611 ) ) ;
#5239 = EDGE_CURVE ( 'NONE', #43290, #42970, #27072, .T. ) ;
#5240 = CARTESIAN_POINT ( 'NONE',  ( 781.2497674668890113, -108.3510508353236759, 375.3608509340180603 ) ) ;
#5241 = CARTESIAN_POINT ( 'NONE',  ( 763.0428371773158460, -323.4636090269706301, -358.7617431975195359 ) ) ;
#5242 = CARTESIAN_POINT ( 'NONE',  ( 803.6646147819161570, -329.9073299311467053, -348.8264449731210561 ) ) ;
#5243 = CARTESIAN_POINT ( 'NONE',  ( 804.6798772138708955, -135.7255117493291152, -334.6312213355107019 ) ) ;
#5244 = CARTESIAN_POINT ( 'NONE',  ( 744.7301800767019131, -436.8164208402372992, 337.4774526936615757 ) ) ;
#5246 = DIRECTION ( 'NONE',  ( -0.000000000000000000, -0.000000000000000000, 1.000000000000000000 ) ) ;
#5245 = PLANE ( 'NONE',  #13062 ) ;
#5247 = CARTESIAN_POINT ( 'NONE',  ( 795.8262568251477660, -118.3726999360621619, -308.3538107759623585 ) ) ;
#5248 = LINE ( 'NONE', #40597, #11606 ) ;
#5249 = CARTESIAN_POINT ( 'NONE',  ( 959.5497976682736407, 120.6654763175833693, -2132.806278688367456 ) ) ;
#5250 = EDGE_CURVE ( 'NONE', #20839, #5289, #39638, .T. ) ;
#5251 = CARTESIAN_POINT ( 'NONE',  ( 804.4086373105744769, -313.6454272087888171, 333.3843516231986541 ) ) ;
#5252 = ORIENTED_EDGE ( 'NONE', *, *, #28896, .F. ) ;
#5253 = CARTESIAN_POINT ( 'NONE',  ( 782.4968714119720516, -130.8164208402383224, -305.0891759886411023 ) ) ;
#5254 = CARTESIAN_POINT ( 'NONE',  ( 799.9999999999993179, -512.9681489794448908, 339.9999999999999432 ) ) ;
#5255 = CARTESIAN_POINT ( 'NONE',  ( 776.2046728542105711, -68.19088175424413123, 304.8212110874238761 ) ) ;
#5256 = CARTESIAN_POINT ( 'NONE',  ( 747.2067596250078623, -267.1800572038742985, -352.2312462859687230 ) ) ;
#5257 = CARTESIAN_POINT ( 'NONE',  ( 745.0891759886404770, -436.2709662947827951, -342.4968714119734159 ) ) ;
#5258 = CARTESIAN_POINT ( 'NONE',  ( 801.9419747391806368, -138.4527844766019200, 351.9812246680014027 ) ) ;
#5259 = ORIENTED_EDGE ( 'NONE', *, *, #16521, .F. ) ;
#5260 = CARTESIAN_POINT ( 'NONE',  ( 748.3538107759620743, -328.7146871989592682, -355.8262568251490165 ) ) ;
#5261 = CARTESIAN_POINT ( 'NONE',  ( 813.1304606946830518, -89.90732993114750116, -352.3570229623690580 ) ) ;
#5262 = CARTESIAN_POINT ( 'NONE',  ( 755.3028492785439312, -15.28179084515340058, 335.9200461376539693 ) ) ;
#5263 = CARTESIAN_POINT ( 'NONE',  ( 814.9108240113580450, -352.2709662947830225, -337.5031285880265273 ) ) ;
#5264 = CARTESIAN_POINT ( 'NONE',  ( 799.9999999999993179, 197.3292319334027241, 273.4704985657796783 ) ) ;
#5265 = CARTESIAN_POINT ( 'NONE',  ( 795.9930595647434757, -411.0783235625954717, 320.7433823573372820 ) ) ;
#5266 = VERTEX_POINT ( 'NONE', #2121 ) ;
#5267 = CARTESIAN_POINT ( 'NONE',  ( 798.7617431975189675, -75.62377810805104161, 323.0428371773161871 ) ) ;
#5268 = CARTESIAN_POINT ( 'NONE',  ( 755.3201227861273992, -219.7255117493289447, -345.3687786644892981 ) ) ;
#5269 = CARTESIAN_POINT ( 'NONE',  ( 807.5423716828161105, -129.0783235625963243, -362.2119215644372048 ) ) ;
#5270 = DIRECTION ( 'NONE',  ( 0.000000000000000000, -0.6755902076156505842, -0.7372773368101327440 ) ) ;
#5271 = CARTESIAN_POINT ( 'NONE',  ( 745.1769319972822814, -257.8055962898686744, 346.2694204179732083 ) ) ;
#5272 = CARTESIAN_POINT ( 'NONE',  ( 767.8955696845334842, -72.45278447660213317, 362.1676090361161755 ) ) ;
#5273 = ORIENTED_EDGE ( 'NONE', *, *, #37945, .T. ) ;
#5274 = ORIENTED_EDGE ( 'NONE', *, *, #22162, .T. ) ;
#5275 = CARTESIAN_POINT ( 'NONE',  ( 805.0264073115434940, -222.3510508353233206, -339.4763451958999099 ) ) ;
#5276 = CARTESIAN_POINT ( 'NONE',  ( 762.3223304703356007, -247.5436935675106724, 322.3223304703362828 ) ) ;
#5277 = CARTESIAN_POINT ( 'NONE',  ( 782.4968714119720516, 13.18357915976123174, -305.0891759886411023 ) ) ;
#5278 = CARTESIAN_POINT ( 'NONE',  ( 807.5423716828161105, -57.07832356259658013, -362.2119215644372048 ) ) ;
#5279 = CYLINDRICAL_SURFACE ( 'NONE', #25408, 20.00000000000001776 ) ;
#5280 = EDGE_LOOP ( 'NONE', ( #30765, #27271, #4117, #12240 ) ) ;
#5281 = EDGE_LOOP ( 'NONE', ( #26473, #28522, #9221, #12508 ) ) ;
#5282 = CARTESIAN_POINT ( 'NONE',  ( 814.8207195650702488, -362.1908817542432644, -336.2433038121456548 ) ) ;
#5283 = CARTESIAN_POINT ( 'NONE',  ( 781.7834795799800531, -226.8164208402380098, -315.0636971347436202 ) ) ;
#5284 = CARTESIAN_POINT ( 'NONE',  ( 744.7301800767020268, -340.8164208402376403, 337.4774526936615189 ) ) ;
#5285 = CARTESIAN_POINT ( 'NONE',  ( 749.8865473780648472, -44.53286901714205470, 322.1177392798429082 ) ) ;
#5286 = CARTESIAN_POINT ( 'NONE',  ( 784.1219089521767955, -237.2817908451526421, -315.0488828828318333 ) ) ;
#5287 = CARTESIAN_POINT ( 'NONE',  ( 785.3141322388236176, -213.7255117493289731, -364.4286716492789537 ) ) ;
#5288 = CARTESIAN_POINT ( 'NONE',  ( 762.3223304703356007, -367.5436935675102745, -322.3223304703362828 ) ) ;
#5289 = VERTEX_POINT ( 'NONE', #30288 ) ;
#5290 = CARTESIAN_POINT ( 'NONE',  ( 785.3687786644884454, -203.3618753856925991, 315.3201227861279676 ) ) ;
#5291 = CARTESIAN_POINT ( 'NONE',  ( 781.8018195045266339, -118.2709662947837899, -365.1927285166406705 ) ) ;
#5292 = CARTESIAN_POINT ( 'NONE',  ( 754.9967657858570647, -313.5436935675102745, 365.0032342141425374 ) ) ;
#5293 = CARTESIAN_POINT ( 'NONE',  ( 879.9999999999992042, 99.99999999999984368, -360.0000000000000000 ) ) ;
#5294 = CARTESIAN_POINT ( 'NONE',  ( 939.9999999999994316, -428.4497686941065240, -352.6378164459125628 ) ) ;
#5295 = DIRECTION ( 'NONE',  ( -1.000000000000000000, -0.000000000000000000, -0.000000000000000000 ) ) ;
#5296 = CARTESIAN_POINT ( 'NONE',  ( 759.0159684113467620, -184.9181544815165239, 325.8855110935213020 ) ) ;
#5297 = CARTESIAN_POINT ( 'NONE',  ( 802.1676090361156639, -86.63460265842023489, 327.8955696845344505 ) ) ;
#5298 = VERTEX_POINT ( 'NONE', #12984 ) ;
#5299 = CARTESIAN_POINT ( 'NONE',  ( 814.4686193811664907, -435.2817908451521021, -346.2056067578752732 ) ) ;
#5300 = CARTESIAN_POINT ( 'NONE',  ( 805.0032342141413437, -37.54369356751133324, -314.9967657858572352 ) ) ;
#5301 = CARTESIAN_POINT ( 'NONE',  ( 769.1273215169530886, -262.7146871989594956, 317.4527132478988847 ) ) ;
#5302 = CARTESIAN_POINT ( 'NONE',  ( 754.8072714833581358, -388.8164208402374129, -338.1981804954720587 ) ) ;
#5303 = CARTESIAN_POINT ( 'NONE',  ( 762.3223304703356007, -7.543693567511430942, -322.3223304703362828 ) ) ;
#5304 = CARTESIAN_POINT ( 'NONE',  ( 749.2812353651451076, -438.4527844766009821, 323.2262854647983090 ) ) ;
#5305 = CARTESIAN_POINT ( 'NONE',  ( 779.9999999999992042, -462.9681489794448339, 309.9999999999998863 ) ) ;
#5306 = CARTESIAN_POINT ( 'NONE',  ( 804.4086373105744769, -289.6454272087889308, -333.3843516231986541 ) ) ;
#5307 = CARTESIAN_POINT ( 'NONE',  ( 811.0346526505616112, -182.6346026584199649, -323.0537975583477532 ) ) ;
#5308 = CARTESIAN_POINT ( 'NONE',  ( 746.8695393053150156, -53.90732993114765037, 327.6429770376306010 ) ) ;
#5309 = CARTESIAN_POINT ( 'NONE',  ( 815.2698199232961542, -136.8164208402382371, 342.5225473063383106 ) ) ;
#5310 = LINE ( 'NONE', #22864, #23241 ) ;
#5311 = CARTESIAN_POINT ( 'NONE',  ( 51.16348990802859475, 256.5000000000000568, -199.9999999999945146 ) ) ;
#5312 = LINE ( 'NONE', #5543, #10273 ) ;
#5313 = CARTESIAN_POINT ( 'NONE',  ( 763.0537975583475827, -360.4527844766010958, 371.0346526505627480 ) ) ;
#5314 = CARTESIAN_POINT ( 'NONE',  ( 797.6776695296629214, -331.5436935675104451, -357.6776695296636603 ) ) ;
#5315 = CARTESIAN_POINT ( 'NONE',  ( 765.8855110935204493, 1.830767346494167391, 319.0159684113471599 ) ) ;
#5316 = VECTOR ( 'NONE', #28249, 1000.000000000000000 ) ;
#5317 = CARTESIAN_POINT ( 'NONE',  ( 804.1009440267234822, -95.46360902697132644, -314.0944755984392600 ) ) ;
#5318 = CARTESIAN_POINT ( 'NONE',  ( 766.7756240680305382, -110.5328690171418629, -361.5560724626415663 ) ) ;
#5319 = CARTESIAN_POINT ( 'NONE',  ( 788.7631598425961101, -145.4419599262326699, 305.7194118038759143 ) ) ;
#5320 = CARTESIAN_POINT ( 'NONE',  ( 804.4286716492782716, -449.3618753856918602, 345.3141322388244703 ) ) ;
#5321 = CARTESIAN_POINT ( 'NONE',  ( 778.7502325331095108, -168.3510508353234911, 304.6391490659818828 ) ) ;
#5322 = CARTESIAN_POINT ( 'NONE',  ( 800.2193346964447755, -18.99823902205683979, -355.1360043628815788 ) ) ;
#5323 = CARTESIAN_POINT ( 'NONE',  ( 758.6633372737375112, -116.5328690171418202, -326.9102291470432533 ) ) ;
#5324 = CARTESIAN_POINT ( 'NONE',  ( 774.6858677611749044, -129.7255117493292289, 315.5713283507209894 ) ) ;
#5325 = CARTESIAN_POINT ( 'NONE',  ( 761.2382568024794409, -423.6237781080499190, -356.9571628226838129 ) ) ;
#5327 = CARTESIAN_POINT ( 'NONE',  ( 759.7806653035535192, -270.9982390220561115, 324.8639956371181370 ) ) ;
#5326 = CARTESIAN_POINT ( 'NONE',  ( 794.9819416627830151, -276.9982390220559978, 319.9864689768909898 ) ) ;
#5328 = DIRECTION ( 'NONE',  ( -0.000000000000000000, 1.000000000000000000, -0.000000000000000000 ) ) ;
#5329 = ORIENTED_EDGE ( 'NONE', *, *, #23218, .F. ) ;
#5330 = CARTESIAN_POINT ( 'NONE',  ( 802.1676090361156639, -446.6346026584189985, 327.8955696845344505 ) ) ;
#5331 = CARTESIAN_POINT ( 'NONE',  ( 752.7379699480933368, -276.0090635724253048, -361.9858362298580232 ) ) ;
#5332 = VERTEX_POINT ( 'NONE', #40482 ) ;
#5333 = DIRECTION ( 'NONE',  ( 0.000000000000000000, 0.000000000000000000, 1.000000000000000000 ) ) ;
#5334 = CARTESIAN_POINT ( 'NONE',  ( 814.2001403089898304, -209.3618753856926276, 347.4397851343538264 ) ) ;
#5335 = CARTESIAN_POINT ( 'NONE',  ( 757.0176451133909268, -301.0999726633342561, 349.9200121543848354 ) ) ;
#5336 = CARTESIAN_POINT ( 'NONE',  ( 755.8398074228967971, -403.4419599262317888, 333.4516893846970333 ) ) ;
#5337 = EDGE_LOOP ( 'NONE', ( #40422, #292, #10993, #45248 ) ) ;
#5338 = CARTESIAN_POINT ( 'NONE',  ( 763.8424801807145741, -114.0090635724258163, -320.5453621957614700 ) ) ;
#5339 = AXIS2_PLACEMENT_3D ( 'NONE', #5930, #26716, #13330 ) ;
#5340 = CARTESIAN_POINT ( 'NONE',  ( 803.6646147819162707, -281.9073299311469327, -348.8264449731211130 ) ) ;
#5341 = ORIENTED_EDGE ( 'NONE', *, *, #32907, .T. ) ;
#5342 = CARTESIAN_POINT ( 'NONE',  ( 792.1044303154645831, -420.4527844766009252, -317.8323909638837677 ) ) ;
#5343 = CARTESIAN_POINT ( 'NONE',  ( 800.0135310231082713, -86.08914811296573077, -325.0180583372163028 ) ) ;
#5344 = CARTESIAN_POINT ( 'NONE',  ( 786.6156483768007774, -289.4419599262321299, 315.5913626894246136 ) ) ;
#5345 = DIRECTION ( 'NONE',  ( 0.000000000000000000, -0.6594541114781790059, -0.7517448203044204691 ) ) ;
#5346 = DIRECTION ( 'NONE',  ( 0.000000000000000000, 0.000000000000000000, 1.000000000000000000 ) ) ;
#5347 = CARTESIAN_POINT ( 'NONE',  ( 701.1634899080286232, 256.4999999999999432, -202.7499999999989484 ) ) ;
#5348 = ORIENTED_EDGE ( 'NONE', *, *, #1226, .F. ) ;
#5349 = CARTESIAN_POINT ( 'NONE',  ( 791.0478386215596629, -357.8272453906068904, -306.7653713866226326 ) ) ;
#5350 = AXIS2_PLACEMENT_3D ( 'NONE', #8388, #11398, #25483 ) ;
#5351 = CARTESIAN_POINT ( 'NONE',  ( 746.4236121716829757, -207.8272453906073451, 328.8385539511384650 ) ) ;
#5353 = CARTESIAN_POINT ( 'NONE',  ( 781.7834795799800531, -298.8164208402377540, -315.0636971347436202 ) ) ;
#5352 = PLANE ( 'NONE',  #22396 ) ;
#5354 = CARTESIAN_POINT ( 'NONE',  ( 831.1634899080286232, 229.9999999999998863, -197.2500000000000853 ) ) ;
#5355 = CARTESIAN_POINT ( 'NONE',  ( 769.9779781133707957, -163.0999726633347677, -316.7813123517150871 ) ) ;
#5356 = CARTESIAN_POINT ( 'NONE',  ( 792.2312462859673587, -35.90732993114770011, 307.2067596250082602 ) ) ;
#5357 = CARTESIAN_POINT ( 'NONE',  ( 794.9999999999993179, 239.9999999999998863, -235.0000000000000000 ) ) ;
#5358 = CARTESIAN_POINT ( 'NONE',  ( 815.2698199232962679, -376.8164208402375834, -342.5225473063383674 ) ) ;
#5359 = DIRECTION ( 'NONE',  ( -1.000000000000000000, -0.000000000000000000, 0.000000000000000000 ) ) ;
#5360 = CARTESIAN_POINT ( 'NONE',  ( 765.0180583372156207, -48.99823902205675807, 360.0135310231089534 ) ) ;
#5361 = CARTESIAN_POINT ( 'NONE',  ( 745.5313806188320314, -327.2817908451525000, 333.7943932421247268 ) ) ;
#5362 = CARTESIAN_POINT ( 'NONE',  ( 755.2512626584698410, -247.5436935675106724, 315.2512626584710915 ) ) ;
#5363 = CARTESIAN_POINT ( 'NONE',  ( 748.9653473494363425, -26.63460265842045871, -356.9462024416521331 ) ) ;
#5364 = CARTESIAN_POINT ( 'NONE',  ( 701.1634899080286232, 259.9999999999999432, -199.9999999999990337 ) ) ;
#5365 = LINE ( 'NONE', #29865, #9928 ) ;
#5366 = CARTESIAN_POINT ( 'NONE',  ( 805.1927285166397041, -352.8164208402374129, 341.8018195045277707 ) ) ;
#5367 = CIRCLE ( 'NONE', #26007, 2.749999999999863665 ) ;
#5368 = CARTESIAN_POINT ( 'NONE',  ( 766.0291762391763086, -106.9181544815167371, 360.7704444035551319 ) ) ;
#5369 = CARTESIAN_POINT ( 'NONE',  ( 802.7791456095903868, -4.714687198960358039, -329.0155153010375102 ) ) ;
#5370 = CARTESIAN_POINT ( 'NONE',  ( 755.0636971347428243, -388.2709662947829656, -341.7834795799807353 ) ) ;
#5371 = DIRECTION ( 'NONE',  ( 0.000000000000000000, 0.000000000000000000, 1.000000000000000000 ) ) ;
#5372 = DIRECTION ( 'NONE',  ( -1.000000000000000000, -0.000000000000000000, -0.000000000000000000 ) ) ;
#5373 = CARTESIAN_POINT ( 'NONE',  ( 791.1614460488616487, -131.2601417444144829, 373.5763878283158874 ) ) ;
#5374 = CARTESIAN_POINT ( 'NONE',  ( 774.6312213355099630, -407.3618753856920307, 364.6798772138717482 ) ) ;
#5375 = ORIENTED_EDGE ( 'NONE', *, *, #36816, .T. ) ;
#5376 = CARTESIAN_POINT ( 'NONE',  ( 773.3843516231979720, -325.4419599262320162, -364.4086373105754433 ) ) ;
#5378 = CARTESIAN_POINT ( 'NONE',  ( 792.1044303154646968, -156.4527844766018916, 317.8323909638837677 ) ) ;
#5377 = CARTESIAN_POINT ( 'NONE',  ( 795.1360043628807261, -164.0891481129655176, 360.2193346964456282 ) ) ;
#5379 = CARTESIAN_POINT ( 'NONE',  ( 746.7653713866222915, -329.2601417444138860, -351.0478386215610271 ) ) ;
#5380 = CYLINDRICAL_SURFACE ( 'NONE', #27823, 20.00000000000001776 ) ;
#5381 = ORIENTED_EDGE ( 'NONE', *, *, #14831, .T. ) ;
#5382 = CARTESIAN_POINT ( 'NONE',  ( 771.2633955100217236, -359.9073299311467053, 363.4237431249939618 ) ) ;
#5383 = VERTEX_POINT ( 'NONE', #5347 ) ;
#5384 = CARTESIAN_POINT ( 'NONE',  ( 454.7528517110262101, 239.9999999999999716, -122.7905160835442615 ) ) ;
#5385 = CARTESIAN_POINT ( 'NONE',  ( 782.5225473063381969, -166.2709662947835909, -375.2698199232970637 ) ) ;
#5386 = CARTESIAN_POINT ( 'NONE',  ( 755.2512626584698410, -103.5436935675111272, 315.2512626584710915 ) ) ;
#5387 = VERTEX_POINT ( 'NONE', #40922 ) ;
#5388 = CARTESIAN_POINT ( 'NONE',  ( 765.0180583372156207, -192.9982390220562820, -360.0135310231089534 ) ) ;
#5389 = VERTEX_POINT ( 'NONE', #44381 ) ;
#5390 = CARTESIAN_POINT ( 'NONE',  ( 801.9419747391806368, 5.547215523397618142, -351.9812246680014027 ) ) ;
#5391 = CARTESIAN_POINT ( 'NONE',  ( 745.0891759886404770, -268.2709662947833067, 342.4968714119734159 ) ) ;
#5392 = CARTESIAN_POINT ( 'NONE',  ( 755.0488828828309806, -161.8055962898689870, 344.1219089521771934 ) ) ;
#5394 = DIRECTION ( 'NONE',  ( -1.000000000000000000, -4.625929269271485914E-16, -0.000000000000000000 ) ) ;
#5393 = CARTESIAN_POINT ( 'NONE',  ( 759.9999999999992042, 166.4563064324884465, 360.0000000000000000 ) ) ;
#5395 = VERTEX_POINT ( 'NONE', #37913 ) ;
#5396 = CARTESIAN_POINT ( 'NONE',  ( 755.1538015810308480, -422.1908817542430370, -343.0433043558613804 ) ) ;
#5397 = CARTESIAN_POINT ( 'NONE',  ( -919.9999999999993179, 154.9999999999998863, 350.0000000000000000 ) ) ;
#5398 = AXIS2_PLACEMENT_3D ( 'NONE', #4634, #6787, #18294 ) ;
#5399 = CARTESIAN_POINT ( 'NONE',  ( 745.7194118038753459, -205.6454272087891297, -348.7631598425976449 ) ) ;
#5400 = CARTESIAN_POINT ( 'NONE',  ( 749.5768839229115201, -108.5545181178803915, 358.0661480581553064 ) ) ;
#5402 = CARTESIAN_POINT ( 'NONE',  ( 800.2193346964447755, -186.9982390220563104, -355.1360043628815788 ) ) ;
#5401 = PLANE ( 'NONE',  #1751 ) ;
#5403 = CARTESIAN_POINT ( 'NONE',  ( 772.3691319403857278, -359.2601417444137724, -315.8894580844506663 ) ) ;
#5404 = DIRECTION ( 'NONE',  ( 0.000000000000000000, 0.000000000000000000, 1.000000000000000000 ) ) ;
#5405 = CARTESIAN_POINT ( 'NONE',  ( 813.5763878283155464, -219.8272453906073167, -351.1614460488615350 ) ) ;
#5406 = CARTESIAN_POINT ( 'NONE',  ( 999.9999999999992042, 249.9999999999998863, -359.0000000000000000 ) ) ;
#5407 = CARTESIAN_POINT ( 'NONE',  ( 769.9999999999992042, 240.0000000000000568, -319.9999999999999432 ) ) ;
#5408 = CARTESIAN_POINT ( 'NONE',  ( 801.5560724626406000, -48.55451811788057626, -326.7756240680316182 ) ) ;
#5409 = CARTESIAN_POINT ( 'NONE',  ( 766.0291762391763086, -418.9181544815157849, 360.7704444035551319 ) ) ;
#5410 = EDGE_CURVE ( 'NONE', #26360, #5298, #6267, .T. ) ;
#5411 = CARTESIAN_POINT ( 'NONE',  ( 786.2694204179717872, -357.2817908451523294, 305.1769319972829067 ) ) ;
#5412 = CARTESIAN_POINT ( 'NONE',  ( 777.4774526936600978, -250.2709662947833351, -304.7301800767028226 ) ) ;
#5413 = CARTESIAN_POINT ( 'NONE',  ( 798.5707757039680246, -245.4636090269709143, 356.7845633553585003 ) ) ;
#5414 = DIRECTION ( 'NONE',  ( -1.880165489482579047E-16, -1.000000000000000000, -0.000000000000000000 ) ) ;
#5415 = CARTESIAN_POINT ( 'NONE',  ( 919.9999999999993179, 219.9999999999998863, -360.0000000000000000 ) ) ;
#5416 = CARTESIAN_POINT ( 'NONE',  ( 755.3201227861273992, -51.72551174932946338, -345.3687786644892981 ) ) ;
#5417 = VECTOR ( 'NONE', #19310, 1000.000000000000000 ) ;
#5418 = CARTESIAN_POINT ( 'NONE',  ( 813.5763878283155464, -171.8272453906074304, 351.1614460488615350 ) ) ;
#5419 = CARTESIAN_POINT ( 'NONE',  ( 810.1134526219336749, -128.5328690171417634, -357.8822607201570349 ) ) ;
#5420 = CARTESIAN_POINT ( 'NONE',  ( 746.8695393053150156, -149.9073299311473875, 327.6429770376306010 ) ) ;
#5421 = CARTESIAN_POINT ( 'NONE',  ( 808.3070685750230950, -378.9982390220555999, -361.1904061080339261 ) ) ;
#5422 = DIRECTION ( 'NONE',  ( -1.000000000000000000, -0.000000000000000000, -0.000000000000000000 ) ) ;
#5423 = CARTESIAN_POINT ( 'NONE',  ( 785.3687786644884454, -251.3618753856923149, 315.3201227861279676 ) ) ;
#5424 = CARTESIAN_POINT ( 'NONE',  ( 804.4086373105744769, -25.64542720878973014, 333.3843516231986541 ) ) ;
#5425 = CARTESIAN_POINT ( 'NONE',  ( 795.1360043628807261, -404.0891481129646081, -360.2193346964456282 ) ) ;
#5426 = CARTESIAN_POINT ( 'NONE',  ( -773.4999999999993179, -544.8427095258973623, -350.0000000000000000 ) ) ;
#5427 = CARTESIAN_POINT ( 'NONE',  ( 783.7953271457878373, -8.190881754244330182, -375.1787889125761239 ) ) ;
#5428 = PLANE ( 'NONE',  #396 ) ;
#5429 = CARTESIAN_POINT ( 'NONE',  ( 758.6633372737375112, -92.53286901714190549, 326.9102291470432533 ) ) ;
#5430 = VERTEX_POINT ( 'NONE', #12737 ) ;
#5431 = ADVANCED_FACE ( 'NONE', ( #1883 ), #20126, .F. ) ;
#5432 = CARTESIAN_POINT ( 'NONE',  ( 802.7791456095903868, -220.7146871989596661, -329.0155153010375102 ) ) ;
#5433 = AXIS2_PLACEMENT_3D ( 'NONE', #22081, #32258, #21856 ) ;
#5434 = CARTESIAN_POINT ( 'NONE',  ( 804.4286716492782716, -65.36187538569306810, 345.3141322388244703 ) ) ;
#5435 = CIRCLE ( 'NONE', #19453, 30.00000000000008171 ) ;
#5436 = CARTESIAN_POINT ( 'NONE',  ( 813.2346286133761168, -221.2601417444142271, -328.9521613784389160 ) ) ;
#5437 =( NAMED_UNIT ( * ) PLANE_ANGLE_UNIT ( ) SI_UNIT ( $, .RADIAN. ) );
#5438 = CARTESIAN_POINT ( 'NONE',  ( 805.9055244015594326, -363.6237781080502032, 315.8990559732753240 ) ) ;
#5439 = ORIENTED_EDGE ( 'NONE', *, *, #32681, .F. ) ;
#5440 = CARTESIAN_POINT ( 'NONE',  ( 759.8311093483677041, -430.1692326535043094, 310.9282345327691814 ) ) ;
#5441 = CARTESIAN_POINT ( 'NONE',  ( 771.1735550268778070, -177.1800572038744690, -316.3353852180827630 ) ) ;
#5442 = CARTESIAN_POINT ( 'NONE',  ( 788.7366044899766848, -371.9073299311465917, 316.5762568750059813 ) ) ;
#5443 = EDGE_CURVE ( 'NONE', #24719, #9965, #23359, .T. ) ;
#5444 = CARTESIAN_POINT ( 'NONE',  ( 810.7187646348534145, -90.45278447660209054, -356.7737145352016341 ) ) ;
#5445 = CARTESIAN_POINT ( 'NONE',  ( 795.1360043628808398, -68.08914811296577341, -360.2193346964456282 ) ) ;
#5446 = ORIENTED_EDGE ( 'NONE', *, *, #32624, .F. ) ;
#5447 = CARTESIAN_POINT ( 'NONE',  ( 787.5531968255692163, 2.172754609392001601, -316.1348686366205811 ) ) ;
#5448 = VERTEX_POINT ( 'NONE', #41165 ) ;
#5449 = CARTESIAN_POINT ( 'NONE',  ( 793.0897708529556667, -366.5545181178795815, -361.3366627262616362 ) ) ;
#5450 = AXIS2_PLACEMENT_3D ( 'NONE', #19014, #12077, #36561 ) ;
#5452 = CARTESIAN_POINT ( 'NONE',  ( 783.0745993439762742, -392.1908817542432075, 365.1016975059196739 ) ) ;
#5451 = CARTESIAN_POINT ( 'NONE',  ( 767.8955696845333705, -96.45278447660203369, 362.1676090361162323 ) ) ;
#5455 = CARTESIAN_POINT ( 'NONE',  ( 778.7502325331095108, -336.3510508353228943, 304.6391490659818828 ) ) ;
#5454 = CYLINDRICAL_SURFACE ( 'NONE', #38766, 7.999999999999896083 ) ;
#5453 = CARTESIAN_POINT ( 'NONE',  ( 812.7932403749906598, -423.1800572038737300, 327.7687537140311633 ) ) ;
#5456 = CARTESIAN_POINT ( 'NONE',  ( 747.3154664389472828, -91.98741447168737295, 326.4474001241230781 ) ) ;
#5457 = CARTESIAN_POINT ( 'NONE',  ( 766.9102291470427417, -330.5545181178796952, -318.6633372737382501 ) ) ;
#5458 = CARTESIAN_POINT ( 'NONE',  ( 759.9864689768902508, -338.0891481129649492, -354.9819416627836404 ) ) ;
#5459 = CARTESIAN_POINT ( 'NONE',  ( 795.1360043628807261, -164.0891481129655176, -360.2193346964456282 ) ) ;
#5460 = EDGE_CURVE ( 'NONE', #25515, #38059, #44855, .T. ) ;
#5461 = CARTESIAN_POINT ( 'NONE',  ( 796.7737145352015204, -452.6346026584191691, 370.7187646348536987 ) ) ;
#5463 = CARTESIAN_POINT ( 'NONE',  ( -829.9999999999992042, 290.0000000000001137, -244.9999999999999716 ) ) ;
#5462 = CARTESIAN_POINT ( 'NONE',  ( 939.9999999999992042, 240.0000000000000568, 210.0000000000000000 ) ) ;
#5464 = CARTESIAN_POINT ( 'NONE',  ( 787.6308680596127942, -275.2601417444140566, -364.1105419155492768 ) ) ;
#5465 = ADVANCED_FACE ( 'NONE', ( #41388 ), #25890, .F. ) ;
#5466 = CARTESIAN_POINT ( 'NONE',  ( 744.6391490659812007, -134.7363362996984790, -338.7502325331110455 ) ) ;
#5467 = CARTESIAN_POINT ( 'NONE',  ( 790.0183182880230106, -452.9681489794449476, 362.9048749981275250 ) ) ;
#5468 = CARTESIAN_POINT ( 'NONE',  ( 799.9999999999993179, -462.9681489794448339, 309.9999999999998863 ) ) ;
#5469 = CARTESIAN_POINT ( 'NONE',  ( 763.8424801807145741, -282.0090635724253048, 320.5453621957614700 ) ) ;
#5470 = CARTESIAN_POINT ( 'NONE',  ( 754.8072714833581358, -172.8164208402381234, 338.1981804954720587 ) ) ;
#5471 = ORIENTED_EDGE ( 'NONE', *, *, #42213, .F. ) ;
#5472 = CARTESIAN_POINT ( 'NONE',  ( 757.7880784355613741, -282.0090635724253048, 312.4576283171834916 ) ) ;
#5473 = CARTESIAN_POINT ( 'NONE',  ( 772.5602148656447525, -153.7255117493291721, -305.7998596910095443 ) ) ;
#5474 = DIRECTION ( 'NONE',  ( 0.000000000000000000, 1.110223024625155554E-15, -1.000000000000000000 ) ) ;
#5475 = CARTESIAN_POINT ( 'NONE',  ( 755.8990559732751535, -59.46360902697142592, 365.9055244015606831 ) ) ;
#5476 = CARTESIAN_POINT ( 'NONE',  ( 815.2698199232961542, -280.8164208402378677, -342.5225473063383106 ) ) ;
#5477 = CARTESIAN_POINT ( 'NONE',  ( 747.2067596250078623, -435.1800572038737869, -352.2312462859687230 ) ) ;
#5478 = CARTESIAN_POINT ( 'NONE',  ( 756.3353852180819104, -149.9073299311473875, 331.1735550268788302 ) ) ;
#5479 = CARTESIAN_POINT ( 'NONE',  ( 745.1769319972822814, -353.8055962898683333, -346.2694204179732083 ) ) ;
#5480 = CARTESIAN_POINT ( 'NONE',  ( 792.3570229623688874, -93.18005720387481006, -373.1304606946836202 ) ) ;
#5481 = CIRCLE ( 'NONE', #32035, 10.00000000000006395 ) ;
#5482 = ADVANCED_FACE ( 'NONE', ( #38629 ), #36826, .T. ) ;
#5483 = CARTESIAN_POINT ( 'NONE',  ( 775.8780910478218402, -33.28179084515333130, 364.9511171171680530 ) ) ;
#5484 = CARTESIAN_POINT ( 'NONE',  ( 755.2512626584698410, -367.5436935675102745, -315.2512626584710915 ) ) ;
#5485 = CARTESIAN_POINT ( 'NONE',  ( 939.9999999999993179, -600.0000000000001137, 350.0000000000000000 ) ) ;
#5486 = CARTESIAN_POINT ( 'NONE',  ( 801.3366627262608972, -416.5328690171409107, 353.0897708529566899 ) ) ;
#5487 = ORIENTED_EDGE ( 'NONE', *, *, #18705, .F. ) ;
#5488 = CARTESIAN_POINT ( 'NONE',  ( 775.9200461376533440, -71.80559628986922860, 315.3028492785443291 ) ) ;
#5489 = VECTOR ( 'NONE', #4025, 1000.000000000000000 ) ;
#5490 = EDGE_CURVE ( 'NONE', #41960, #20290, #45724, .T. ) ;
#5491 = CARTESIAN_POINT ( 'NONE',  ( 758.0141637701419768, -111.0783235625964096, -367.2620300519063790 ) ) ;
#5492 = CARTESIAN_POINT ( 'NONE',  ( 311.1634899080286232, 240.0000000000000000, -202.7499999999961915 ) ) ;
#5493 = CARTESIAN_POINT ( 'NONE',  ( 761.9338519418445230, -230.5328690171415076, 370.4231160770881957 ) ) ;
#5494 = CARTESIAN_POINT ( 'NONE',  ( 771.1735550268780344, -81.18005720387482427, 316.3353852180828198 ) ) ;
#5495 = VERTEX_POINT ( 'NONE', #18243 ) ;
#5496 = ORIENTED_EDGE ( 'NONE', *, *, #20182, .F. ) ;
#5497 = CARTESIAN_POINT ( 'NONE',  ( 793.2243759319678702, -2.532869017142183932, -318.4439275373583200 ) ) ;
#5498 = CARTESIAN_POINT ( 'NONE',  ( 804.9363028652555840, -256.2709662947834204, 338.2165204200192079 ) ) ;
#5499 = EDGE_CURVE ( 'NONE', #14856, #20856, #39484, .T. ) ;
#5500 = CARTESIAN_POINT ( 'NONE',  ( 754.0944755984390895, -423.6237781080499190, -364.1009440267246760 ) ) ;
#5501 = CARTESIAN_POINT ( 'NONE',  ( 998.9999999999992042, 74.99999999999984368, -359.0000000000000000 ) ) ;
#5502 = CIRCLE ( 'NONE', #32826, 6.119000000000013095 ) ;
#5503 = EDGE_LOOP ( 'NONE', ( #40837, #6028 ) ) ;
#5504 = EDGE_LOOP ( 'NONE', ( #24647, #14112, #14964, #44075 ) ) ;
#5505 = CARTESIAN_POINT ( 'NONE',  ( 809.0717654672305343, -364.9181544815158986, -360.1688906516309885 ) ) ;
#5506 = VECTOR ( 'NONE', #5595, 1000.000000000000000 ) ;
#5508 = CARTESIAN_POINT ( 'NONE',  ( 800.1688906516307043, -226.1692326535051052, 369.0717654672308186 ) ) ;
#5507 = CARTESIAN_POINT ( 'NONE',  ( 772.4837098697145166, -311.3618753856923149, 374.5518280994205611 ) ) ;
#5509 = CARTESIAN_POINT ( 'NONE',  ( 793.4146539503750546, -49.98741447168749374, 307.6481478633938877 ) ) ;
#5510 = CARTESIAN_POINT ( 'NONE',  ( 761.4292242960306112, -209.4636090269709996, -323.2154366446414429 ) ) ;
#5511 = CARTESIAN_POINT ( 'NONE',  ( 802.1676090361156639, -206.6346026584198512, -327.8955696845344505 ) ) ;
#5512 = CARTESIAN_POINT ( 'NONE',  ( 778.2165204200184689, -406.8164208402375266, -364.9363028652563230 ) ) ;
#5513 = EDGE_LOOP ( 'NONE', ( #20969, #15897, #8765, #32507 ) ) ;
#5514 = CARTESIAN_POINT ( 'NONE',  ( 797.8594530101008786, -205.5436935675108430, 322.1405469898980982 ) ) ;
#5515 = CARTESIAN_POINT ( 'NONE',  ( 797.6776695296629214, -115.5436935675110988, -357.6776695296636603 ) ) ;
#5516 = VERTEX_POINT ( 'NONE', #17773 ) ;
#5517 = CARTESIAN_POINT ( 'NONE',  ( 767.7687537140311633, -311.9073299311468759, 372.7932403749916830 ) ) ;
#5518 = ADVANCED_FACE ( 'NONE', ( #24914, #42024 ), #209, .T. ) ;
#5519 = DIRECTION ( 'NONE',  ( 0.000000000000000000, 0.000000000000000000, 1.000000000000000000 ) ) ;
#5520 = DIRECTION ( 'NONE',  ( 1.000000000000000000, 0.000000000000000000, 0.000000000000000000 ) ) ;
#5521 = CARTESIAN_POINT ( 'NONE',  ( 761.4292242960306112, -185.4636090269710280, 323.2154366446414429 ) ) ;
#5522 = VECTOR ( 'NONE', #4307, 1000.000000000000000 ) ;
#5523 = CARTESIAN_POINT ( 'NONE',  ( 800.2193346964447755, -66.99823902205672255, 355.1360043628815788 ) ) ;
#5524 = ORIENTED_EDGE ( 'NONE', *, *, #32500, .T. ) ;
#5525 = CARTESIAN_POINT ( 'NONE',  ( 811.3240766477731540, -436.3726999360612240, -355.6651683502462902 ) ) ;
#5526 = CARTESIAN_POINT ( 'NONE',  ( 800.9747183278959710, -36.99823902205679360, -311.9810565676471583 ) ) ;
#5527 = CARTESIAN_POINT ( 'NONE',  ( 804.1601925771018387, -247.4419599262323004, 346.5483106153029098 ) ) ;
#5528 = CARTESIAN_POINT ( 'NONE',  ( 781.7834795799800531, -394.8164208402374697, -315.0636971347436202 ) ) ;
#5529 = CARTESIAN_POINT ( 'NONE',  ( 755.0636971347428243, -4.270966294784170003, -341.7834795799807353 ) ) ;
#5530 = CARTESIAN_POINT ( 'NONE',  ( 810.7187646348534145, -426.4527844766010389, 356.7737145352016341 ) ) ;
#5531 = DIRECTION ( 'NONE',  ( 0.000000000000000000, 0.000000000000000000, 1.000000000000000000 ) ) ;
#5532 = CARTESIAN_POINT ( 'NONE',  ( 757.0176451133909268, -277.0999726633344267, -349.9200121543848354 ) ) ;
#5533 = CARTESIAN_POINT ( 'NONE',  ( 763.0537975583475827, -168.4527844766018347, -371.0346526505627480 ) ) ;
#5534 = AXIS2_PLACEMENT_3D ( 'NONE', #41405, #23598, #27312 ) ;
#5535 = CARTESIAN_POINT ( 'NONE',  ( 815.2698199232961542, -88.81642084023842187, 342.5225473063383106 ) ) ;
#5536 = CARTESIAN_POINT ( 'NONE',  ( 751.9810565676468741, -146.0891481129655176, 360.9747183278973921 ) ) ;
#5537 = DIRECTION ( 'NONE',  ( -1.000000000000000000, -0.000000000000000000, 0.000000000000000000 ) ) ;
#5538 = AXIS2_PLACEMENT_3D ( 'NONE', #14758, #21906, #427 ) ;
#5539 = FACE_BOUND ( 'NONE', #4627, .T. ) ;
#5540 = CIRCLE ( 'NONE', #30608, 10.00000000000000888 ) ;
#5541 = EDGE_CURVE ( 'NONE', #6874, #9331, #11602, .T. ) ;
#5542 = ADVANCED_FACE ( 'NONE', ( #10602 ), #36008, .T. ) ;
#5543 = CARTESIAN_POINT ( 'NONE',  ( 265.7583438952258916, 430.0000000000002842, -320.0000000000000000 ) ) ;
#5544 = CARTESIAN_POINT ( 'NONE',  ( 747.2067596250078623, -363.1800572038739006, 352.2312462859687230 ) ) ;
#5545 = CARTESIAN_POINT ( 'NONE',  ( 748.9653473494365699, -2.634602658420536425, 356.9462024416520762 ) ) ;
#5546 = CARTESIAN_POINT ( 'NONE',  ( 756.3353852180819104, -341.9073299311465917, -331.1735550268788302 ) ) ;
#5547 = ADVANCED_FACE ( 'NONE', ( #7377 ), #14774, .F. ) ;
#5548 = CARTESIAN_POINT ( 'NONE',  ( 805.1016975059191054, 17.10349461922139369, 343.0745993439771837 ) ) ;
#5549 = CIRCLE ( 'NONE', #31374, 8.025000000000003908 ) ;
#5550 = CARTESIAN_POINT ( 'NONE',  ( 764.1737431748507561, -106.3726999360621903, -371.6461892240376415 ) ) ;
#5551 = CARTESIAN_POINT ( 'NONE',  ( 786.6156483768007774, -145.4419599262326699, -315.5913626894246136 ) ) ;
#5552 = CARTESIAN_POINT ( 'NONE',  ( 771.2368401574024119, -133.4419599262326699, 374.2805881961240857 ) ) ;
#5553 = CARTESIAN_POINT ( 'NONE',  ( 774.6858677611749044, 14.27448825067031812, 315.5713283507209894 ) ) ;
#5554 = AXIS2_PLACEMENT_3D ( 'NONE', #25266, #25045, #28752 ) ;
#5555 = CARTESIAN_POINT ( 'NONE',  ( 773.7943932421234194, -167.8055962898689586, 305.5313806188329409 ) ) ;
#5556 = CARTESIAN_POINT ( 'NONE',  ( 800.2193346964447755, -42.99823902205675807, -355.1360043628815788 ) ) ;
#5557 = CARTESIAN_POINT ( 'NONE',  ( 761.2382568024794409, -183.6237781080507148, -356.9571628226838129 ) ) ;
#5558 = CARTESIAN_POINT ( 'NONE',  ( 791.9812246680005501, -140.6346026584201070, -361.9419747391813189 ) ) ;
#5559 = CARTESIAN_POINT ( 'NONE',  ( 765.0180583372156207, -144.9982390220564525, 360.0135310231089534 ) ) ;
#5560 = VECTOR ( 'NONE', #5609, 1000.000000000000000 ) ;
#5561 = CARTESIAN_POINT ( 'NONE',  ( 773.7943932421234194, 24.19440371013046231, -305.5313806188329409 ) ) ;
#5562 = CARTESIAN_POINT ( 'NONE',  ( 804.4286716492782716, -281.3618753856923718, 345.3141322388244703 ) ) ;
#5563 = FACE_OUTER_BOUND ( 'NONE', #6612, .T. ) ;
#5564 = ORIENTED_EDGE ( 'NONE', *, *, #13446, .F. ) ;
#5565 = CARTESIAN_POINT ( 'NONE',  ( 770.0799878456142551, 10.01258552831232329, 362.9823548866085616 ) ) ;
#5566 = CARTESIAN_POINT ( 'NONE',  ( 749.5768839229115201, -276.5545181178798657, -358.0661480581553064 ) ) ;
#5567 = ORIENTED_EDGE ( 'NONE', *, *, #13708, .F. ) ;
#5568 = SHAPE_DEFINITION_REPRESENTATION ( #35103, #39835 ) ;
#5569 = CARTESIAN_POINT ( 'NONE',  ( 749.2812353651451076, -222.4527844766016642, 323.2262854647983090 ) ) ;
#5570 = CARTESIAN_POINT ( 'NONE',  ( 784.1219089521767955, -285.2817908451526137, 315.0488828828318333 ) ) ;
#5571 = CARTESIAN_POINT ( 'NONE',  ( 769.1273215169530886, -406.7146871989590409, 317.4527132478988847 ) ) ;
#5572 = ORIENTED_EDGE ( 'NONE', *, *, #33916, .T. ) ;
#5573 = CARTESIAN_POINT ( 'NONE',  ( 773.4516893846965786, -115.6454272087894424, -315.8398074228977066 ) ) ;
#5574 = CARTESIAN_POINT ( 'NONE',  ( 755.0636971347428243, -100.2709662947838609, -341.7834795799807353 ) ) ;
#5575 = CARTESIAN_POINT ( 'NONE',  ( 756.3353852180820240, -269.9073299311469327, -331.1735550268787733 ) ) ;
#5576 = AXIS2_PLACEMENT_3D ( 'NONE', #5136, #22228, #25707 ) ;
#5577 = ORIENTED_EDGE ( 'NONE', *, *, #10584, .T. ) ;
#5578 = CARTESIAN_POINT ( 'NONE',  ( 788.7366044899766848, -419.9073299311465348, -316.5762568750059813 ) ) ;
#5579 = CARTESIAN_POINT ( 'NONE',  ( 797.6776695296629214, -67.54369356751125508, -357.6776695296636603 ) ) ;
#5580 = AXIS2_PLACEMENT_3D ( 'NONE', #364, #36154, #21834 ) ;
#5581 = CARTESIAN_POINT ( 'NONE',  ( 759.2295555964440155, -304.1692326535048210, 353.9708237608231229 ) ) ;
#5582 = FACE_OUTER_BOUND ( 'NONE', #12309, .T. ) ;
#5583 = CARTESIAN_POINT ( 'NONE',  ( -338.8365100919713200, 260.0000000000001137, -199.9999999999917861 ) ) ;
#5584 = CARTESIAN_POINT ( 'NONE',  ( 799.9999999999993179, 205.0000000000000568, 255.0000000000000000 ) ) ;
#5585 = ORIENTED_EDGE ( 'NONE', *, *, #17111, .F. ) ;
#5586 = CARTESIAN_POINT ( 'NONE',  ( 750.9282345327678740, -328.9181544815160692, -319.8311093483690115 ) ) ;
#5587 = CARTESIAN_POINT ( 'NONE',  ( 793.5525998758768083, -199.0999726633346825, 372.6845335610516941 ) ) ;
#5588=STYLED_ITEM('',(#45779),#31868);
#5590 = CARTESIAN_POINT ( 'NONE',  ( 762.3223304703356007, -295.5436935675105588, -322.3223304703362828 ) ) ;
#5589 = CARTESIAN_POINT ( 'NONE',  ( -78.83651009197140525, 256.5000000000000568, -193.8809999999935769 ) ) ;
#5591 = DIRECTION ( 'NONE',  ( -0.000000000000000000, 1.000000000000000000, -0.000000000000000000 ) ) ;
#5592 = CARTESIAN_POINT ( 'NONE',  ( 763.0428371773158460, -203.4636090269709996, -358.7617431975195359 ) ) ;
#5593 = CIRCLE ( 'NONE', #34347, 50.00000000000004263 ) ;
#5594 = CARTESIAN_POINT ( 'NONE',  ( 814.2001403089898304, -41.36187538569314626, 347.4397851343538264 ) ) ;
#5595 = DIRECTION ( 'NONE',  ( 1.000000000000000000, -1.880165489482579047E-16, -0.000000000000000000 ) ) ;
#5596 = CARTESIAN_POINT ( 'NONE',  ( 745.0891759886404770, -388.2709662947829656, -342.4968714119734159 ) ) ;
#5597 = SURFACE_STYLE_FILL_AREA ( #23128 ) ;
#5598 = CARTESIAN_POINT ( 'NONE',  ( 768.0187753319979720, -56.63460265842036279, 318.0580252608186242 ) ) ;
#5599 = CARTESIAN_POINT ( 'NONE',  ( 752.7379699480933368, -324.0090635724251911, 361.9858362298580232 ) ) ;
#5600 = CARTESIAN_POINT ( 'NONE',  ( 748.9653473494363425, -266.6346026584197375, 356.9462024416521331 ) ) ;
#5601 = CARTESIAN_POINT ( 'NONE',  ( 758.8095938919642549, -32.08914811296588709, -311.6929314249763365 ) ) ;
#5602 = CARTESIAN_POINT ( 'NONE',  ( 765.0180583372156207, -240.9982390220561683, -360.0135310231089534 ) ) ;
#5603 = CARTESIAN_POINT ( 'NONE',  ( 759.9999999999992042, -462.9681489794448339, 309.9999999999998863 ) ) ;
#5604 = CARTESIAN_POINT ( 'NONE',  ( 771.2633955100217236, -359.9073299311467053, 363.4237431249939618 ) ) ;
#5605 = CARTESIAN_POINT ( 'NONE',  ( 769.0155153010367712, -106.3726999360621903, 362.7791456095907279 ) ) ;
#5606 = CARTESIAN_POINT ( 'NONE',  ( 758.6633372737375112, -20.53286901714212931, -326.9102291470432533 ) ) ;
#5607 = CARTESIAN_POINT ( 'NONE',  ( 762.1405469898973024, -385.5436935675102745, 357.8594530101016176 ) ) ;
#5608 = AXIS2_PLACEMENT_3D ( 'NONE', #20405, #2860, #45598 ) ;
#5609 = DIRECTION ( 'NONE',  ( -1.000000000000000000, 0.000000000000000000, 0.000000000000000000 ) ) ;
#5610 = DIRECTION ( 'NONE',  ( 0.000000000000000000, 0.000000000000000000, 1.000000000000000000 ) ) ;
#5611 = CARTESIAN_POINT ( 'NONE',  ( 771.1735550268778070, -393.1800572038737300, 316.3353852180827630 ) ) ;
#5612 = VERTEX_POINT ( 'NONE', #39249 ) ;
#5613 = AXIS2_PLACEMENT_3D ( 'NONE', #4302, #31997, #7762 ) ;
#5614 = CARTESIAN_POINT ( 'NONE',  ( 759.2295555964440155, -328.1692326535048210, -353.9708237608231229 ) ) ;
#5616 = CARTESIAN_POINT ( 'NONE',  ( 765.0180583372156207, -144.9982390220564525, 360.0135310231089534 ) ) ;
#5615 = CARTESIAN_POINT ( 'NONE',  ( 778.1981804954714335, -202.2709662947834772, 314.8072714833589885 ) ) ;
#5617 = CARTESIAN_POINT ( 'NONE',  ( 749.8865473780648472, -380.5328690171409676, -322.1177392798429082 ) ) ;
#5618 = LINE ( 'NONE', #2152, #15309 ) ;
#5619 = ORIENTED_EDGE ( 'NONE', *, *, #36478, .F. ) ;
#5620 = CARTESIAN_POINT ( 'NONE',  ( 803.4237431249931660, -351.1800572038740142, 331.2633955100225194 ) ) ;
#5621 = AXIS2_PLACEMENT_3D ( 'NONE', #44533, #33682, #23273 ) ;
#5622 = ORIENTED_EDGE ( 'NONE', *, *, #37385, .F. ) ;
#5623 = VECTOR ( 'NONE', #27450, 1000.000000000000000 ) ;
#5624 = CARTESIAN_POINT ( 'NONE',  ( 745.7998596910086917, -197.3618753856926560, -332.5602148656461168 ) ) ;
#5625 = CARTESIAN_POINT ( 'NONE',  ( 812.7932403749906598, -111.1800572038747532, 327.7687537140311633 ) ) ;
#5626 = ORIENTED_EDGE ( 'NONE', *, *, #14615, .F. ) ;
#5627 = CARTESIAN_POINT ( 'NONE',  ( 804.6798772138710092, -159.7255117493291436, -334.6312213355106451 ) ) ;
#5628 = ORIENTED_EDGE ( 'NONE', *, *, #37315, .T. ) ;
#5629 = CARTESIAN_POINT ( 'NONE',  ( 801.9419747391806368, -330.4527844766013231, -351.9812246680014027 ) ) ;
#5630 = CARTESIAN_POINT ( 'NONE',  ( 790.7339360641449275, -462.9631818684622999, -362.6136660859752965 ) ) ;
#5631 = CARTESIAN_POINT ( 'NONE',  ( 745.4481719005789273, -267.7255117493286320, 347.5162901302853129 ) ) ;
#5632 = CARTESIAN_POINT ( 'NONE',  ( 765.8855110935204493, -190.1692326535052189, 319.0159684113471599 ) ) ;
#5634 = DIRECTION ( 'NONE',  ( -0.000000000000000000, 1.586032892321651891E-15, 1.000000000000000000 ) ) ;
#5633 = DIRECTION ( 'NONE',  ( -0.000000000000000000, 1.000000000000000000, -0.000000000000000000 ) ) ;
#5635 = FACE_BOUND ( 'NONE', #29931, .T. ) ;
#5636 = ORIENTED_EDGE ( 'NONE', *, *, #28615, .F. ) ;
#5637 = CARTESIAN_POINT ( 'NONE',  ( 783.0745993439762742, -440.1908817542430370, -365.1016975059196739 ) ) ;
#5638 = CARTESIAN_POINT ( 'NONE',  ( -949.5497976682736407, 120.6654763175833693, -2132.806278688367456 ) ) ;
#5639 = CARTESIAN_POINT ( 'NONE',  ( 998.9999999999992042, 479.9999999999999432, -360.0000000000000000 ) ) ;
#5640 = EDGE_LOOP ( 'NONE', ( #26576, #41313, #37034, #2113, #25208, #36979, #29286, #32303, #10113, #16109, #43701, #38019, #29087, #6247, #38707 ) ) ;
#5641 = CARTESIAN_POINT ( 'NONE',  ( 754.3581564841646241, -233.4636090269708575, -316.1443688327762516 ) ) ;
#5642 = CARTESIAN_POINT ( 'NONE',  ( 810.4231160770870019, -120.5545181178803205, 321.9338519418446936 ) ) ;
#5643 = CIRCLE ( 'NONE', #9346, 19.99999999999990763 ) ;
#5645 = CARTESIAN_POINT ( 'NONE',  ( 795.1360043628807261, -188.0891481129653187, -360.2193346964456282 ) ) ;
#5644 = CYLINDRICAL_SURFACE ( 'NONE', #32254, 50.00000000000004263 ) ;
#5646 = CARTESIAN_POINT ( 'NONE',  ( 786.6156483768007774, -361.4419599262319593, -315.5913626894246136 ) ) ;
#5647 = CARTESIAN_POINT ( 'NONE',  ( -200.7583438952257211, -1.114432678890474281E-13, -244.9999999999999716 ) ) ;
#5648 = CARTESIAN_POINT ( 'NONE',  ( 804.1009440267234822, -239.4636090269709143, -314.0944755984392600 ) ) ;
#5649 = LINE ( 'NONE', #16275, #37778 ) ;
#5650 = DIRECTION ( 'NONE',  ( -0.000000000000000000, 1.000000000000000000, -0.000000000000000000 ) ) ;
#5651 = CARTESIAN_POINT ( 'NONE',  ( 801.5560724626406000, -72.55451811788049099, -326.7756240680316182 ) ) ;
#5652 = AXIS2_PLACEMENT_3D ( 'NONE', #36616, #30125, #29897 ) ;
#5653 = CARTESIAN_POINT ( 'NONE',  ( 766.0291762391763086, -442.9181544815157849, 360.7704444035551319 ) ) ;
#5654 = CIRCLE ( 'NONE', #490, 6.118999999999985562 ) ;
#5655 = LINE ( 'NONE', #2408, #22653 ) ;
#5656 = CARTESIAN_POINT ( 'NONE',  ( 787.4397851343537695, -285.7255117493286889, -374.2001403089903988 ) ) ;
#5657 = LINE ( 'NONE', #34278, #45285 ) ;
#5658 = CARTESIAN_POINT ( 'NONE',  ( -26.63011601220122060, -494.6608068873671300, -357.6536686473015720 ) ) ;
#5659 = CARTESIAN_POINT ( 'NONE',  ( 792.1044303154645831, -60.45278447660215448, -317.8323909638837677 ) ) ;
#5660 = VECTOR ( 'NONE', #41163, 1000.000000000000000 ) ;
#5661 = CARTESIAN_POINT ( 'NONE',  ( 768.9521613784389729, -201.8272453906073451, 373.2346286133773106 ) ) ;
#5662 = CARTESIAN_POINT ( 'NONE',  ( 756.1443688327750579, -141.6237781080508569, -314.3581564841659315 ) ) ;
#5663 = CARTESIAN_POINT ( 'NONE',  ( 772.4837098697144029, -167.3618753856927412, 374.5518280994205611 ) ) ;
#5664 = CARTESIAN_POINT ( 'NONE',  ( 787.5162901302840055, -419.3618753856918033, -305.4481719005792684 ) ) ;
#5665 = VECTOR ( 'NONE', #15441, 1000.000000000000000 ) ;
#5666 = DIRECTION ( 'NONE',  ( 0.000000000000000000, 0.000000000000000000, 1.000000000000000000 ) ) ;
#5667 = CARTESIAN_POINT ( 'NONE',  ( 803.6646147819161570, -257.9073299311469896, 348.8264449731210561 ) ) ;
#5668 = CARTESIAN_POINT ( 'NONE',  ( 766.0291762391763086, -10.91815448151704793, 360.7704444035551319 ) ) ;
#5669 = CARTESIAN_POINT ( 'NONE',  ( 771.2633955100217236, -407.9073299311465348, -363.4237431249939618 ) ) ;
#5670 = LINE ( 'NONE', #22978, #25449 ) ;
#5671 = CARTESIAN_POINT ( 'NONE',  ( 791.0478386215596629, -45.82724539060783542, -306.7653713866226326 ) ) ;
#5672 = CARTESIAN_POINT ( 'NONE',  ( 1238.921997096861332, 579.9999999999998863, -320.0000000000000000 ) ) ;
#5673 = CARTESIAN_POINT ( 'NONE',  ( 796.7845633553578182, -105.6237781080509421, 358.5707757039688204 ) ) ;
#5674 = ORIENTED_EDGE ( 'NONE', *, *, #11458, .T. ) ;
#5675 = CARTESIAN_POINT ( 'NONE',  ( 754.8983024940795303, -234.8965053807777963, -336.9254006560228163 ) ) ;
#5676 = CARTESIAN_POINT ( 'NONE',  ( 768.0187753319979720, -128.6346026584201354, -318.0580252608186242 ) ) ;
#5677 = CARTESIAN_POINT ( 'NONE',  ( 774.6312213355099630, -71.36187538569302546, 364.6798772138717482 ) ) ;
#5678 = CARTESIAN_POINT ( 'NONE',  ( 786.2056067578752163, -275.8055962898685038, -374.4686193811670023 ) ) ;
#5679 = DIRECTION ( 'NONE',  ( -0.000000000000000000, 1.000000000000000000, -0.000000000000000000 ) ) ;
#5680 = CARTESIAN_POINT ( 'NONE',  ( 745.1769319972822814, -377.8055962898682765, 346.2694204179732083 ) ) ;
#5681 = ORIENTED_EDGE ( 'NONE', *, *, #42431, .F. ) ;
#5682 = AXIS2_PLACEMENT_3D ( 'NONE', #26817, #30075, #9289 ) ;
#5683 = CARTESIAN_POINT ( 'NONE',  ( 782.4968714119720516, 13.18357915976123174, 305.0891759886411023 ) ) ;
#5684 = CARTESIAN_POINT ( 'NONE',  ( 760.5453621957607311, -21.07832356259667250, -323.8424801807151425 ) ) ;
#5685 = CARTESIAN_POINT ( 'NONE',  ( 795.1360043628807261, -188.0891481129653187, -360.2193346964456282 ) ) ;
#5686 = CARTESIAN_POINT ( 'NONE',  ( 771.1735550268778070, -369.1800572038739574, 316.3353852180827630 ) ) ;
#5687 = VECTOR ( 'NONE', #28837, 1000.000000000000000 ) ;
#5688 = CARTESIAN_POINT ( 'NONE',  ( 804.7487373415286811, -67.54369356751125508, -364.7487373415288516 ) ) ;
#5689 = EDGE_CURVE ( 'NONE', #2565, #32511, #24097, .T. ) ;
#5690 = CARTESIAN_POINT ( 'NONE',  ( 754.8072714833583632, -76.81642084023847872, -338.1981804954721156 ) ) ;
#5691 = VERTEX_POINT ( 'NONE', #7601 ) ;
#5692 = CARTESIAN_POINT ( 'NONE',  ( 801.5560724626406000, -24.55451811788064020, -326.7756240680316182 ) ) ;
#5693 = CIRCLE ( 'NONE', #14587, 6.118999999999985562 ) ;
#5694 = ORIENTED_EDGE ( 'NONE', *, *, #44442, .T. ) ;
#5695 = CARTESIAN_POINT ( 'NONE',  ( 805.2837595273609850, -362.7363362996977116, -340.5290396650784714 ) ) ;
#5697 = CARTESIAN_POINT ( 'NONE',  ( 784.1219089521767955, -405.2817908451522158, 315.0488828828318333 ) ) ;
#5696 = CARTESIAN_POINT ( 'NONE',  ( 764.8639956371174549, -80.08914811296574499, 319.7806653035542013 ) ) ;
#5698 = CARTESIAN_POINT ( 'NONE',  ( 756.1348686366196716, -89.26014174441463922, 347.5531968255698416 ) ) ;
#5701 = CARTESIAN_POINT ( 'NONE',  ( 803.8556311672234642, -321.6237781080502600, 365.6418435158340117 ) ) ;
#5700 = DIRECTION ( 'NONE',  ( 0.000000000000000000, 0.000000000000000000, 1.000000000000000000 ) ) ;
#5699 = CARTESIAN_POINT ( 'NONE',  ( 755.2512626584698410, -415.5436935675102177, 315.2512626584710915 ) ) ;
#5702 = CARTESIAN_POINT ( 'NONE',  ( 801.9858362298568863, -123.0783235625963385, 312.7379699480935642 ) ) ;
#5703 = CARTESIAN_POINT ( 'NONE',  ( 784.1219089521767955, -333.2817908451523863, -315.0488828828318333 ) ) ;
#5704 = CARTESIAN_POINT ( 'NONE',  ( 771.1735550268778070, -321.1800572038740142, -316.3353852180827630 ) ) ;
#5705 = CARTESIAN_POINT ( 'NONE',  ( 809.0717654672305343, -124.9181544815167086, -360.1688906516309885 ) ) ;
#5706 = CARTESIAN_POINT ( 'NONE',  ( 776.2046728542105711, 3.809118245755632959, 304.8212110874238761 ) ) ;
#5708 = FACE_OUTER_BOUND ( 'NONE', #31644, .T. ) ;
#5707 = CARTESIAN_POINT ( 'NONE',  ( 779.9999999999992042, 16.45630643248849267, -329.9999999999999432 ) ) ;
#5709 = CARTESIAN_POINT ( 'NONE',  ( 805.6418435158337843, -125.4636090269712412, -363.8556311672236916 ) ) ;
#5710 = LINE ( 'NONE', #23474, #20423 ) ;
#5711 = LINE ( 'NONE', #16106, #19361 ) ;
#5712 = CARTESIAN_POINT ( 'NONE',  ( 761.4292242960306112, -329.4636090269706870, 323.2154366446414429 ) ) ;
#5713 = CARTESIAN_POINT ( 'NONE',  ( 795.1360043628807261, -188.0891481129653187, 360.2193346964456282 ) ) ;
#5714 = EDGE_LOOP ( 'NONE', ( #28871, #23285, #1471, #25341 ) ) ;
#5715 = CARTESIAN_POINT ( 'NONE',  ( 788.6739635108323228, -319.6454272087888739, 373.9316612368139090 ) ) ;
#5716 = CARTESIAN_POINT ( 'NONE',  ( 746.8695393053151292, -173.9073299311472454, -327.6429770376306578 ) ) ;
#5717 = DIRECTION ( 'NONE',  ( 1.000000000000000000, 0.000000000000000000, 0.000000000000000000 ) ) ;
#5718 = CARTESIAN_POINT ( 'NONE',  ( 752.7379699480933368, -108.0090635724258448, 361.9858362298580232 ) ) ;
#5719 = CARTESIAN_POINT ( 'NONE',  ( 800.9747183278959710, -300.9982390220559409, -311.9810565676471583 ) ) ;
#5720 = ADVANCED_FACE ( 'NONE', ( #11291 ), #38795, .F. ) ;
#5721 = CARTESIAN_POINT ( 'NONE',  ( 782.4968714119720516, -442.8164208402372992, -305.0891759886411023 ) ) ;
#5722 = CARTESIAN_POINT ( 'NONE',  ( 801.9419747391806368, -162.4527844766018632, 351.9812246680014027 ) ) ;
#5723 = ORIENTED_EDGE ( 'NONE', *, *, #38818, .F. ) ;
#5724 = CARTESIAN_POINT ( 'NONE',  ( 776.2046728542105711, -404.1908817542431507, 304.8212110874238761 ) ) ;
#5725 = CARTESIAN_POINT ( 'NONE',  ( 803.8556311672234642, -345.6237781080501463, -365.6418435158340117 ) ) ;
#5726 = VECTOR ( 'NONE', #26797, 1000.000000000000000 ) ;
#5727 = CARTESIAN_POINT ( 'NONE',  ( 746.8695393053150156, -77.90732993114757221, -327.6429770376306010 ) ) ;
#5728 = CARTESIAN_POINT ( 'NONE',  ( 780.5236548040995785, -44.73633629969875614, 314.9735926884559944 ) ) ;
#5729 = CARTESIAN_POINT ( 'NONE',  ( 814.2001403089898304, -377.3618753856920875, -347.4397851343538264 ) ) ;
#5730 = CARTESIAN_POINT ( 'NONE',  ( 919.9999999999993179, 219.9999999999998863, -360.0000000000000000 ) ) ;
#5731 = CARTESIAN_POINT ( 'NONE',  ( 804.9511171171677688, -437.8055962898679923, 335.8780910478229202 ) ) ;
#5732 = ORIENTED_EDGE ( 'NONE', *, *, #34778, .F. ) ;
#5733 = CARTESIAN_POINT ( 'NONE',  ( 766.5853460496234675, -133.9874144716872024, -372.3518521366060554 ) ) ;
#5734 = DIRECTION ( 'NONE',  ( 0.000000000000000000, 0.000000000000000000, -1.000000000000000000 ) ) ;
#5735 = CARTESIAN_POINT ( 'NONE',  ( 766.5853460496234675, -277.9874144716867477, 372.3518521366060554 ) ) ;
#5736 = CARTESIAN_POINT ( 'NONE',  ( 764.8639956371174549, -80.08914811296574499, 319.7806653035542581 ) ) ;
#5737 = EDGE_LOOP ( 'NONE', ( #38692, #13151, #1478, #22065, #14540, #26370, #12442, #27865, #33086, #25061, #17683 ) ) ;
#5738 = CARTESIAN_POINT ( 'NONE',  ( 776.9566956441375396, -12.89650538077851216, -364.8461984189686405 ) ) ;
#5739 = CARTESIAN_POINT ( 'NONE',  ( 771.2633955100217236, -263.9073299311469327, 363.4237431249939618 ) ) ;
#5740 = CARTESIAN_POINT ( 'NONE',  ( 761.9338519418445230, -422.5328690171408539, -370.4231160770881957 ) ) ;
#5741 = DIRECTION ( 'NONE',  ( 0.000000000000000000, -0.000000000000000000, 1.000000000000000000 ) ) ;
#5742 = ORIENTED_EDGE ( 'NONE', *, *, #13885, .F. ) ;
#5743 = ORIENTED_EDGE ( 'NONE', *, *, #7837, .F. ) ;
#5744 = CARTESIAN_POINT ( 'NONE',  ( 760.0363995740630116, -370.9181544815159555, -368.7758568127991907 ) ) ;
#5745 = CARTESIAN_POINT ( 'NONE',  ( 788.7366044899766848, -299.9073299311468759, 316.5762568750059813 ) ) ;
#5747 = CARTESIAN_POINT ( 'NONE',  ( 748.3538107759620743, -232.7146871989596377, 355.8262568251490165 ) ) ;
#5746 = CARTESIAN_POINT ( 'NONE',  ( 745.4481719005789273, -315.7255117493286320, 347.5162901302853697 ) ) ;
#5748 = CARTESIAN_POINT ( 'NONE',  ( 757.0176451133909268, -205.0999726633346256, -349.9200121543848354 ) ) ;
#5749 = CARTESIAN_POINT ( 'NONE',  ( 757.8323909638827445, -218.6346026584197944, -352.1044303154654358 ) ) ;
#5750 = CARTESIAN_POINT ( 'NONE',  ( 757.8323909638828582, -410.6346026584191691, -352.1044303154654358 ) ) ;
#5751 = ORIENTED_EDGE ( 'NONE', *, *, #32627, .T. ) ;
#5752 = CARTESIAN_POINT ( 'NONE',  ( 762.1405469898971887, -217.5436935675107293, 357.8594530101015607 ) ) ;
#5753 = CARTESIAN_POINT ( 'NONE',  ( 803.6646147819161570, -113.9073299311474301, -348.8264449731210561 ) ) ;
#5754 = EDGE_LOOP ( 'NONE', ( #16476, #10279, #856, #4471 ) ) ;
#5755 = AXIS2_PLACEMENT_3D ( 'NONE', #9642, #28101, #38286 ) ;
#5756 = CARTESIAN_POINT ( 'NONE',  ( 763.2262854647970016, -368.6346026584193964, 309.2812353651462445 ) ) ;
#5757 = ADVANCED_FACE ( 'NONE', ( #3905, #18000 ), #32070, .F. ) ;
#5758 = CARTESIAN_POINT ( 'NONE',  ( 789.5584187865343893, -452.9681489794450613, -363.1011989789364520 ) ) ;
#5759 = CARTESIAN_POINT ( 'NONE',  ( 793.9408588713487234, 16.45630643248830438, 314.6714885282663090 ) ) ;
#5760 = LINE ( 'NONE', #33929, #19426 ) ;
#5761 = ADVANCED_FACE ( 'NONE', ( #42925 ), #32540, .F. ) ;
#5762 = CARTESIAN_POINT ( 'NONE',  ( 775.8780910478218402, -225.2817908451527273, 364.9511171171680530 ) ) ;
#5763 = CARTESIAN_POINT ( 'NONE',  ( 805.1927285166397041, -88.81642084023842187, 341.8018195045277707 ) ) ;
#5764 = ORIENTED_EDGE ( 'NONE', *, *, #17939, .F. ) ;
#5765 = CARTESIAN_POINT ( 'NONE',  ( 766.4474001241216001, -451.0999726633339151, -307.3154664389482491 ) ) ;
#5766 = CARTESIAN_POINT ( 'NONE',  ( 763.0537975583476964, -48.45278447660221133, -371.0346526505628617 ) ) ;
#5767 = CARTESIAN_POINT ( 'NONE',  ( 801.3366627262608972, -272.5328690171413086, 353.0897708529566899 ) ) ;
#5768 = CARTESIAN_POINT ( 'NONE',  ( 791.9812246680005501, -428.6346026584192259, -361.9419747391813189 ) ) ;
#5769 = CARTESIAN_POINT ( 'NONE',  ( 774.6858677611749044, -9.725511749329603717, -315.5713283507209894 ) ) ;
#5770 = CARTESIAN_POINT ( 'NONE',  ( 801.1904061080336987, -428.0891481129644944, 368.3070685750235498 ) ) ;
#5771 = DIRECTION ( 'NONE',  ( 0.000000000000000000, -1.000000000000000000, 0.000000000000000000 ) ) ;
#5772 = CARTESIAN_POINT ( 'NONE',  ( 793.0897708529556667, -294.5545181178797520, -361.3366627262616362 ) ) ;
#5773 = EDGE_CURVE ( 'NONE', #8959, #28228, #11068, .T. ) ;
#5774 = CARTESIAN_POINT ( 'NONE',  ( 758.8095938919642549, -176.0891481129653755, -311.6929314249763365 ) ) ;
#5775 = EDGE_CURVE ( 'NONE', #31386, #13608, #14989, .T. ) ;
#5776 = CARTESIAN_POINT ( 'NONE',  ( 759.0252816721024374, -96.99823902205660886, 368.0189434323527280 ) ) ;
#5777 = CARTESIAN_POINT ( 'NONE',  ( 796.9462024416508257, -156.4527844766018916, 308.9653473494370246 ) ) ;
#5778 = CARTESIAN_POINT ( 'NONE',  ( 766.8731515446878575, 16.45630643248848912, -318.5849060538806725 ) ) ;
#5779 = CARTESIAN_POINT ( 'NONE',  ( -598.8365100919716042, 258.0940000000001646, -199.9999999999899671 ) ) ;
#5780 = CARTESIAN_POINT ( 'NONE',  ( 746.0683387631852383, -235.4419599262323857, -331.3260364891676204 ) ) ;
#5781 = CARTESIAN_POINT ( 'NONE',  ( 815.3608509340175488, -410.7363362996976548, 341.2497674668889545 ) ) ;
#5782 = LINE ( 'NONE', #16639, #13979 ) ;
#5783 = CARTESIAN_POINT ( 'NONE',  ( 782.5225473063381969, -406.2709662947829088, 375.2698199232970637 ) ) ;
#5784 = CARTESIAN_POINT ( 'NONE',  ( 777.5031285880264704, -22.81642084023865280, 374.9108240113588408 ) ) ;
#5785 = CARTESIAN_POINT ( 'NONE',  ( 764.8639956371174549, -368.0891481129647786, -319.7806653035542013 ) ) ;
#5786 = CARTESIAN_POINT ( 'NONE',  ( 772.3691319403857278, 0.7398582555850804487, 315.8894580844506663 ) ) ;
#5787 = CARTESIAN_POINT ( 'NONE',  ( 754.3581564841646241, -113.4636090269712554, -316.1443688327762516 ) ) ;
#5788 = CARTESIAN_POINT ( 'NONE',  ( 760.5453621957607311, -165.0783235625962391, -323.8424801807151425 ) ) ;
#5789 = EDGE_CURVE ( 'NONE', #17118, #17174, #27051, .T. ) ;
#5790 = CARTESIAN_POINT ( 'NONE',  ( 746.0683387631852383, -163.4419599262325846, 331.3260364891676204 ) ) ;
#5791 = CARTESIAN_POINT ( 'NONE',  ( 764.8639956371174549, 15.91085188703394593, 319.7806653035542581 ) ) ;
#5792 = AXIS2_PLACEMENT_3D ( 'NONE', #17729, #4994, #23815 ) ;
#5793 = EDGE_CURVE ( 'NONE', #8042, #36701, #13080, .T. ) ;
#5794 = CARTESIAN_POINT ( 'NONE',  ( 814.8230680027162407, -173.8055962898689302, 333.7305795820267917 ) ) ;
#5795 = CARTESIAN_POINT ( 'NONE',  ( 805.1927285166397041, -64.81642084023852135, -341.8018195045277707 ) ) ;
#5796 = CARTESIAN_POINT ( 'NONE',  ( 772.3691319403857278, -167.2601417444143976, -315.8894580844506663 ) ) ;
#5797 = CARTESIAN_POINT ( 'NONE',  ( 762.3223304703356007, -175.5436935675108998, 322.3223304703362828 ) ) ;
#5798 = CARTESIAN_POINT ( 'NONE',  ( 744.9990715423526808, 5.648949164675971524, -341.2370466360926002 ) ) ;
#5800 = CARTESIAN_POINT ( 'NONE',  ( 781.8018195045267476, -286.2709662947833067, 365.1927285166407273 ) ) ;
#5799 = CARTESIAN_POINT ( 'NONE',  ( 803.6646147819161570, -281.9073299311468759, 348.8264449731210561 ) ) ;
#5801 = DIRECTION ( 'NONE',  ( 0.000000000000000000, 0.000000000000000000, 1.000000000000000000 ) ) ;
#5802 = ORIENTED_EDGE ( 'NONE', *, *, #33989, .F. ) ;
#5803 = CARTESIAN_POINT ( 'NONE',  ( 755.0488828828309806, -17.80559628986940979, 344.1219089521771934 ) ) ;
#5804 = CARTESIAN_POINT ( 'NONE',  ( 813.5763878283155464, -267.8272453906071746, -351.1614460488615350 ) ) ;
#5805 = ORIENTED_EDGE ( 'NONE', *, *, #19944, .F. ) ;
#5806 = SHAPE_DEFINITION_REPRESENTATION ( #16262, #28884 ) ;
#5807 = CARTESIAN_POINT ( 'NONE',  ( 814.5518280994195948, -231.7255117493288594, 332.4837098697145166 ) ) ;
#5808 = CARTESIAN_POINT ( 'NONE',  ( 757.4527132478984868, -304.3726999360615082, 329.1273215169538844 ) ) ;
#5809 = CARTESIAN_POINT ( 'NONE',  ( 772.3691319403857278, -383.2601417444137155, 315.8894580844506663 ) ) ;
#5810 = VERTEX_POINT ( 'NONE', #1349 ) ;
#5811 = CARTESIAN_POINT ( 'NONE',  ( 779.4763451958990572, -128.7363362996984790, -365.0264073115438919 ) ) ;
#5812 = CARTESIAN_POINT ( 'NONE',  ( 762.3223304703356007, -103.5436935675111272, -322.3223304703362828 ) ) ;
#5813 = CARTESIAN_POINT ( 'NONE',  ( 757.8323909638828582, -314.6346026584195101, -352.1044303154654358 ) ) ;
#5814 = ADVANCED_FACE ( 'NONE', ( #19974 ), #36448, .T. ) ;
#5815 = ORIENTED_EDGE ( 'NONE', *, *, #36821, .F. ) ;
#5816 = CARTESIAN_POINT ( 'NONE',  ( 755.5713283507202505, -437.3618753856919170, -334.6858677611754729 ) ) ;
#5817 = EDGE_CURVE ( 'NONE', #4454, #22673, #29528, .T. ) ;
#5818 = CARTESIAN_POINT ( 'NONE',  ( 793.2243759319678702, -290.5328690171412518, 318.4439275373583200 ) ) ;
#5819 = CARTESIAN_POINT ( 'NONE',  ( 779.9999999999992042, -462.9681489794448339, -339.9999999999999432 ) ) ;
#5820 = LINE ( 'NONE', #16902, #44029 ) ;
#5821 = EDGE_CURVE ( 'NONE', #24190, #26595, #11969, .T. ) ;
#5822 = CARTESIAN_POINT ( 'NONE',  ( 759.9999999999992042, 205.0000000000000568, 319.9999999999999432 ) ) ;
#5823 = VERTEX_POINT ( 'NONE', #22345 ) ;
#5824 = CARTESIAN_POINT ( 'NONE',  ( 791.0478386215596629, -333.8272453906070041, -306.7653713866226326 ) ) ;
#5825 = CARTESIAN_POINT ( 'NONE',  ( 745.7194118038753459, -205.6454272087891297, 348.7631598425976449 ) ) ;
#5826 = AXIS2_PLACEMENT_3D ( 'NONE', #9700, #16399, #44345 ) ;
#5827 = CARTESIAN_POINT ( 'NONE',  ( 785.3141322388236176, -285.7255117493286889, -364.4286716492789537 ) ) ;
#5828 = CARTESIAN_POINT ( 'NONE',  ( 802.5472867521000353, -196.3726999360619061, -350.8726784830461156 ) ) ;
#5829 = EDGE_CURVE ( 'NONE', #8740, #45067, #42592, .T. ) ;
#5830 = CARTESIAN_POINT ( 'NONE',  ( 767.6429770376289525, -57.18005720387489532, 306.8695393053162093 ) ) ;
#5831 = CARTESIAN_POINT ( 'NONE',  ( -773.4999999999993179, -110.5936016518799221, 750.6326042729449455 ) ) ;
#5832 = CARTESIAN_POINT ( 'NONE',  ( 782.5225473063383106, -382.2709662947829088, -375.2698199232970637 ) ) ;
#5833 = CARTESIAN_POINT ( 'NONE',  ( -26.63011601220122060, -494.6608068873671300, -357.6536686473015720 ) ) ;
#5834 = CARTESIAN_POINT ( 'NONE',  ( 778.1981804954714335, -82.27096629478388934, 314.8072714833589885 ) ) ;
#5835 = CARTESIAN_POINT ( 'NONE',  ( 760.0363995740630116, -322.9181544815161260, 368.7758568127991907 ) ) ;
#5836 = CARTESIAN_POINT ( 'NONE',  ( 784.4999999999993179, 22.32581219114657856, 895.6886905569881492 ) ) ;
#5837 = CARTESIAN_POINT ( 'NONE',  ( 767.6429770376289525, -297.1800572038740711, 306.8695393053162093 ) ) ;
#5838 = CARTESIAN_POINT ( 'NONE',  ( 787.5162901302840055, -35.36187538569316047, -305.4481719005792684 ) ) ;
#5839 = CARTESIAN_POINT ( 'NONE',  ( 755.5713283507202505, -245.3618753856925139, -334.6858677611754729 ) ) ;
#5840 = CARTESIAN_POINT ( 'NONE',  ( 787.4999999999992042, -512.9681489794448908, 339.9999999999999432 ) ) ;
#5841 = CARTESIAN_POINT ( 'NONE',  ( 804.6798772138708955, -375.7255117493283478, 334.6312213355107019 ) ) ;
#5842 = CARTESIAN_POINT ( 'NONE',  ( 799.2566176426618085, -120.0090635724258021, 324.0069404352559559 ) ) ;
#5843 = CARTESIAN_POINT ( 'NONE',  ( 790.8726784830453198, -58.71468719896019905, -362.5472867521010585 ) ) ;
#5844 = CARTESIAN_POINT ( 'NONE',  ( 744.9990715423526808, -42.35105083532388193, 341.2370466360926002 ) ) ;
#5845 = CARTESIAN_POINT ( 'NONE',  ( 800.2193346964446619, -354.9982390220557136, 355.1360043628816925 ) ) ;
#5846 = FACE_BOUND ( 'NONE', #7949, .T. ) ;
#5847 = CARTESIAN_POINT ( 'NONE',  ( 791.9812246680005501, -428.6346026584192259, 361.9419747391813189 ) ) ;
#5848 = VERTEX_POINT ( 'NONE', #15229 ) ;
#5849 = CARTESIAN_POINT ( 'NONE',  ( 755.8398074228967971, -379.4419599262318457, -333.4516893846970333 ) ) ;
#5851 = CARTESIAN_POINT ( 'NONE',  ( 759.7806653035535192, -198.9982390220562536, 324.8639956371181370 ) ) ;
#5850 = CARTESIAN_POINT ( 'NONE',  ( 805.1927285166397041, -184.8164208402380950, 341.8018195045277707 ) ) ;
#5852 = CARTESIAN_POINT ( 'NONE',  ( 761.9338519418445230, -350.5328690171411381, -370.4231160770881957 ) ) ;
#5853 = CARTESIAN_POINT ( 'NONE',  ( 998.9999999999992042, -599.0000000000001137, -360.0000000000000000 ) ) ;
#5854 = VERTEX_POINT ( 'NONE', #26662 ) ;
#5855 = CARTESIAN_POINT ( 'NONE',  ( 757.8323909638827445, -386.6346026584191691, 352.1044303154654358 ) ) ;
#5856 = AXIS2_PLACEMENT_3D ( 'NONE', #23408, #8265, #11954 ) ;
#5857 = ORIENTED_EDGE ( 'NONE', *, *, #6651, .T. ) ;
#5858 = CARTESIAN_POINT ( 'NONE',  ( 808.0189434323515343, -206.0891481129653471, -319.0252816721025511 ) ) ;
#5859 = CARTESIAN_POINT ( 'NONE',  ( 805.0032342141413437, -133.5436935675110419, 314.9967657858572352 ) ) ;
#5860 = ORIENTED_EDGE ( 'NONE', *, *, #31546, .F. ) ;
#5861 = CARTESIAN_POINT ( 'NONE',  ( 755.3201227861273992, -195.7255117493290015, -345.3687786644892981 ) ) ;
#5862 = ORIENTED_EDGE ( 'NONE', *, *, #317, .T. ) ;
#5863 = CARTESIAN_POINT ( 'NONE',  ( 771.2633955100217236, -335.9073299311468190, -363.4237431249939618 ) ) ;
#5864 = CARTESIAN_POINT ( 'NONE',  ( 755.5913626894240451, -445.6454272087883055, -346.6156483768012890 ) ) ;
#5865 = CARTESIAN_POINT ( 'NONE',  ( 777.5031285880264704, -238.8164208402379813, 374.9108240113588408 ) ) ;
#5866 = CARTESIAN_POINT ( 'NONE',  ( 769.1273215169530886, -190.7146871989597798, 317.4527132478988847 ) ) ;
#5868 = CARTESIAN_POINT ( 'NONE',  ( 773.4999999999993179, -513.1383975375929367, -349.9999999999999432 ) ) ;
#5867 = LINE ( 'NONE', #18037, #45475 ) ;
#5869 = FACE_OUTER_BOUND ( 'NONE', #22229, .T. ) ;
#5870 = ORIENTED_EDGE ( 'NONE', *, *, #15575, .F. ) ;
#5871 = CARTESIAN_POINT ( 'NONE',  ( 798.5707757039680246, -461.4636090269701754, -356.7845633553585003 ) ) ;
#5872 = CARTESIAN_POINT ( 'NONE',  ( -786.4999999999993179, -513.1383975375929367, -349.9999999999999432 ) ) ;
#5873 = DIRECTION ( 'NONE',  ( -1.000000000000000000, -0.000000000000000000, -0.000000000000000000 ) ) ;
#5874 = ORIENTED_EDGE ( 'NONE', *, *, #28330, .T. ) ;
#5875 = CARTESIAN_POINT ( 'NONE',  ( 760.0363995740630116, -226.9181544815163534, -368.7758568127991907 ) ) ;
#5876 = CARTESIAN_POINT ( 'NONE',  ( 748.6759233522253680, -112.3726999360621761, 324.3348316497537098 ) ) ;
#5878 = CARTESIAN_POINT ( 'NONE',  ( 797.6776695296629214, -187.5436935675108430, -357.6776695296636603 ) ) ;
#5877 = DIRECTION ( 'NONE',  ( 0.000000000000000000, 0.3826834323650836756, 0.9238795325112892920 ) ) ;
#5879 = CARTESIAN_POINT ( 'NONE',  ( 765.8855110935204493, -358.1692326535047641, -319.0159684113471599 ) ) ;
#5880 = CARTESIAN_POINT ( 'NONE',  ( 815.3608509340175488, -218.7363362996982232, -341.2497674668889545 ) ) ;
#5881 = CARTESIAN_POINT ( 'NONE',  ( 794.9999999999993179, 212.6707680665973612, 236.5295014342203785 ) ) ;
#5882 = LINE ( 'NONE', #22959, #33402 ) ;
#5883 = CARTESIAN_POINT ( 'NONE',  ( 780.5236548040995785, -68.73633629969867798, -314.9735926884559944 ) ) ;
#5884 = CARTESIAN_POINT ( 'NONE',  ( 804.4086373105744769, -433.6454272087884760, 333.3843516231986541 ) ) ;
#5885 = FACE_OUTER_BOUND ( 'NONE', #4279, .T. ) ;
#5886 = CARTESIAN_POINT ( 'NONE',  ( 787.6308680596127942, -419.2601417444136587, -364.1105419155492768 ) ) ;
#5887 = CARTESIAN_POINT ( 'NONE',  ( 782.4968714119720516, -274.8164208402378108, -305.0891759886411023 ) ) ;
#5888 = CARTESIAN_POINT ( 'NONE',  ( 311.1634899080286232, 260.0000000000000000, -199.9999999999963336 ) ) ;
#5889 = CARTESIAN_POINT ( 'NONE',  ( 200.7583438952259485, 394.6698570112193920, -274.9999999999999432 ) ) ;
#5890 = CARTESIAN_POINT ( 'NONE',  ( 757.8323909638827445, -50.63460265842036989, -352.1044303154654358 ) ) ;
#5891 = CARTESIAN_POINT ( 'NONE',  ( 757.7880784355613741, -210.0090635724255321, 312.4576283171834916 ) ) ;
#5892 = CARTESIAN_POINT ( 'NONE',  ( 798.0661480581538854, -170.5328690171416781, -309.5768839229118043 ) ) ;
#5893 = CARTESIAN_POINT ( 'NONE',  ( 748.9653473494363425, -170.6346026584199649, 356.9462024416521331 ) ) ;
#5894 = CARTESIAN_POINT ( 'NONE',  ( 792.3570229623688874, -405.1800572038737300, -373.1304606946836202 ) ) ;
#5895 = LINE ( 'NONE', #10051, #26845 ) ;
#5896 = CARTESIAN_POINT ( 'NONE',  ( 755.0636971347428243, -268.2709662947833067, 341.7834795799807353 ) ) ;
#5897 = CARTESIAN_POINT ( 'NONE',  ( 769.0155153010367712, -58.37269993606236085, 362.7791456095907279 ) ) ;
#5898 = CARTESIAN_POINT ( 'NONE',  ( 781.7834795799800531, -442.8164208402372992, -315.0636971347436202 ) ) ;
#5899 = DIRECTION ( 'NONE',  ( -0.000000000000000000, 1.000000000000000000, -0.000000000000000000 ) ) ;
#5900 = CARTESIAN_POINT ( 'NONE',  ( 989.9999999999992042, 469.9999999999999432, -350.0000000000000000 ) ) ;
#5901 = CARTESIAN_POINT ( 'NONE',  ( 796.7845633553578182, -81.62377810805104161, 358.5707757039688204 ) ) ;
#5902 = ORIENTED_EDGE ( 'NONE', *, *, #24394, .F. ) ;
#5903 = CARTESIAN_POINT ( 'NONE',  ( 763.2154366446407039, -237.6237781080505442, -321.4292242960311228 ) ) ;
#5904 = CARTESIAN_POINT ( 'NONE',  ( 778.2165204200184689, -46.81642084023858530, 364.9363028652563230 ) ) ;
#5905 = CARTESIAN_POINT ( 'NONE',  ( 744.9990715423526808, -258.3510508353231785, -341.2370466360926002 ) ) ;
#5906 = CARTESIAN_POINT ( 'NONE',  ( -911.9749999999993406, 219.9999999999998863, 339.9999999999999432 ) ) ;
#5907 = CARTESIAN_POINT ( 'NONE',  ( 791.1614460488616487, -371.2601417444136587, 373.5763878283158874 ) ) ;
#5908 = ORIENTED_EDGE ( 'NONE', *, *, #40798, .F. ) ;
#5909 = CARTESIAN_POINT ( 'NONE',  ( 788.8264449731200330, -189.1800572038744122, -363.6646147819171233 ) ) ;
#5910 = CARTESIAN_POINT ( 'NONE',  ( 756.3353852180819104, -365.9073299311465917, 331.1735550268788302 ) ) ;
#5911 = CARTESIAN_POINT ( 'NONE',  ( 751.9810565676468741, -98.08914811296568814, -360.9747183278973921 ) ) ;
#5912 = CARTESIAN_POINT ( 'NONE',  ( 804.9363028652555840, -64.27096629478397460, -338.2165204200192079 ) ) ;
#5913 = ORIENTED_EDGE ( 'NONE', *, *, #36558, .T. ) ;
#5914 = CARTESIAN_POINT ( 'NONE',  ( 754.7162404726377645, -62.73633629969871350, -339.4709603349214717 ) ) ;
#5915 = EDGE_LOOP ( 'NONE', ( #33444, #35634, #11438, #18589 ) ) ;
#5916 = CARTESIAN_POINT ( 'NONE',  ( 783.0745993439762742, -368.1908817542433212, -365.1016975059196739 ) ) ;
#5918 = CARTESIAN_POINT ( 'NONE',  ( 754.7162404726377645, -398.7363362996976548, 339.4709603349214717 ) ) ;
#5917 = CARTESIAN_POINT ( 'NONE',  ( 797.8594530101008786, -85.54369356751118403, 322.1405469898980982 ) ) ;
#5921 = CARTESIAN_POINT ( 'NONE',  ( 788.7631598425961101, -361.4419599262319593, 305.7194118038759143 ) ) ;
#5920 = LINE ( 'NONE', #40802, #26943 ) ;
#5919 = CARTESIAN_POINT ( 'NONE',  ( 812.7932403749906598, -447.1800572038736732, 327.7687537140311633 ) ) ;
#5922 = CARTESIAN_POINT ( 'NONE',  ( 760.7433823573367135, -324.0090635724251911, -355.9930595647440441 ) ) ;
#5923 = CARTESIAN_POINT ( 'NONE',  ( 774.6312213355099630, -311.3618753856922581, -364.6798772138717482 ) ) ;
#5924 = CARTESIAN_POINT ( 'NONE',  ( 807.2620300519052989, -144.0090635724257027, -318.0141637701419768 ) ) ;
#5925 = CARTESIAN_POINT ( 'NONE',  ( 815.3608509340175488, -2.736336299698892027, 341.2497674668889545 ) ) ;
#5927 = DIRECTION ( 'NONE',  ( 0.000000000000000000, 1.000000000000000000, -0.000000000000000000 ) ) ;
#5926 = PLANE ( 'NONE',  #21172 ) ;
#5928 = CARTESIAN_POINT ( 'NONE',  ( 783.7953271457878373, -104.1908817542440175, -375.1787889125761239 ) ) ;
#5929 = DIRECTION ( 'NONE',  ( 0.000000000000000000, 1.000000000000000000, 0.000000000000000000 ) ) ;
#5930 = CARTESIAN_POINT ( 'NONE',  ( 454.7528517110262101, 199.9999999999999432, -122.7905160835442615 ) ) ;
#5931 = CARTESIAN_POINT ( 'NONE',  ( 769.9779781133707957, -331.0999726633342561, 316.7813123517150871 ) ) ;
#5932 = CARTESIAN_POINT ( 'NONE',  ( 804.4286716492782716, -185.3618753856926844, 345.3141322388244703 ) ) ;
#5933 = ORIENTED_EDGE ( 'NONE', *, *, #35629, .F. ) ;
#5934 = CARTESIAN_POINT ( 'NONE',  ( 744.6391490659812007, -302.7363362996979959, 338.7502325331110455 ) ) ;
#5935 = CARTESIAN_POINT ( 'NONE',  ( 815.2698199232962679, -160.8164208402382371, -342.5225473063383674 ) ) ;
#5936 = CARTESIAN_POINT ( 'NONE',  ( 786.4999999999993179, -512.9681489794448908, -339.9999999999999432 ) ) ;
#5937 = CARTESIAN_POINT ( 'NONE',  ( 745.5313806188320314, -111.2817908451530968, 333.7943932421247268 ) ) ;
#5938 = CARTESIAN_POINT ( 'NONE',  ( 796.9462024416508257, -300.4527844766012663, -308.9653473494370246 ) ) ;
#5939 = PLANE ( 'NONE',  #43939 ) ;
#5940 = CARTESIAN_POINT ( 'NONE',  ( 755.3201227861273992, -147.7255117493291152, 345.3687786644892981 ) ) ;
#5941 = ORIENTED_EDGE ( 'NONE', *, *, #24651, .T. ) ;
#5942 = CARTESIAN_POINT ( 'NONE',  ( 744.6391490659812007, -422.7363362996975980, 338.7502325331110455 ) ) ;
#5943 = CARTESIAN_POINT ( 'NONE',  ( 766.5853460496234675, -349.9874144716865771, -372.3518521366060554 ) ) ;
#5944 = CARTESIAN_POINT ( 'NONE',  ( 796.9462024416508257, -108.4527844766019911, -308.9653473494370246 ) ) ;
#5945 = CARTESIAN_POINT ( 'NONE',  ( 769.9779781133707957, -43.09997266333511590, 316.7813123517150871 ) ) ;
#5946 = CARTESIAN_POINT ( 'NONE',  ( 815.2698199232961542, -376.8164208402375834, -342.5225473063383106 ) ) ;
#5947 = DIRECTION ( 'NONE',  ( 0.000000000000000000, -0.000000000000000000, -1.000000000000000000 ) ) ;
#5948 = CARTESIAN_POINT ( 'NONE',  ( 768.8385539511368734, 24.73985825558500551, 306.4236121716840557 ) ) ;
#5949 = EDGE_LOOP ( 'NONE', ( #26381, #20221, #15527, #13701, #4110, #18562, #28056, #18264 ) ) ;
#5950 = CARTESIAN_POINT ( 'NONE',  ( 790.8726784830453198, -82.71468719896012090, 362.5472867521010585 ) ) ;
#5951 = CARTESIAN_POINT ( 'NONE',  ( 749.8865473780648472, -164.5328690171416781, -322.1177392798429082 ) ) ;
#5952 = LINE ( 'NONE', #12438, #14488 ) ;
#5953 = CARTESIAN_POINT ( 'NONE',  ( 812.6845335610512393, -271.9874144716868045, 353.5525998758768651 ) ) ;
#5954 = CARTESIAN_POINT ( 'NONE',  ( 771.2633955100217236, -71.90732993114760063, 363.4237431249939618 ) ) ;
#5955 = VERTEX_POINT ( 'NONE', #4587 ) ;
#5956 = CARTESIAN_POINT ( 'NONE',  ( 770.0799878456142551, -13.98741447168760033, -362.9823548866085616 ) ) ;
#5957 = CARTESIAN_POINT ( 'NONE',  ( 792.1044303154645831, -252.4527844766015789, 317.8323909638837677 ) ) ;
#5958 = CARTESIAN_POINT ( 'NONE',  ( 803.8556311672234642, -441.6237781080499190, -365.6418435158340117 ) ) ;
#5959 = CARTESIAN_POINT ( 'NONE',  ( 799.9999999999993179, -365.3551492539851893, -18.13243251470705886 ) ) ;
#5960 = ORIENTED_EDGE ( 'NONE', *, *, #32681, .T. ) ;
#5961 = VERTEX_POINT ( 'NONE', #40759 ) ;
#5962 = CARTESIAN_POINT ( 'NONE',  ( 807.2620300519052989, -384.0090635724249637, -318.0141637701419768 ) ) ;
#5963 = ADVANCED_FACE ( 'NONE', ( #27139, #5885 ), #25824, .F. ) ;
#5965 = CARTESIAN_POINT ( 'NONE',  ( 800.1688906516307043, -250.1692326535050199, 369.0717654672308186 ) ) ;
#5964 = CARTESIAN_POINT ( 'NONE',  ( 767.7687537140311633, -311.9073299311468759, 372.7932403749916830 ) ) ;
#5966 = CARTESIAN_POINT ( 'NONE',  ( 763.0428371773158460, -227.4636090269709143, -358.7617431975195359 ) ) ;
#5967 = CARTESIAN_POINT ( 'NONE',  ( 785.3687786644884454, -203.3618753856925991, -315.3201227861279676 ) ) ;
#5968 = CARTESIAN_POINT ( 'NONE',  ( 762.1405469898973024, -409.5436935675101608, -357.8594530101016176 ) ) ;
#5969 = CARTESIAN_POINT ( 'NONE',  ( 781.7834795799800531, -202.8164208402380950, 315.0636971347436202 ) ) ;
#5970 = CARTESIAN_POINT ( 'NONE',  ( 797.8594530101008786, -109.5436935675110988, -322.1405469898980982 ) ) ;
#5971 = ORIENTED_EDGE ( 'NONE', *, *, #43110, .F. ) ;
#5972 = CARTESIAN_POINT ( 'NONE',  ( 787.5162901302840055, -347.3618753856922012, 305.4481719005792684 ) ) ;
#5973 = FACE_OUTER_BOUND ( 'NONE', #17101, .T. ) ;
#5974 = CARTESIAN_POINT ( 'NONE',  ( 778.5401871010416244, 16.45630643248848912, 314.2029270906900251 ) ) ;
#5975 = DIRECTION ( 'NONE',  ( -0.000000000000000000, 1.000000000000000000, -0.000000000000000000 ) ) ;
#5976 = CARTESIAN_POINT ( 'NONE',  ( 773.4516893846965786, -235.6454272087890729, 315.8398074228977066 ) ) ;
#5977 = CARTESIAN_POINT ( 'NONE',  ( 757.8323909638827445, -98.63460265842024910, 352.1044303154654358 ) ) ;
#5978 = VERTEX_POINT ( 'NONE', #9357 ) ;
#5979 = CARTESIAN_POINT ( 'NONE',  ( 776.2046728542105711, -452.1908817542428665, -304.8212110874238761 ) ) ;
#5980 = CARTESIAN_POINT ( 'NONE',  ( 746.8695393053151292, -77.90732993114757221, -327.6429770376306578 ) ) ;
#5981 = CARTESIAN_POINT ( 'NONE',  ( 795.9930595647434757, -267.0783235625958696, 320.7433823573372820 ) ) ;
#5982 = CARTESIAN_POINT ( 'NONE',  ( 778.1981804954714335, -442.2709662947826814, -314.8072714833589885 ) ) ;
#5983 = CARTESIAN_POINT ( 'NONE',  ( 788.7366044899766848, -35.90732993114770011, -316.5762568750059813 ) ) ;
#5984 = CARTESIAN_POINT ( 'NONE',  ( 746.4236121716829757, -15.82724539060794200, 328.8385539511384650 ) ) ;
#5985 = CARTESIAN_POINT ( 'NONE',  ( 768.0187753319979720, 15.36539734157940629, -318.0580252608186242 ) ) ;
#5986 = CARTESIAN_POINT ( 'NONE',  ( 784.1219089521767955, -285.2817908451526137, -315.0488828828318333 ) ) ;
#5987 = CARTESIAN_POINT ( 'NONE',  ( 811.0346526505616112, -206.6346026584198512, -323.0537975583477532 ) ) ;
#5988 = CARTESIAN_POINT ( 'NONE',  ( 763.0537975583475827, -72.45278447660213317, 371.0346526505627480 ) ) ;
#5989 = EDGE_CURVE ( 'NONE', #30700, #15113, #5655, .T. ) ;
#5990 = CARTESIAN_POINT ( 'NONE',  ( 812.7932403749906598, -159.1800572038746111, 327.7687537140311633 ) ) ;
#5991 = DIRECTION ( 'NONE',  ( -0.000000000000000000, 1.000000000000000000, -1.586032892321652088E-15 ) ) ;
#5992 = CARTESIAN_POINT ( 'NONE',  ( 813.2346286133761168, -245.2601417444141987, -328.9521613784389160 ) ) ;
#5993 = CARTESIAN_POINT ( 'NONE',  ( 804.1009440267234822, -407.4636090269703459, 314.0944755984392600 ) ) ;
#5994 = CARTESIAN_POINT ( 'NONE',  ( 787.5162901302840055, -299.3618753856922581, -305.4481719005792684 ) ) ;
#5995 = CARTESIAN_POINT ( 'NONE',  ( 779.9999999999992042, -462.9681489794448339, 339.9999999999999432 ) ) ;
#5996 = CARTESIAN_POINT ( 'NONE',  ( 751.9810565676468741, -386.0891481129647786, 360.9747183278973921 ) ) ;
#5997 = CARTESIAN_POINT ( 'NONE',  ( 777.4774526936600978, -10.27096629478415046, 304.7301800767028226 ) ) ;
#5998 = CARTESIAN_POINT ( 'NONE',  ( 771.2633955100217236, -359.9073299311467053, -363.4237431249939618 ) ) ;
#5999 = CARTESIAN_POINT ( 'NONE',  ( 780.5290396650775619, -12.35105083532396897, 365.2837595273619513 ) ) ;
#6000 = CARTESIAN_POINT ( 'NONE',  ( 754.0944755984390895, -39.62377810805116951, -364.1009440267246760 ) ) ;
#6001 = CARTESIAN_POINT ( 'NONE',  ( 800.7704444035546203, -172.1692326535052757, -326.0291762391768771 ) ) ;
#6002 = CARTESIAN_POINT ( 'NONE',  ( 778.7502325331095108, -168.3510508353234911, 304.6391490659818828 ) ) ;
#6003 = CARTESIAN_POINT ( 'NONE',  ( 791.7608162188021197, 205.0000000000000568, -350.0000000000000000 ) ) ;
#6004 = CARTESIAN_POINT ( 'NONE',  ( 803.8556311672234642, -177.6237781080507148, 365.6418435158340117 ) ) ;
#6005 = ORIENTED_EDGE ( 'NONE', *, *, #9679, .T. ) ;
#6006 = CARTESIAN_POINT ( 'NONE',  ( 803.4237431249931660, -63.18005720387488822, -331.2633955100225194 ) ) ;
#6007 = CARTESIAN_POINT ( 'NONE',  ( 758.6633372737375112, -164.5328690171416781, -326.9102291470432533 ) ) ;
#6008 = CARTESIAN_POINT ( 'NONE',  ( 800.0135310231082713, -158.0891481129655176, 325.0180583372163028 ) ) ;
#6009 = EDGE_CURVE ( 'NONE', #17287, #23251, #2753, .T. ) ;
#6010 = CARTESIAN_POINT ( 'NONE',  ( 771.2368401574024119, -13.44195992623305713, -374.2805881961240857 ) ) ;
#6012 = CARTESIAN_POINT ( 'NONE',  ( 762.3223304703356007, -295.5436935675105588, 322.3223304703362828 ) ) ;
#6011 = CARTESIAN_POINT ( 'NONE',  ( 804.4286716492782716, -281.3618753856923718, 345.3141322388244703 ) ) ;
#6013 = AXIS2_PLACEMENT_3D ( 'NONE', #18296, #15281, #3957 ) ;
#6014 = LINE ( 'NONE', #16415, #10919 ) ;
#6015 = ORIENTED_EDGE ( 'NONE', *, *, #39078, .F. ) ;
#6016 = CARTESIAN_POINT ( 'NONE',  ( 754.8983024940795303, -18.89650538077849617, 336.9254006560228163 ) ) ;
#6017 = CARTESIAN_POINT ( 'NONE',  ( 786.2694204179717872, -285.2817908451526137, -305.1769319972829067 ) ) ;
#6018 = ORIENTED_EDGE ( 'NONE', *, *, #23778, .F. ) ;
#6019 = CARTESIAN_POINT ( 'NONE',  ( 0.000000000000000000, 0.000000000000000000, 0.000000000000000000 ) ) ;
#6020 = EDGE_CURVE ( 'NONE', #14400, #22607, #32769, .T. ) ;
#6021 = CARTESIAN_POINT ( 'NONE',  ( 767.7687537140311633, -215.9073299311471317, 372.7932403749916830 ) ) ;
#6022 = CARTESIAN_POINT ( 'NONE',  ( 798.5707757039680246, -341.4636090269705733, 356.7845633553585003 ) ) ;
#6023 = CARTESIAN_POINT ( 'NONE',  ( 799.4546378042377910, -417.0783235625954148, 356.1575198192848006 ) ) ;
#6024 = ORIENTED_EDGE ( 'NONE', *, *, #409, .T. ) ;
#6025 = CARTESIAN_POINT ( 'NONE',  ( 755.5913626894240451, -109.6454272087894566, -346.6156483768012890 ) ) ;
#6026 = CARTESIAN_POINT ( 'NONE',  ( 778.1981804954714335, -106.2709662947838467, -314.8072714833589885 ) ) ;
#6027 = CARTESIAN_POINT ( 'NONE',  ( 785.3141322388236176, -309.7255117493287457, -364.4286716492789537 ) ) ;
#6028 = ORIENTED_EDGE ( 'NONE', *, *, #5250, .F. ) ;
#6029 = CARTESIAN_POINT ( 'NONE',  ( 778.1981804954714335, -418.2709662947827383, -314.8072714833589885 ) ) ;
#6030 = CARTESIAN_POINT ( 'NONE',  ( 784.0799538623451781, -299.8055962898685038, 364.6971507214555572 ) ) ;
#6031 = CARTESIAN_POINT ( 'NONE',  ( 793.4322487044281615, -453.3695810002254234, 372.3199466871218419 ) ) ;
#6032 = CARTESIAN_POINT ( 'NONE',  ( 784.4999999999993179, -365.3551492539851893, -28.13243251470704109 ) ) ;
#6033 = CARTESIAN_POINT ( 'NONE',  ( 793.0897708529556667, -126.5545181178803205, 361.3366627262616362 ) ) ;
#6034 = CARTESIAN_POINT ( 'NONE',  ( 764.8639956371174549, 15.91085188703394238, 319.7806653035542013 ) ) ;
#6035 = ORIENTED_EDGE ( 'NONE', *, *, #39430, .F. ) ;
#6036 = CARTESIAN_POINT ( 'NONE',  ( 745.5313806188320314, -327.2817908451525000, -333.7943932421247268 ) ) ;
#6037 = EDGE_CURVE ( 'NONE', #42633, #5448, #25612, .T. ) ;
#6038 = CARTESIAN_POINT ( 'NONE',  ( 795.8262568251477660, -214.3726999360618493, 308.3538107759623585 ) ) ;
#6039 = CARTESIAN_POINT ( 'NONE',  ( 778.1981804954714335, -322.2709662947830225, -314.8072714833589885 ) ) ;
#6040 = EDGE_CURVE ( 'NONE', #40029, #29782, #8281, .T. ) ;
#6041 = CARTESIAN_POINT ( 'NONE',  ( 802.5472867521000353, -172.3726999360619914, -350.8726784830461156 ) ) ;
#6042 =( REPRESENTATION_RELATIONSHIP ('NONE','NONE', #39835, #2289 ) REPRESENTATION_RELATIONSHIP_WITH_TRANSFORMATION ( #4344 )SHAPE_REPRESENTATION_RELATIONSHIP( ) );
#6043 = EDGE_CURVE ( 'NONE', #25919, #41246, #11529, .T. ) ;
#6044 = CARTESIAN_POINT ( 'NONE',  ( 796.7737145352015204, -44.63460265842040542, 370.7187646348536987 ) ) ;
#6045 = CARTESIAN_POINT ( 'NONE',  ( 791.3800697268461590, -452.9681489794449476, 362.3092612109132915 ) ) ;
#6046 = CARTESIAN_POINT ( 'NONE',  ( 767.6429770376291799, -393.1800572038737869, -306.8695393053162093 ) ) ;
#6047 = CARTESIAN_POINT ( 'NONE',  ( 794.9999999999993179, 205.0000000000000568, -255.0000000000000000 ) ) ;
#6048 = CARTESIAN_POINT ( 'NONE',  ( 810.4231160770870019, -312.5545181178797520, 321.9338519418446936 ) ) ;
#6049 = CARTESIAN_POINT ( 'NONE',  ( 759.2380499001254748, 21.41625977839825978, 318.3449445151863415 ) ) ;
#6050 = CARTESIAN_POINT ( 'NONE',  ( 777.4774526936600978, -298.2709662947830793, 304.7301800767027657 ) ) ;
#6051 = CARTESIAN_POINT ( 'NONE',  ( 804.7487373415286811, -19.54369356751139364, -364.7487373415288516 ) ) ;
#6052 = CARTESIAN_POINT ( 'NONE',  ( 767.8955696845333705, -264.4527844766016074, -362.1676090361162323 ) ) ;
#6053 = DIRECTION ( 'NONE',  ( 0.000000000000000000, 0.000000000000000000, 1.000000000000000000 ) ) ;
#6054 = CARTESIAN_POINT ( 'NONE',  ( 768.0187753319979720, -392.6346026584193396, 318.0580252608186242 ) ) ;
#6055 = CARTESIAN_POINT ( 'NONE',  ( 787.5531968255692163, -141.8272453906075157, 316.1348686366205811 ) ) ;
#6056 = CARTESIAN_POINT ( 'NONE',  ( 756.1348686366196716, -65.26014174441471027, -347.5531968255698416 ) ) ;
#6057 = CARTESIAN_POINT ( 'NONE',  ( 764.3348316497523456, -70.71468719896014932, 308.6759233522265617 ) ) ;
#6058 = CARTESIAN_POINT ( 'NONE',  ( 788.8264449731201466, -357.1800572038739574, 363.6646147819170665 ) ) ;
#6059 = LINE ( 'NONE', #13240, #1859 ) ;
#6060 = EDGE_CURVE ( 'NONE', #22319, #19543, #16279, .T. ) ;
#6061 = PRESENTATION_STYLE_ASSIGNMENT (( #34479 ) ) ;
#6062 = CARTESIAN_POINT ( 'NONE',  ( 804.4286716492782716, -425.3618753856919170, 345.3141322388244703 ) ) ;
#6063 = ORIENTED_EDGE ( 'NONE', *, *, #44462, .F. ) ;
#6064 = CARTESIAN_POINT ( 'NONE',  ( 781.8018195045266339, -46.27096629478404566, -365.1927285166406705 ) ) ;
#6065 = ADVANCED_FACE ( 'NONE', ( #23425 ), #30358, .F. ) ;
#6066 = CARTESIAN_POINT ( 'NONE',  ( 756.1348686366196716, -377.2601417444137724, -347.5531968255698416 ) ) ;
#6068 = CARTESIAN_POINT ( 'NONE',  ( 794.9819416627830151, -204.9982390220562820, 319.9864689768909898 ) ) ;
#6067 = CARTESIAN_POINT ( 'NONE',  ( 794.9819416627830151, -180.9982390220563389, 319.9864689768909898 ) ) ;
#6069 = VECTOR ( 'NONE', #20486, 1000.000000000000000 ) ;
#6070 = CARTESIAN_POINT ( 'NONE',  ( 756.1443688327750579, -357.6237781080501463, -314.3581564841659315 ) ) ;
#6071 = DIRECTION ( 'NONE',  ( 0.000000000000000000, 0.000000000000000000, -1.000000000000000000 ) ) ;
#6072 = ORIENTED_EDGE ( 'NONE', *, *, #4995, .T. ) ;
#6073 = CARTESIAN_POINT ( 'NONE',  ( 803.6646147819161570, -401.9073299311463643, 348.8264449731210561 ) ) ;
#6074 = VERTEX_POINT ( 'NONE', #6106 ) ;
#6075 = DIRECTION ( 'NONE',  ( 1.000000000000000000, 0.000000000000000000, 0.000000000000000000 ) ) ;
#6076 = EDGE_CURVE ( 'NONE', #35766, #21705, #6448, .T. ) ;
#6077 = CARTESIAN_POINT ( 'NONE',  ( 813.1304606946830518, -209.9073299311470748, -352.3570229623690580 ) ) ;
#6078 = CARTESIAN_POINT ( 'NONE',  ( 754.9967657858570647, -121.5436935675110561, 365.0032342141425943 ) ) ;
#6079 = ORIENTED_EDGE ( 'NONE', *, *, #38013, .T. ) ;
#6080 = VECTOR ( 'NONE', #21557, 1000.000000000000000 ) ;
#6081 = CARTESIAN_POINT ( 'NONE',  ( 774.6858677611749044, -225.7255117493289163, -315.5713283507209894 ) ) ;
#6082 = ORIENTED_EDGE ( 'NONE', *, *, #8079, .F. ) ;
#6083 = CARTESIAN_POINT ( 'NONE',  ( 792.1044303154645831, -324.4527844766013231, -317.8323909638837677 ) ) ;
#6084 = CARTESIAN_POINT ( 'NONE',  ( 763.8424801807145741, -450.0090635724248500, -320.5453621957614700 ) ) ;
#6085 = CARTESIAN_POINT ( 'NONE',  ( 763.0537975583475827, -240.4527844766015221, 371.0346526505627480 ) ) ;
#6086 = CARTESIAN_POINT ( 'NONE',  ( 802.7791456095903868, -196.7146871989598083, 329.0155153010375102 ) ) ;
#6088 = CARTESIAN_POINT ( 'NONE',  ( 779.9999999999992042, -462.9681489794448339, 339.9999999999999432 ) ) ;
#6087 = FACE_OUTER_BOUND ( 'NONE', #15314, .T. ) ;
#6089 = DIRECTION ( 'NONE',  ( -0.000000000000000000, 1.000000000000000000, -0.000000000000000000 ) ) ;
#6090 = ORIENTED_EDGE ( 'NONE', *, *, #23320, .F. ) ;
#6091 = CARTESIAN_POINT ( 'NONE',  ( 802.1676090361156639, 9.365397341579420498, -327.8955696845344505 ) ) ;
#6092 = CARTESIAN_POINT ( 'NONE',  ( 441.1634899080286232, 259.9999999999999432, -197.2499999999973852 ) ) ;
#6093 = ORIENTED_EDGE ( 'NONE', *, *, #29552, .F. ) ;
#6094 = CARTESIAN_POINT ( 'NONE',  ( 793.5525998758768083, -247.0999726633344835, -372.6845335610516941 ) ) ;
#6095 = CARTESIAN_POINT ( 'NONE',  ( 776.2046728542105711, -92.19088175424406018, 304.8212110874238761 ) ) ;
#6097 = CARTESIAN_POINT ( 'NONE',  ( 778.1981804954714335, -226.2709662947834204, -314.8072714833589885 ) ) ;
#6096 = CARTESIAN_POINT ( 'NONE',  ( 831.1634899080286232, 259.9999999999998863, -199.9999999999999432 ) ) ;
#6098 = CARTESIAN_POINT ( 'NONE',  ( 799.4546378042377910, -345.0783235625956991, -356.1575198192848006 ) ) ;
#6099 = CARTESIAN_POINT ( 'NONE',  ( 755.8990559732751535, -251.4636090269709143, -365.9055244015606831 ) ) ;
#6100 = DIRECTION ( 'NONE',  ( 0.000000000000000000, -0.000000000000000000, -1.000000000000000000 ) ) ;
#6101 = CARTESIAN_POINT ( 'NONE',  ( -786.4999999999993179, -295.7697417039441916, 122.5118383533586837 ) ) ;
#6102 = CARTESIAN_POINT ( 'NONE',  ( 773.4516893846965786, -67.64542720878958448, -315.8398074228977066 ) ) ;
#6103 = CARTESIAN_POINT ( 'NONE',  ( 754.7162404726377645, -446.7363362996975980, 339.4709603349214717 ) ) ;
#6104 = CARTESIAN_POINT ( 'NONE',  ( 813.5763878283155464, -363.8272453906068336, 351.1614460488615350 ) ) ;
#6105 = VECTOR ( 'NONE', #5650, 1000.000000000000000 ) ;
#6106 = CARTESIAN_POINT ( 'NONE',  ( 939.9999999999992042, 56.60618624968560653, -350.0000000000000000 ) ) ;
#6107 = CARTESIAN_POINT ( 'NONE',  ( 767.7687537140311633, -263.9073299311469327, -372.7932403749916830 ) ) ;
#6108 = CYLINDRICAL_SURFACE ( 'NONE', #26110, 12.00000000000001066 ) ;
#6109 = LINE ( 'NONE', #3343, #30527 ) ;
#6110 = CARTESIAN_POINT ( 'NONE',  ( 774.6858677611749044, -57.72551174932945628, -315.5713283507209894 ) ) ;
#6111 = CARTESIAN_POINT ( 'NONE',  ( 814.2805881961230625, -217.6454272087891582, 331.2368401574024119 ) ) ;
#6112 = CARTESIAN_POINT ( 'NONE',  ( 778.7502325331095108, -168.3510508353234911, -304.6391490659818828 ) ) ;
#6113 = CARTESIAN_POINT ( 'NONE',  ( 758.8095938919642549, -176.0891481129653755, 311.6929314249763365 ) ) ;
#6114 = CARTESIAN_POINT ( 'NONE',  ( 808.3070685750230950, -402.9982390220555430, -361.1904061080339261 ) ) ;
#6115 = DIRECTION ( 'NONE',  ( 0.000000000000000000, 0.000000000000000000, 1.000000000000000000 ) ) ;
#6116 = CARTESIAN_POINT ( 'NONE',  ( 781.8018195045266339, -286.2709662947833635, 365.1927285166406705 ) ) ;
#6117 = CARTESIAN_POINT ( 'NONE',  ( 787.5531968255692163, -69.82724539060775726, 316.1348686366205811 ) ) ;
#6118 = CARTESIAN_POINT ( 'NONE',  ( 756.5762568750052424, -435.1800572038737869, -348.7366044899774238 ) ) ;
#6119 = DIRECTION ( 'NONE',  ( -1.000000000000000000, 0.000000000000000000, 0.000000000000000000 ) ) ;
#6120 = EDGE_CURVE ( 'NONE', #28948, #42674, #8072, .T. ) ;
#6121 = PLANE ( 'NONE',  #1115 ) ;
#6123 = CARTESIAN_POINT ( 'NONE',  ( 755.5713283507202505, -317.3618753856922581, 334.6858677611754729 ) ) ;
#6122 = CARTESIAN_POINT ( 'NONE',  ( 802.7791456095903868, -100.7146871989600356, 329.0155153010375102 ) ) ;
#6124 = ORIENTED_EDGE ( 'NONE', *, *, #26419, .T. ) ;
#6125 = CARTESIAN_POINT ( 'NONE',  ( 795.9930595647434757, -267.0783235625958696, -320.7433823573372820 ) ) ;
#6126 = CARTESIAN_POINT ( 'NONE',  ( 797.6776695296629214, -43.54369356751131903, 357.6776695296636603 ) ) ;
#6127 = CARTESIAN_POINT ( 'NONE',  ( 748.3538107759620743, -256.7146871989595525, -355.8262568251490165 ) ) ;
#6128 = CARTESIAN_POINT ( 'NONE',  ( 914.9999999999992042, 74.99999999999984368, -360.0000000000000000 ) ) ;
#6129 = CARTESIAN_POINT ( 'NONE',  ( 756.1443688327750579, -381.6237781080500326, 314.3581564841659315 ) ) ;
#6130 = ORIENTED_EDGE ( 'NONE', *, *, #32264, .F. ) ;
#6131 = CARTESIAN_POINT ( 'NONE',  ( 792.1044303154645831, -276.4527844766013800, 317.8323909638837677 ) ) ;
#6132 = CARTESIAN_POINT ( 'NONE',  ( 815.2698199232961542, 7.183579159761247723, 342.5225473063383106 ) ) ;
#6133 = CARTESIAN_POINT ( 'NONE',  ( 755.5713283507202505, -173.3618753856927128, -334.6858677611754729 ) ) ;
#6134 = CARTESIAN_POINT ( 'NONE',  ( 788.8264449731200330, -381.1800572038737869, 363.6646147819171233 ) ) ;
#6135 = CARTESIAN_POINT ( 'NONE',  ( 772.5602148656447525, -129.7255117493292289, -305.7998596910095443 ) ) ;
#6136 = AXIS2_PLACEMENT_3D ( 'NONE', #41745, #16807, #27880 ) ;
#6137 = CARTESIAN_POINT ( 'NONE',  ( 804.9363028652555840, -112.2709662947838325, -338.2165204200192079 ) ) ;
#6138 = ORIENTED_EDGE ( 'NONE', *, *, #35330, .F. ) ;
#6139 = CARTESIAN_POINT ( 'NONE',  ( 790.0220218866281812, -55.09997266333508747, -363.2186876482849129 ) ) ;
#6140 = AXIS2_PLACEMENT_3D ( 'NONE', #29829, #33296, #19209 ) ;
#6141 = CARTESIAN_POINT ( 'NONE',  ( 780.5236548040995785, -356.7363362996978253, -314.9735926884559944 ) ) ;
#6143 = CARTESIAN_POINT ( 'NONE',  ( 755.1538015810308480, -398.1908817542431507, 343.0433043558613804 ) ) ;
#6142 = CARTESIAN_POINT ( 'NONE',  ( 781.7834795799800531, -106.8164208402383935, 315.0636971347436202 ) ) ;
#6146 = CARTESIAN_POINT ( 'NONE',  ( 764.3348316497523456, -358.7146871989592114, 308.6759233522265617 ) ) ;
#6145 = DIRECTION ( 'NONE',  ( 0.000000000000000000, 0.000000000000000000, 1.000000000000000000 ) ) ;
#6144 = CARTESIAN_POINT ( 'NONE',  ( 815.2698199232962679, -448.8164208402372424, 342.5225473063383674 ) ) ;
#6147 = CARTESIAN_POINT ( 'NONE',  ( 756.1443688327750579, -117.6237781080509279, 314.3581564841659315 ) ) ;
#6148 = CARTESIAN_POINT ( 'NONE',  ( 790.9844846989617508, -358.3726999360613945, -317.2208543904092721 ) ) ;
#6149 = CARTESIAN_POINT ( 'NONE',  ( 801.9419747391806368, -306.4527844766013800, -351.9812246680014027 ) ) ;
#6150 = CARTESIAN_POINT ( 'NONE',  ( 793.5525998758768083, -151.0999726633347677, -372.6845335610516941 ) ) ;
#6151 = CARTESIAN_POINT ( 'NONE',  ( 773.7305795820266212, -9.281790845153418346, 374.8230680027170365 ) ) ;
#6152 = VECTOR ( 'NONE', #6590, 1000.000000000000000 ) ;
#6154 = CARTESIAN_POINT ( 'NONE',  ( 879.9999999999990905, -414.5899773927342835, -210.0000000000000000 ) ) ;
#6153 = CARTESIAN_POINT ( 'NONE',  ( -468.8365100919714337, 260.0000000000001705, -199.9999999999908766 ) ) ;
#6155 = CARTESIAN_POINT ( 'NONE',  ( 769.1273215169530886, -262.7146871989594956, -317.4527132478988847 ) ) ;
#6156 = CARTESIAN_POINT ( 'NONE',  ( 815.3608509340175488, -146.7363362996984506, -341.2497674668889545 ) ) ;
#6157 = LINE ( 'NONE', #1765, #15302 ) ;
#6158 = DIRECTION ( 'NONE',  ( 1.000000000000000000, 0.000000000000000000, 0.000000000000000000 ) ) ;
#6159 = CARTESIAN_POINT ( 'NONE',  ( 755.5913626894240451, -325.6454272087888739, 346.6156483768012890 ) ) ;
#6160 = ORIENTED_EDGE ( 'NONE', *, *, #25270, .F. ) ;
#6161 = CARTESIAN_POINT ( 'NONE',  ( 795.8262568251477660, -310.3726999360616219, 308.3538107759623585 ) ) ;
#6162 = CARTESIAN_POINT ( 'NONE',  ( 812.7932403749906598, -183.1800572038744974, -327.7687537140311633 ) ) ;
#6163 = DIRECTION ( 'NONE',  ( -1.000000000000000000, -0.000000000000000000, -0.000000000000000000 ) ) ;
#6164 = CARTESIAN_POINT ( 'NONE',  ( 815.3608509340175488, -122.7363362996985074, 341.2497674668889545 ) ) ;
#6165 = CARTESIAN_POINT ( 'NONE',  ( 755.2512626584698410, -295.5436935675105588, -315.2512626584710915 ) ) ;
#6166 = CARTESIAN_POINT ( 'NONE',  ( -879.9999999999992042, 529.9999999999997726, -320.0000000000000000 ) ) ;
#6167 = LINE ( 'NONE', #2941, #28653 ) ;
#6168 = CARTESIAN_POINT ( 'NONE',  ( 771.2633955100217236, -143.9073299311473590, 363.4237431249939618 ) ) ;
#6169 = VECTOR ( 'NONE', #25084, 1000.000000000000000 ) ;
#6170 = ORIENTED_EDGE ( 'NONE', *, *, #24477, .T. ) ;
#6171 = CARTESIAN_POINT ( 'NONE',  ( 797.8822607201568644, -414.5545181178795247, 370.1134526219340160 ) ) ;
#6172 = CARTESIAN_POINT ( 'NONE',  ( 778.7502325331095108, -360.3510508353228374, -304.6391490659818828 ) ) ;
#6173 = VECTOR ( 'NONE', #12244, 999.9999999999998863 ) ;
#6174 = CARTESIAN_POINT ( 'NONE',  ( 792.2312462859673587, -107.9073299311474727, -307.2067596250082602 ) ) ;
#6175 = CARTESIAN_POINT ( 'NONE',  ( 790.0220218866281812, -55.09997266333508747, 363.2186876482849129 ) ) ;
#6176 = CARTESIAN_POINT ( 'NONE',  ( 755.2512626584698410, -391.5436935675101608, -315.2512626584710915 ) ) ;
#6177 = FACE_BOUND ( 'NONE', #14391, .T. ) ;
#6178 = CARTESIAN_POINT ( 'NONE',  ( 798.0661480581538854, 21.46713098285774279, 309.5768839229118043 ) ) ;
#6179 = EDGE_LOOP ( 'NONE', ( #8966, #14743, #44375, #33457 ) ) ;
#6180 = CARTESIAN_POINT ( 'NONE',  ( 745.1769319972822814, -137.8055962898690154, -346.2694204179732083 ) ) ;
#6181 = CARTESIAN_POINT ( 'NONE',  ( 799.9999999999993179, -462.9681489794448339, -370.0000000000000568 ) ) ;
#6182 = CARTESIAN_POINT ( 'NONE',  ( 778.7502325331095108, -288.3510508353231216, 304.6391490659818828 ) ) ;
#6183 = CARTESIAN_POINT ( 'NONE',  ( 767.8955696845334842, -96.45278447660204790, 362.1676090361161755 ) ) ;
#6184 = ORIENTED_EDGE ( 'NONE', *, *, #26462, .T. ) ;
#6185 = CARTESIAN_POINT ( 'NONE',  ( 803.8651313633788504, -5.260141744414903897, -332.4468031744301015 ) ) ;
#6186 = CARTESIAN_POINT ( 'NONE',  ( 804.4286716492782716, -281.3618753856923718, 345.3141322388244703 ) ) ;
#6187 = CARTESIAN_POINT ( 'NONE',  ( 812.7932403749906598, 8.819942796124882634, -327.7687537140311633 ) ) ;
#6188 = LINE ( 'NONE', #17048, #15072 ) ;
#6189 = EDGE_LOOP ( 'NONE', ( #30273, #41536 ) ) ;
#6190 = CARTESIAN_POINT ( 'NONE',  ( 786.2694204179717872, -405.2817908451522158, -305.1769319972829067 ) ) ;
#6191 = CARTESIAN_POINT ( 'NONE',  ( 797.8594530101008786, -277.5436935675105019, -322.1405469898980982 ) ) ;
#6193 = CARTESIAN_POINT ( 'NONE',  ( 768.8385539511368734, -263.2601417444141134, 306.4236121716840557 ) ) ;
#6192 = CARTESIAN_POINT ( 'NONE',  ( 782.5225473063383106, -358.2709662947830225, 375.2698199232970637 ) ) ;
#6194 = CARTESIAN_POINT ( 'NONE',  ( 798.5707757039680246, -269.4636090269708006, -356.7845633553585003 ) ) ;
#6195 = CARTESIAN_POINT ( 'NONE',  ( 771.1735550268778070, -225.1800572038743269, -316.3353852180827630 ) ) ;
#6196 = VECTOR ( 'NONE', #32919, 1000.000000000000000 ) ;
#6197 = CARTESIAN_POINT ( 'NONE',  ( 778.1981804954715471, -418.2709662947828519, -314.8072714833591021 ) ) ;
#6198 = CARTESIAN_POINT ( 'NONE',  ( 756.5762568750052424, -243.1800572038743269, 348.7366044899774238 ) ) ;
#6199 = ORIENTED_EDGE ( 'NONE', *, *, #11210, .F. ) ;
#6200 = CARTESIAN_POINT ( 'NONE',  ( 758.8095938919642549, -368.0891481129647786, 311.6929314249763365 ) ) ;
#6201 = CARTESIAN_POINT ( 'NONE',  ( 790.0183182880230106, -452.9681489794449476, -362.9048749981275250 ) ) ;
#6202 = CARTESIAN_POINT ( 'NONE',  ( 747.6481478633932056, -13.09997266333522248, -353.4146539503763620 ) ) ;
#6203 = CARTESIAN_POINT ( 'NONE',  ( 788.0874520139973356, 16.45630643248838609, 314.0623709945898554 ) ) ;
#6204 = CARTESIAN_POINT ( 'NONE',  ( 799.9999999999993179, 166.4563064324884465, -319.9999999999999432 ) ) ;
#6205 = CARTESIAN_POINT ( 'NONE',  ( 757.4527132478984868, -232.3726999360617924, 329.1273215169538844 ) ) ;
#6206 = CARTESIAN_POINT ( 'NONE',  ( 764.8639956371174549, -128.0891481129655176, 319.7806653035542013 ) ) ;
#6207 = ORIENTED_EDGE ( 'NONE', *, *, #26420, .F. ) ;
#6208 = CARTESIAN_POINT ( 'NONE',  ( 746.4236121716829757, -447.8272453906067199, -328.8385539511384650 ) ) ;
#6209 = CARTESIAN_POINT ( 'NONE',  ( 767.6429770376291799, -81.18005720387482427, -306.8695393053162093 ) ) ;
#6210 = CARTESIAN_POINT ( 'NONE',  ( 802.7791456095903868, -244.7146871989596093, 329.0155153010375102 ) ) ;
#6211 = CARTESIAN_POINT ( 'NONE',  ( 755.5713283507202505, -437.3618753856919170, -334.6858677611754729 ) ) ;
#6212 = CARTESIAN_POINT ( 'NONE',  ( 771.2633955100217236, -47.90732993114767169, -363.4237431249939618 ) ) ;
#6213 = VECTOR ( 'NONE', #15908, 1000.000000000000114 ) ;
#6214 = CARTESIAN_POINT ( 'NONE',  ( 793.3938497862117174, -453.0432664090020012, 372.3358127763067955 ) ) ;
#6215 = CARTESIAN_POINT ( 'NONE',  ( 800.2193346964447755, 5.001760977943074948, -355.1360043628815788 ) ) ;
#6216 = CARTESIAN_POINT ( 'NONE',  ( 758.8095938919642549, -200.0891481129653187, -311.6929314249763365 ) ) ;
#6217 = CIRCLE ( 'NONE', #40164, 20.00000000000001776 ) ;
#6218 = CARTESIAN_POINT ( 'NONE',  ( 745.7998596910086917, -101.3618753856929544, 332.5602148656461168 ) ) ;
#6219 = CARTESIAN_POINT ( 'NONE',  ( 815.2698199232961542, -184.8164208402380950, 342.5225473063383106 ) ) ;
#6220 = DIRECTION ( 'NONE',  ( -0.000000000000000000, 1.000000000000000000, -0.000000000000000000 ) ) ;
#6221 = CARTESIAN_POINT ( 'NONE',  ( 999.5857864376259840, 479.9999999999999432, -360.0000000000000000 ) ) ;
#6222 = CARTESIAN_POINT ( 'NONE',  ( 788.7631598425961101, -289.4419599262321299, -305.7194118038759143 ) ) ;
#6223 = CARTESIAN_POINT ( 'NONE',  ( 773.7305795820266212, -417.2817908451522158, 374.8230680027170365 ) ) ;
#6224 = CARTESIAN_POINT ( 'NONE',  ( 777.4774526936600978, -274.2709662947833067, -304.7301800767027657 ) ) ;
#6225 = CARTESIAN_POINT ( 'NONE',  ( 959.5497976682736407, 120.6654763175833693, -209.9999999999999716 ) ) ;
#6226 = CARTESIAN_POINT ( 'NONE',  ( 744.7301800767019131, -388.8164208402374129, 337.4774526936615757 ) ) ;
#6227 = CARTESIAN_POINT ( 'NONE',  ( 772.4837098697145166, 0.6381246143067237364, 374.5518280994205611 ) ) ;
#6228 = CARTESIAN_POINT ( 'NONE',  ( 759.7806653035534055, -342.9982390220557136, -324.8639956371180801 ) ) ;
#6229 = CLOSED_SHELL ( 'NONE', ( #10346, #12867, #37117, #1530, #18516, #8801, #36126, #7214, #32583, #4084, #43045, #19268, #33761, #23580, #4988, #36322, #44499, #16813, #16830, #24365, #43560, #33510, #24320, #12302 ) ) ;
#6230 = CARTESIAN_POINT ( 'NONE',  ( 764.0069404352550464, -15.07832356259669560, 359.2566176426627180 ) ) ;
#6231 = AXIS2_PLACEMENT_3D ( 'NONE', #9528, #43942, #16447 ) ;
#6232 = CARTESIAN_POINT ( 'NONE',  ( 783.7566961878529810, -48.89650538077840025, -305.1792804349288417 ) ) ;
#6233 = CARTESIAN_POINT ( 'NONE',  ( 795.9930595647434757, -147.0783235625962959, -320.7433823573372820 ) ) ;
#6234 = CARTESIAN_POINT ( 'NONE',  ( 761.9338519418445230, -182.5328690171416497, 370.4231160770881957 ) ) ;
#6235 = LINE ( 'NONE', #9934, #7777 ) ;
#6236 = AXIS2_PLACEMENT_3D ( 'NONE', #8173, #15334, #4261 ) ;
#6237 = CARTESIAN_POINT ( 'NONE',  ( 771.2368401574024119, -181.4419599262325278, 374.2805881961240857 ) ) ;
#6238 = ORIENTED_EDGE ( 'NONE', *, *, #27806, .T. ) ;
#6239 = CARTESIAN_POINT ( 'NONE',  ( 756.5762568750052424, -75.18005720387485269, -348.7366044899774238 ) ) ;
#6240 = CARTESIAN_POINT ( 'NONE',  ( 804.9511171171677688, -149.8055962898689870, -335.8780910478229202 ) ) ;
#6241 = UNCERTAINTY_MEASURE_WITH_UNIT (LENGTH_MEASURE( 1.000000000000000082E-05 ), #45148, 'distance_accuracy_value', 'NONE');
#6242 = CARTESIAN_POINT ( 'NONE',  ( 781.8018195045266339, -166.2709662947835909, 365.1927285166406705 ) ) ;
#6243 = CARTESIAN_POINT ( 'NONE',  ( 815.0009284576459549, 17.64894916467593688, -338.7629533639073429 ) ) ;
#6245 = CARTESIAN_POINT ( 'NONE',  ( 785.3141322388236176, -285.7255117493286889, 364.4286716492789537 ) ) ;
#6244 = CARTESIAN_POINT ( 'NONE',  ( 755.5713283507202505, -293.3618753856923718, 334.6858677611754729 ) ) ;
#6246 = CARTESIAN_POINT ( 'NONE',  ( 355.8971257818259915, 290.0000000000001137, -244.9999999999999716 ) ) ;
#6247 = ORIENTED_EDGE ( 'NONE', *, *, #11400, .F. ) ;
#6248 = CARTESIAN_POINT ( 'NONE',  ( 783.0433043558608688, -24.89650538077847486, 315.1538015810313027 ) ) ;
#6249 = CARTESIAN_POINT ( 'NONE',  ( 755.8990559732751535, -323.4636090269706301, -365.9055244015606831 ) ) ;
#6250 = AXIS2_PLACEMENT_3D ( 'NONE', #27206, #16590, #30672 ) ;
#6251 = APPLICATION_PROTOCOL_DEFINITION ( 'draft international standard', 'automotive_design', 1998, #19019 ) ;
#6252 = AXIS2_PLACEMENT_3D ( 'NONE', #39369, #28745, #7499 ) ;
#6253 = CARTESIAN_POINT ( 'NONE',  ( 745.0891759886404770, -220.2709662947834772, 342.4968714119734159 ) ) ;
#6254 = CARTESIAN_POINT ( 'NONE',  ( 786.5483106153019435, -343.6454272087887603, 364.1601925771022366 ) ) ;
#6255 = VECTOR ( 'NONE', #44220, 1000.000000000000000 ) ;
#6256 = CARTESIAN_POINT ( 'NONE',  ( 804.1601925771018387, -439.4419599262316751, 346.5483106153029098 ) ) ;
#6257 = CARTESIAN_POINT ( 'NONE',  ( 760.7433823573367135, -132.0090635724257595, -355.9930595647440441 ) ) ;
#6258 = CARTESIAN_POINT ( 'NONE',  ( 804.9363028652555840, -112.2709662947838325, -338.2165204200192079 ) ) ;
#6259 = CARTESIAN_POINT ( 'NONE',  ( 781.7834795799800531, -322.8164208402377540, -315.0636971347436202 ) ) ;
#6260 = ORIENTED_EDGE ( 'NONE', *, *, #33421, .F. ) ;
#6261 = CARTESIAN_POINT ( 'NONE',  ( 802.1676090361156639, -446.6346026584189985, -327.8955696845344505 ) ) ;
#6262 = CARTESIAN_POINT ( 'NONE',  ( 763.2154366446407039, -285.6237781080502600, 321.4292242960311228 ) ) ;
#6263 = CARTESIAN_POINT ( 'NONE',  ( 829.9999999999992042, -600.0000000000000000, -320.0000000000000568 ) ) ;
#6264 = CARTESIAN_POINT ( 'NONE',  ( -911.9749999999993406, 154.9999999999998863, 350.0000000000000000 ) ) ;
#6265 = AXIS2_PLACEMENT_3D ( 'NONE', #5840, #30781, #19926 ) ;
#6266 = CARTESIAN_POINT ( 'NONE',  ( 786.5483106153019435, -127.6454272087894140, 364.1601925771022366 ) ) ;
#6267 = LINE ( 'NONE', #30764, #516 ) ;
#6268 = ORIENTED_EDGE ( 'NONE', *, *, #138, .T. ) ;
#6269 = CARTESIAN_POINT ( 'NONE',  ( 813.5763878283155464, -339.8272453906069472, -351.1614460488615350 ) ) ;
#6270 = VECTOR ( 'NONE', #10375, 1000.000000000000000 ) ;
#6271 = CARTESIAN_POINT ( 'NONE',  ( 781.2370466360911223, -236.7363362996981380, 304.9990715423533629 ) ) ;
#6272 = AXIS2_PLACEMENT_3D ( 'NONE', #21978, #32598, #36284 ) ;
#6273 = CARTESIAN_POINT ( 'NONE',  ( 754.8072714833581358, -316.8164208402377540, -338.1981804954720587 ) ) ;
#6274 = DIRECTION ( 'NONE',  ( -0.000000000000000000, 1.000000000000000000, -0.000000000000000000 ) ) ;
#6275 = CARTESIAN_POINT ( 'NONE',  ( 755.1538015810308480, -182.1908817542437760, -343.0433043558613804 ) ) ;
#6276 = ADVANCED_FACE ( 'NONE', ( #42130 ), #13506, .T. ) ;
#6277 = CARTESIAN_POINT ( 'NONE',  ( 812.7932403749906598, -63.18005720387488822, 327.7687537140311633 ) ) ;
#6278 = CARTESIAN_POINT ( 'NONE',  ( 807.0960494954803153, -452.9681489794450613, 341.9322302743943851 ) ) ;
#6280 = VECTOR ( 'NONE', #38725, 1000.000000000000000 ) ;
#6279 = CARTESIAN_POINT ( 'NONE',  ( 792.2312462859673587, -371.9073299311465917, -307.2067596250082602 ) ) ;
#6281 = DIRECTION ( 'NONE',  ( 1.892425610156518354E-16, 1.000000000000000000, -0.000000000000000000 ) ) ;
#6282 = VECTOR ( 'NONE', #33387, 1000.000000000000000 ) ;
#6283 = CARTESIAN_POINT ( 'NONE',  ( 788.6739635108323228, -319.6454272087888739, 373.9316612368139090 ) ) ;
#6284 = CARTESIAN_POINT ( 'NONE',  ( 804.7487373415286811, -283.5436935675105019, 364.7487373415288516 ) ) ;
#6285 = CARTESIAN_POINT ( 'NONE',  ( 787.5162901302840055, -11.36187538569323863, -305.4481719005792684 ) ) ;
#6286 = EDGE_CURVE ( 'NONE', #36310, #21150, #26154, .T. ) ;
#6287 = CARTESIAN_POINT ( 'NONE',  ( 801.9419747391806368, -234.4527844766016358, -351.9812246680014027 ) ) ;
#6288 = CIRCLE ( 'NONE', #44636, 2.749999999999919176 ) ;
#6289 = CARTESIAN_POINT ( 'NONE',  ( 928.0249999999991815, 219.9999999999998863, 350.0000000000000000 ) ) ;
#6290 = CARTESIAN_POINT ( 'NONE',  ( 767.8955696845333705, -384.4527844766011526, 362.1676090361162323 ) ) ;
#6291 = CARTESIAN_POINT ( 'NONE',  ( 757.4527132478984868, -160.3726999360620482, 329.1273215169538844 ) ) ;
#6292 = CARTESIAN_POINT ( 'NONE',  ( 760.5453621957607311, -45.07832356259660145, -323.8424801807151425 ) ) ;
#6293 = CARTESIAN_POINT ( 'NONE',  ( 810.1134526219336749, -56.53286901714201917, 357.8822607201570349 ) ) ;
#6294 = CARTESIAN_POINT ( 'NONE',  ( 757.8323909638828582, -362.6346026584193964, 352.1044303154654358 ) ) ;
#6295 = LINE ( 'NONE', #17149, #36528 ) ;
#6296 = DIRECTION ( 'NONE',  ( -0.000000000000000000, 1.000000000000000000, -0.000000000000000000 ) ) ;
#6297 = CARTESIAN_POINT ( 'NONE',  ( 746.0683387631852383, -139.4419599262326699, 331.3260364891676204 ) ) ;
#6298 = CARTESIAN_POINT ( 'NONE',  ( 803.4237431249931660, -447.1800572038736732, 331.2633955100225194 ) ) ;
#6299 = ORIENTED_EDGE ( 'NONE', *, *, #26147, .F. ) ;
#6300 = CARTESIAN_POINT ( 'NONE',  ( 791.9812246680005501, -68.63460265842033436, -361.9419747391813189 ) ) ;
#6301 = CARTESIAN_POINT ( 'NONE',  ( 783.0433043558608688, -360.8965053807773984, -315.1538015810313027 ) ) ;
#6303 = CARTESIAN_POINT ( 'NONE',  ( 756.3353852180820240, -173.9073299311472454, 331.1735550268787733 ) ) ;
#6302 = CARTESIAN_POINT ( 'NONE',  ( 804.6798772138708955, -207.7255117493289447, 334.6312213355107019 ) ) ;
#6304 = AXIS2_PLACEMENT_3D ( 'NONE', #873, #8267, #7828 ) ;
#6305 = CARTESIAN_POINT ( 'NONE',  ( 803.8556311672234642, -369.6237781080500895, -365.6418435158340117 ) ) ;
#6306 = DIRECTION ( 'NONE',  ( 0.000000000000000000, 0.000000000000000000, -1.000000000000000000 ) ) ;
#6307 = VERTEX_POINT ( 'NONE', #31725 ) ;
#6308 = CARTESIAN_POINT ( 'NONE',  ( 756.5762568750052424, -387.1800572038738437, 348.7366044899774238 ) ) ;
#6309 = CIRCLE ( 'NONE', #32129, 2.749999999999919176 ) ;
#6310 = EDGE_CURVE ( 'NONE', #6, #26042, #34965, .T. ) ;
#6311 = EDGE_LOOP ( 'NONE', ( #29313, #22494, #1938, #24019 ) ) ;
#6312 =( NAMED_UNIT ( * ) SI_UNIT ( $, .STERADIAN. ) SOLID_ANGLE_UNIT ( ) );
#6313 = AXIS2_PLACEMENT_3D ( 'NONE', #11902, #1049, #25075 ) ;
#6314 = CARTESIAN_POINT ( 'NONE',  ( 814.5518280994195948, -231.7255117493288310, -332.4837098697145734 ) ) ;
#6315 = CARTESIAN_POINT ( 'NONE',  ( 767.6429770376291799, -129.1800572038746679, 306.8695393053162093 ) ) ;
#6316 = ORIENTED_EDGE ( 'NONE', *, *, #42173, .T. ) ;
#6317 = CARTESIAN_POINT ( 'NONE',  ( 785.3687786644885591, -227.3618753856925423, -315.3201227861280813 ) ) ;
#6318 = VERTEX_POINT ( 'NONE', #17432 ) ;
#6319 = CARTESIAN_POINT ( 'NONE',  ( 803.6646147819161570, 6.092670068852159559, -348.8264449731210561 ) ) ;
#6320 = MECHANICAL_DESIGN_GEOMETRIC_PRESENTATION_REPRESENTATION (  '', ( #1887 ), #7831 ) ;
#6321 = CARTESIAN_POINT ( 'NONE',  ( 764.0069404352550464, -183.0783235625961538, 359.2566176426627180 ) ) ;
#6323 = FACE_OUTER_BOUND ( 'NONE', #17699, .T. ) ;
#6322 = DIRECTION ( 'NONE',  ( -0.000000000000000000, 1.000000000000000000, -0.000000000000000000 ) ) ;
#6324 = CARTESIAN_POINT ( 'NONE',  ( 794.9999999999993179, 197.3292319334027241, 273.4704985657796783 ) ) ;
#6325 = AXIS2_PLACEMENT_3D ( 'NONE', #14699, #17921, #363 ) ;
#6326 = PRODUCT ( 'MirrorHeavy Cast Iron Table Bed Base', 'MirrorHeavy Cast Iron Table Bed Base', '', ( #21430 ) ) ;
#6327 = ORIENTED_EDGE ( 'NONE', *, *, #20624, .F. ) ;
#6328 = CARTESIAN_POINT ( 'NONE',  ( 802.9823548866075953, -457.0999726633339151, -330.0799878456151077 ) ) ;
#6329 = PLANE ( 'NONE',  #35084 ) ;
#6330 = CARTESIAN_POINT ( 'NONE',  ( 8.295132257852724189E-14, 199.9999999999999147, 339.9999999999999432 ) ) ;
#6331 = CARTESIAN_POINT ( 'NONE',  ( 804.1009440267234822, -239.4636090269709143, -314.0944755984392600 ) ) ;
#6332 = CARTESIAN_POINT ( 'NONE',  ( 746.4236121716829757, -87.82724539060770041, 328.8385539511384650 ) ) ;
#6334 = CARTESIAN_POINT ( 'NONE',  ( 757.8323909638827445, -218.6346026584197944, -352.1044303154654358 ) ) ;
#6333 = FACE_BOUND ( 'NONE', #3325, .T. ) ;
#6335 = EDGE_CURVE ( 'NONE', #28948, #30680, #35859, .T. ) ;
#6336 = CARTESIAN_POINT ( 'NONE',  ( 800.7704444035546203, -388.1692326535045936, -326.0291762391768771 ) ) ;
#6337 = CARTESIAN_POINT ( 'NONE',  ( 745.5313806188320314, -255.2817908451526705, -333.7943932421247268 ) ) ;
#6338 = FILL_AREA_STYLE ('',( #3574 ) ) ;
#6339 = CARTESIAN_POINT ( 'NONE',  ( 799.9999999999993179, -462.9681489794448339, -309.9999999999998863 ) ) ;
#6340 = CARTESIAN_POINT ( 'NONE',  ( 784.1219089521767955, -69.28179084515321051, -315.0488828828318333 ) ) ;
#6341 = CARTESIAN_POINT ( 'NONE',  ( 763.8424801807145741, -450.0090635724248500, 320.5453621957614700 ) ) ;
#6342 = EDGE_CURVE ( 'NONE', #4067, #1813, #42351, .T. ) ;
#6343 = DIRECTION ( 'NONE',  ( -0.000000000000000000, 1.000000000000000000, -0.000000000000000000 ) ) ;
#6344 = CARTESIAN_POINT ( 'NONE',  ( 765.8855110935204493, -430.1692326535043094, -319.0159684113471599 ) ) ;
#6345 = CARTESIAN_POINT ( 'NONE',  ( 772.4837098697145166, -263.3618753856924286, -374.5518280994205611 ) ) ;
#6346 = DIRECTION ( 'NONE',  ( 0.000000000000000000, 1.000000000000000000, 1.056348263647623421E-15 ) ) ;
#6347 = FACE_OUTER_BOUND ( 'NONE', #897, .T. ) ;
#6348 = CARTESIAN_POINT ( 'NONE',  ( 774.6858677611749044, -81.72551174932937101, -315.5713283507209894 ) ) ;
#6349 = VECTOR ( 'NONE', #44431, 1000.000000000000000 ) ;
#6350 = CARTESIAN_POINT ( 'NONE',  ( 788.6739635108323228, -199.6454272087891582, 373.9316612368139090 ) ) ;
#6351 = CARTESIAN_POINT ( 'NONE',  ( 813.9316612368132837, -151.4419599262326415, -348.6739635108323228 ) ) ;
#6352 = CARTESIAN_POINT ( 'NONE',  ( 749.2812353651451076, -174.4527844766018063, 323.2262854647983090 ) ) ;
#6353 = CIRCLE ( 'NONE', #9935, 2.749999999999919176 ) ;
#6354 = CARTESIAN_POINT ( 'NONE',  ( 814.2001403089898304, -425.3618753856919170, -347.4397851343538264 ) ) ;
#6355 = EDGE_CURVE ( 'NONE', #15790, #30506, #3097, .T. ) ;
#6356 = EDGE_CURVE ( 'NONE', #7990, #28297, #7271, .T. ) ;
#6357 = FACE_OUTER_BOUND ( 'NONE', #38991, .T. ) ;
#6358 = CARTESIAN_POINT ( 'NONE',  ( 792.1044303154645831, -300.4527844766012663, 317.8323909638837677 ) ) ;
#6359 = CARTESIAN_POINT ( 'NONE',  ( 780.5236548040995785, -44.73633629969875614, 314.9735926884559944 ) ) ;
#6360 = CARTESIAN_POINT ( 'NONE',  ( 755.5713283507202505, -413.3618753856920307, -334.6858677611754729 ) ) ;
#6361 = AXIS2_PLACEMENT_3D ( 'NONE', #38757, #34597, #27897 ) ;
#6362 = CARTESIAN_POINT ( 'NONE',  ( 799.9999999999993179, 205.0000000000000568, 329.9999999999999432 ) ) ;
#6363 = DIRECTION ( 'NONE',  ( 0.000000000000000000, -0.7651688349527138167, -0.6438296778008192334 ) ) ;
#6365 = CARTESIAN_POINT ( 'NONE',  ( 758.0580252608178853, -318.4527844766014368, 328.0187753319985404 ) ) ;
#6364 = CARTESIAN_POINT ( 'NONE',  ( 798.7617431975189675, -123.6237781080508569, 323.0428371773161871 ) ) ;
#6366 = ORIENTED_EDGE ( 'NONE', *, *, #8029, .T. ) ;
#6367 = VECTOR ( 'NONE', #21963, 1000.000000000000000 ) ;
#6368 = CARTESIAN_POINT ( 'NONE',  ( 799.4546378042377910, -273.0783235625958696, -356.1575198192848006 ) ) ;
#6369 = CARTESIAN_POINT ( 'NONE',  ( 757.8323909638827445, -122.6346026584201354, -352.1044303154654358 ) ) ;
#6370 = CARTESIAN_POINT ( 'NONE',  ( 788.8264449731200330, -93.18005720387481006, 363.6646147819171233 ) ) ;
#6371 = CARTESIAN_POINT ( 'NONE',  ( 786.2056067578752163, -251.8055962898686744, -374.4686193811670023 ) ) ;
#6372 = DIRECTION ( 'NONE',  ( 0.000000000000000000, -1.000000000000000000, 0.000000000000000000 ) ) ;
#6373 = CARTESIAN_POINT ( 'NONE',  ( 781.2497674668890113, -396.3510508353228374, 375.3608509340180603 ) ) ;
#6374 = ADVANCED_FACE ( 'NONE', ( #2878, #6567 ), #21116, .F. ) ;
#6375 = ORIENTED_EDGE ( 'NONE', *, *, #17668, .T. ) ;
#6376 = CARTESIAN_POINT ( 'NONE',  ( 764.8639956371174549, -272.0891481129651197, 319.7806653035542013 ) ) ;
#6377 = EDGE_CURVE ( 'NONE', #5448, #8915, #17188, .T. ) ;
#6378 = CARTESIAN_POINT ( 'NONE',  ( 766.7756240680305382, -62.53286901714199786, -361.5560724626415663 ) ) ;
#6379 = CARTESIAN_POINT ( 'NONE',  ( 805.1927285166397041, -160.8164208402382371, -341.8018195045277707 ) ) ;
#6380 = CARTESIAN_POINT ( 'NONE',  ( 759.9864689768902508, -362.0891481129648923, 354.9819416627836404 ) ) ;
#6381 = CARTESIAN_POINT ( 'NONE',  ( 796.9462024416508257, -108.4527844766019911, -308.9653473494370246 ) ) ;
#6382 = CARTESIAN_POINT ( 'NONE',  ( 804.4286716492782716, -113.3618753856929260, -345.3141322388244703 ) ) ;
#6383 = VERTEX_POINT ( 'NONE', #41914 ) ;
#6384 = CARTESIAN_POINT ( 'NONE',  ( 772.4468031744293057, -57.82724539060780700, -363.8651313633793620 ) ) ;
#6385 = CIRCLE ( 'NONE', #3451, 19.99999999999990763 ) ;
#6386 = CARTESIAN_POINT ( 'NONE',  ( 804.6971507214547046, -339.2817908451524431, -344.0799538623459739 ) ) ;
#6388 = CARTESIAN_POINT ( 'NONE',  ( 758.4439275373578084, -396.5545181178794678, 353.2243759319684386 ) ) ;
#6387 = CARTESIAN_POINT ( 'NONE',  ( 804.4286716492782716, -137.3618753856928265, 345.3141322388244703 ) ) ;
#6389 = VECTOR ( 'NONE', #40428, 1000.000000000000114 ) ;
#6392 = CARTESIAN_POINT ( 'NONE',  ( 759.8311093483677041, -358.1692326535047641, 310.9282345327691814 ) ) ;
#6391 = FACE_OUTER_BOUND ( 'NONE', #12985, .T. ) ;
#6390 = CARTESIAN_POINT ( 'NONE',  ( 810.7187646348534145, -450.4527844766009821, 356.7737145352016341 ) ) ;
#6393 = CARTESIAN_POINT ( 'NONE',  ( 796.9571628226829034, -359.4636090269705164, -321.2382568024804641 ) ) ;
#6394 = CARTESIAN_POINT ( 'NONE',  ( 778.1981804954714335, -346.2709662947830793, -314.8072714833589885 ) ) ;
#6395 = AXIS2_PLACEMENT_3D ( 'NONE', #25603, #43592, #39238 ) ;
#6396 = CARTESIAN_POINT ( 'NONE',  ( 750.9282345327678740, -136.9181544815166376, -319.8311093483690115 ) ) ;
#6397 = CARTESIAN_POINT ( 'NONE',  ( 797.8822607201568644, -6.554518117880697048, 370.1134526219340160 ) ) ;
#6399 = FACE_OUTER_BOUND ( 'NONE', #38480, .T. ) ;
#6398 = DIRECTION ( 'NONE',  ( -0.000000000000000000, -0.000000000000000000, 1.000000000000000000 ) ) ;
#6400 = EDGE_CURVE ( 'NONE', #3030, #22719, #35200, .T. ) ;
#6401 = CARTESIAN_POINT ( 'NONE',  ( 754.9735926884551418, -258.3510508353231785, -340.5236548041000333 ) ) ;
#6402 = CARTESIAN_POINT ( 'NONE',  ( 814.8207195650702488, -170.1908817542438328, -336.2433038121456548 ) ) ;
#6403 = CARTESIAN_POINT ( 'NONE',  ( 879.9999999999992042, 99.99999999999984368, -360.0000000000000000 ) ) ;
#6404 = CARTESIAN_POINT ( 'NONE',  ( 939.9999999999993179, -416.7569064942979935, -212.5753187112032947 ) ) ;
#6405 = CARTESIAN_POINT ( 'NONE',  ( 754.7162404726377645, -326.7363362996979390, 339.4709603349214717 ) ) ;
#6406 = ADVANCED_FACE ( 'NONE', ( #24335 ), #45145, .T. ) ;
#6407 = CARTESIAN_POINT ( 'NONE',  ( 755.8990559732751535, -299.4636090269707438, 365.9055244015606831 ) ) ;
#6408 = CARTESIAN_POINT ( 'NONE',  ( 804.7487373415286811, -187.5436935675108430, -364.7487373415288516 ) ) ;
#6409 = CYLINDRICAL_SURFACE ( 'NONE', #8359, 2.749999999999863665 ) ;
#6410 = CARTESIAN_POINT ( 'NONE',  ( 814.2805881961230625, -121.6454272087894282, 331.2368401574024119 ) ) ;
#6411 = CARTESIAN_POINT ( 'NONE',  ( 749.2812353651451076, -318.4527844766014368, -323.2262854647983090 ) ) ;
#6412 = CYLINDRICAL_SURFACE ( 'NONE', #42927, 8.024999999999948841 ) ;
#6413 = DIRECTION ( 'NONE',  ( -0.000000000000000000, 1.000000000000000000, -0.000000000000000000 ) ) ;
#6414 = CARTESIAN_POINT ( 'NONE',  ( 792.1044303154645831, -180.4527844766017211, 317.8323909638837677 ) ) ;
#6415 = ORIENTED_EDGE ( 'NONE', *, *, #6651, .F. ) ;
#6416 = CARTESIAN_POINT ( 'NONE',  ( 786.2694204179717872, -429.2817908451521021, 305.1769319972829067 ) ) ;
#6417 = CARTESIAN_POINT ( 'NONE',  ( 805.9055244015594326, -363.6237781080502032, -315.8990559732753240 ) ) ;
#6418 = VECTOR ( 'NONE', #44154, 1000.000000000000000 ) ;
#6419 = CARTESIAN_POINT ( 'NONE',  ( 782.4968714119720516, -106.8164208402383935, -305.0891759886411023 ) ) ;
#6420 = CARTESIAN_POINT ( 'NONE',  ( 796.1575198192839480, -54.00906357242601530, 359.4546378042384163 ) ) ;
#6421 = CARTESIAN_POINT ( 'NONE',  ( 812.7932403749906598, -399.1800572038738437, -327.7687537140311633 ) ) ;
#6422 = DIRECTION ( 'NONE',  ( 0.000000000000000000, 0.000000000000000000, 1.000000000000000000 ) ) ;
#6423 = CARTESIAN_POINT ( 'NONE',  ( 803.2186876482843445, -415.9874144716862361, 350.0220218866286928 ) ) ;
#6424 = ORIENTED_EDGE ( 'NONE', *, *, #29246, .T. ) ;
#6425 = CARTESIAN_POINT ( 'NONE',  ( 762.1405469898971887, -265.5436935675106156, 357.8594530101015607 ) ) ;
#6426 = CIRCLE ( 'NONE', #36655, 2.749999999999835687 ) ;
#6427 = CARTESIAN_POINT ( 'NONE',  ( 800.1688906516307043, -154.1692326535053894, -369.0717654672308186 ) ) ;
#6428 = CARTESIAN_POINT ( 'NONE',  ( 919.9999999999993179, 154.9999999999998863, -360.0000000000000000 ) ) ;
#6429 = CARTESIAN_POINT ( 'NONE',  ( 813.9316612368132837, -271.4419599262321867, 348.6739635108323228 ) ) ;
#6430 = CARTESIAN_POINT ( 'NONE',  ( 788.7366044899766848, -107.9073299311474727, 316.5762568750059813 ) ) ;
#6431 = ORIENTED_EDGE ( 'NONE', *, *, #23149, .F. ) ;
#6432 = AXIS2_PLACEMENT_3D ( 'NONE', #1438, #19440, #12304 ) ;
#6433 = CARTESIAN_POINT ( 'NONE',  ( 801.3366627262608972, -8.532869017142163059, -353.0897708529566899 ) ) ;
#6434 = CARTESIAN_POINT ( 'NONE',  ( 795.1360043628807261, -284.0891481129650629, 360.2193346964456282 ) ) ;
#6435 = CARTESIAN_POINT ( 'NONE',  ( 754.9967657858570647, -1.543693567511449150, -365.0032342141425374 ) ) ;
#6436 = CARTESIAN_POINT ( 'NONE',  ( -78.83651009197140525, 260.0000000000000568, -199.9999999999936051 ) ) ;
#6437 = ORIENTED_EDGE ( 'NONE', *, *, #22489, .T. ) ;
#6438 = ORIENTED_EDGE ( 'NONE', *, *, #10590, .F. ) ;
#6439 = CARTESIAN_POINT ( 'NONE',  ( 755.8990559732751535, -419.4636090269702891, -365.9055244015606831 ) ) ;
#6440 = CARTESIAN_POINT ( 'NONE',  ( 804.6798772138708955, -255.7255117493287742, -334.6312213355107019 ) ) ;
#6442 = CARTESIAN_POINT ( 'NONE',  ( 814.8230680027162407, -269.8055962898686175, 333.7305795820267917 ) ) ;
#6441 = CARTESIAN_POINT ( 'NONE',  ( 814.5518280994195948, -351.7255117493284615, 332.4837098697145166 ) ) ;
#6443 = CARTESIAN_POINT ( 'NONE',  ( 769.0155153010367712, -250.3726999360618208, -362.7791456095907279 ) ) ;
#6444 = CARTESIAN_POINT ( 'NONE',  ( 800.0135310231082713, -254.0891481129652334, -325.0180583372163028 ) ) ;
#6445 = CARTESIAN_POINT ( 'NONE',  ( 756.5762568750052424, -435.1800572038737869, -348.7366044899774238 ) ) ;
#6446 = CARTESIAN_POINT ( 'NONE',  ( 801.9419747391806368, -90.45278447660209054, -351.9812246680014027 ) ) ;
#6447 = CARTESIAN_POINT ( 'NONE',  ( 755.3201227861273992, -243.7255117493287742, 345.3687786644892981 ) ) ;
#6448 = CIRCLE ( 'NONE', #33008, 10.00000000000000888 ) ;
#6449 = CARTESIAN_POINT ( 'NONE',  ( 787.4397851343537695, -357.7255117493285184, 374.2001403089903988 ) ) ;
#6450 = LINE ( 'NONE', #17537, #34376 ) ;
#6451 = CARTESIAN_POINT ( 'NONE',  ( 760.0363995740630116, -34.91815448151697154, -368.7758568127991907 ) ) ;
#6452 = DIRECTION ( 'NONE',  ( 0.000000000000000000, 0.000000000000000000, -1.000000000000000000 ) ) ;
#6453 = DIRECTION ( 'NONE',  ( -0.000000000000000000, -0.000000000000000000, 1.000000000000000000 ) ) ;
#6454 = CARTESIAN_POINT ( 'NONE',  ( 780.5236548040995785, -236.7363362996981380, 314.9735926884559944 ) ) ;
#6455 = CARTESIAN_POINT ( 'NONE',  ( 797.8594530101008786, -133.5436935675110135, 322.1405469898980982 ) ) ;
#6456 = EDGE_LOOP ( 'NONE', ( #37914, #41071, #7295, #41535 ) ) ;
#6457 = CARTESIAN_POINT ( 'NONE',  ( 804.6971507214547046, -3.281790845153435221, -344.0799538623459739 ) ) ;
#6458 = CARTESIAN_POINT ( 'NONE',  ( 792.2312462859673587, -83.90732993114754379, -307.2067596250082602 ) ) ;
#6459 = CARTESIAN_POINT ( 'NONE',  ( 755.0488828828309806, -281.8055962898686175, 344.1219089521771934 ) ) ;
#6460 = CONICAL_SURFACE ( 'NONE', #24882, 8.024999999999948841, 0.7853981633963380560 ) ;
#6461 = CARTESIAN_POINT ( 'NONE',  ( 792.1044303154645831, -420.4527844766009252, -317.8323909638837677 ) ) ;
#6462 = CARTESIAN_POINT ( 'NONE',  ( 800.2193346964446619, -42.99823902205676518, -355.1360043628816925 ) ) ;
#6463 = CARTESIAN_POINT ( 'NONE',  ( 795.1271208383656131, -452.8379544210779954, 371.6178728169206238 ) ) ;
#6464 = CARTESIAN_POINT ( 'NONE',  ( 814.9108240113580450, -184.2709662947835909, -337.5031285880265273 ) ) ;
#6465 = CARTESIAN_POINT ( 'NONE',  ( 800.9747183278959710, -84.99823902205663728, 311.9810565676471583 ) ) ;
#6466 = CARTESIAN_POINT ( 'NONE',  ( 787.4397851343537695, -165.7255117493291152, 374.2001403089903988 ) ) ;
#6467 = LINE ( 'NONE', #17307, #41700 ) ;
#6468 = CARTESIAN_POINT ( 'NONE',  ( -879.9999999999992042, 430.0000000000002842, -320.0000000000000568 ) ) ;
#6469 = CARTESIAN_POINT ( 'NONE',  ( 761.9338519418445230, -278.5328690171412518, -370.4231160770881957 ) ) ;
#6470 = CARTESIAN_POINT ( 'NONE',  ( 802.2119215644370342, -414.0090635724249637, 367.5423716828165084 ) ) ;
#6471 = CARTESIAN_POINT ( 'NONE',  ( 745.4481719005789273, -291.7255117493285752, -347.5162901302853129 ) ) ;
#6472 = CARTESIAN_POINT ( 'NONE',  ( 799.9999999999993179, -365.3551492539851893, 8.132432514707076621 ) ) ;
#6473 = CARTESIAN_POINT ( 'NONE',  ( 745.4481719005789273, -387.7255117493283478, 347.5162901302853129 ) ) ;
#6474 = CARTESIAN_POINT ( 'NONE',  ( 751.9810565676468741, -26.08914811296592262, 360.9747183278973921 ) ) ;
#6475 = CARTESIAN_POINT ( 'NONE',  ( 785.3687786644884454, -395.3618753856918602, -315.3201227861279676 ) ) ;
#6476 = CARTESIAN_POINT ( 'NONE',  ( 769.1273215169530886, -22.71468719896029853, 317.4527132478988847 ) ) ;
#6477 = CARTESIAN_POINT ( 'NONE',  ( 748.3538107759620743, -40.71468719896024879, -355.8262568251490165 ) ) ;
#6478 = CARTESIAN_POINT ( 'NONE',  ( 805.0264073115434940, -150.3510508353235480, -339.4763451958999099 ) ) ;
#6479 = CARTESIAN_POINT ( 'NONE',  ( 751.2241431872005251, -160.1692326535053326, 359.9636004259367610 ) ) ;
#6480 = DIRECTION ( 'NONE',  ( 0.000000000000000000, -1.000000000000000000, 0.000000000000000000 ) ) ;
#6481 = ORIENTED_EDGE ( 'NONE', *, *, #37385, .T. ) ;
#6482 = CARTESIAN_POINT ( 'NONE',  ( 785.3687786644884454, -59.36187538569306810, -315.3201227861279676 ) ) ;
#6483 = CARTESIAN_POINT ( 'NONE',  ( 790.8726784830453198, -178.7146871989598083, -362.5472867521010585 ) ) ;
#6484 = CARTESIAN_POINT ( 'NONE',  ( 759.7806653035534055, -150.9982390220563957, 324.8639956371180801 ) ) ;
#6485 = CARTESIAN_POINT ( 'NONE',  ( 768.8385539511368734, 0.7398582555850804487, -306.4236121716840557 ) ) ;
#6486 = CARTESIAN_POINT ( 'NONE',  ( 792.1044303154646968, -300.4527844766013231, 317.8323909638837677 ) ) ;
#6487 = CARTESIAN_POINT ( 'NONE',  ( 998.9999999999992042, 74.99999999999984368, -360.0000000000000000 ) ) ;
#6488 = VERTEX_POINT ( 'NONE', #28037 ) ;
#6489 = CARTESIAN_POINT ( 'NONE',  ( 764.0069404352550464, -15.07832356259669560, 359.2566176426627180 ) ) ;
#6490 = CARTESIAN_POINT ( 'NONE',  ( 745.5313806188320314, -303.2817908451525000, -333.7943932421247268 ) ) ;
#6491 = AXIS2_PLACEMENT_3D ( 'NONE', #40901, #32850, #9271 ) ;
#6492 = CARTESIAN_POINT ( 'NONE',  ( 777.5031285880264704, -238.8164208402379813, 374.9108240113588408 ) ) ;
#6493 = CARTESIAN_POINT ( 'NONE',  ( 757.0176451133909268, -325.0999726633342561, 349.9200121543848354 ) ) ;
#6494 = CARTESIAN_POINT ( 'NONE',  ( 761.2382568024794409, -423.6237781080499190, 356.9571628226838129 ) ) ;
#6495 = CARTESIAN_POINT ( 'NONE',  ( 804.1105419155481968, -147.8272453906075157, -347.6308680596136469 ) ) ;
#6496 = CARTESIAN_POINT ( 'NONE',  ( 755.5713283507202505, -125.3618753856928834, -334.6858677611754729 ) ) ;
#6497 = CARTESIAN_POINT ( 'NONE',  ( 788.8264449731201466, -309.1800572038740711, -363.6646147819170665 ) ) ;
#6498 = ORIENTED_EDGE ( 'NONE', *, *, #25485, .T. ) ;
#6499 = CARTESIAN_POINT ( 'NONE',  ( 755.8398074228967971, -331.4419599262320162, 333.4516893846970333 ) ) ;
#6500 = CARTESIAN_POINT ( 'NONE',  ( 791.6690787386836519, -454.6466601436378028, -367.6383479129825673 ) ) ;
#6501 = CARTESIAN_POINT ( 'NONE',  ( 805.2837595273609850, -122.7363362996985074, 340.5290396650784714 ) ) ;
#6502 = CARTESIAN_POINT ( 'NONE',  ( 758.0580252608178853, -6.452784476602343666, 328.0187753319985404 ) ) ;
#6503 = ORIENTED_EDGE ( 'NONE', *, *, #10845, .T. ) ;
#6504 = CARTESIAN_POINT ( 'NONE',  ( 755.8990559732751535, -371.4636090269705164, -365.9055244015606831 ) ) ;
#6505 = EDGE_CURVE ( 'NONE', #8476, #15857, #24555, .T. ) ;
#6506 = CARTESIAN_POINT ( 'NONE',  ( 571.1634899080285095, 259.9999999999999432, -199.9999999999981526 ) ) ;
#6507 = CARTESIAN_POINT ( 'NONE',  ( 786.5483106153019435, -223.6454272087891013, 364.1601925771022366 ) ) ;
#6508 = CARTESIAN_POINT ( 'NONE',  ( 813.5763878283155464, -243.8272453906072030, 351.1614460488615350 ) ) ;
#6509 = CARTESIAN_POINT ( 'NONE',  ( 803.2186876482843445, -175.9874144716871172, 350.0220218866286928 ) ) ;
#6510 = CARTESIAN_POINT ( 'NONE',  ( 754.8072714833581358, -340.8164208402376971, -338.1981804954720587 ) ) ;
#6511 = CARTESIAN_POINT ( 'NONE',  ( 759.0159684113467620, -184.9181544815165239, -325.8855110935213020 ) ) ;
#6512 = DIRECTION ( 'NONE',  ( 0.000000000000000000, 0.000000000000000000, 1.000000000000000000 ) ) ;
#6513 = CARTESIAN_POINT ( 'NONE',  ( 815.2698199232962679, -400.8164208402374697, -342.5225473063383674 ) ) ;
#6514 = FACE_OUTER_BOUND ( 'NONE', #17073, .T. ) ;
#6515 = AXIS2_PLACEMENT_3D ( 'NONE', #6852, #20257, #41983 ) ;
#6516 = CARTESIAN_POINT ( 'NONE',  ( 804.1009440267234822, -359.4636090269705164, 314.0944755984392600 ) ) ;
#6517 = CARTESIAN_POINT ( 'NONE',  ( 810.2700907235021077, -453.7763741861470521, -341.5253149289871999 ) ) ;
#6518 = CARTESIAN_POINT ( 'NONE',  ( 746.8695393053150156, -293.9073299311468759, 327.6429770376306010 ) ) ;
#6519 = CARTESIAN_POINT ( 'NONE',  ( 767.6429770376289525, -57.18005720387489532, -306.8695393053162093 ) ) ;
#6520 = CARTESIAN_POINT ( 'NONE',  ( 803.6646147819161570, -233.9073299311470180, -348.8264449731210561 ) ) ;
#6521 = DIRECTION ( 'NONE',  ( -0.000000000000000000, -0.000000000000000000, -1.000000000000000000 ) ) ;
#6522 = CARTESIAN_POINT ( 'NONE',  ( 803.4237431249931660, -399.1800572038738437, 331.2633955100225194 ) ) ;
#6523 = CARTESIAN_POINT ( 'NONE',  ( 769.0155153010367712, -154.3726999360620198, 362.7791456095907279 ) ) ;
#6524 = CARTESIAN_POINT ( 'NONE',  ( 757.2208543904082489, -40.71468719896024879, -350.9844846989624330 ) ) ;
#6525 = CARTESIAN_POINT ( 'NONE',  ( 808.7758568127978833, -76.16923265350557415, 320.0363995740631822 ) ) ;
#6526 = CARTESIAN_POINT ( 'NONE',  ( 788.8264449731201466, -381.1800572038739006, 363.6646147819170665 ) ) ;
#6527 = DIRECTION ( 'NONE',  ( 0.000000000000000000, 0.000000000000000000, 1.000000000000000000 ) ) ;
#6528 = CARTESIAN_POINT ( 'NONE',  ( 762.3223304703356007, -415.5436935675102177, 322.3223304703362828 ) ) ;
#6529 = EDGE_LOOP ( 'NONE', ( #14692, #21309 ) ) ;
#6530 = CARTESIAN_POINT ( 'NONE',  ( 756.5762568750052424, -51.18005720387493085, -348.7366044899774238 ) ) ;
#6531 = CARTESIAN_POINT ( 'NONE',  ( 803.2186876482843445, -367.9874144716865203, -350.0220218866286928 ) ) ;
#6533 = CARTESIAN_POINT ( 'NONE',  ( 778.1981804954715471, -178.2709662947835909, 314.8072714833591021 ) ) ;
#6532 = CARTESIAN_POINT ( 'NONE',  ( 759.9864689768902508, -194.0891481129654039, 354.9819416627836404 ) ) ;
#6534 = CARTESIAN_POINT ( 'NONE',  ( 805.9055244015594326, -363.6237781080502032, -315.8990559732753240 ) ) ;
#6535 = DIRECTION ( 'NONE',  ( 0.000000000000000000, 0.000000000000000000, 1.000000000000000000 ) ) ;
#6536 = VERTEX_POINT ( 'NONE', #41685 ) ;
#6537 = CARTESIAN_POINT ( 'NONE',  ( 785.3141322388236176, -405.7255117493283478, 364.4286716492789537 ) ) ;
#6538 = EDGE_LOOP ( 'NONE', ( #4300, #10500 ) ) ;
#6539 =( LENGTH_UNIT ( ) NAMED_UNIT ( * ) SI_UNIT ( .MILLI., .METRE. ) );
#6540 = CARTESIAN_POINT ( 'NONE',  ( 800.9747183278959710, -204.9982390220562820, -311.9810565676471583 ) ) ;
#6541 = CARTESIAN_POINT ( 'NONE',  ( 815.2698199232962679, -136.8164208402382656, 342.5225473063383674 ) ) ;
#6542 = ORIENTED_EDGE ( 'NONE', *, *, #40756, .F. ) ;
#6543 = CARTESIAN_POINT ( 'NONE',  ( 788.7366044899766848, -203.9073299311471885, -316.5762568750059813 ) ) ;
#6544 = EDGE_CURVE ( 'NONE', #22721, #820, #6790, .T. ) ;
#6545 = ORIENTED_EDGE ( 'NONE', *, *, #26084, .T. ) ;
#6546 = VECTOR ( 'NONE', #14134, 1000.000000000000000 ) ;
#6547 = CARTESIAN_POINT ( 'NONE',  ( 778.2165204200184689, -358.8164208402375834, -364.9363028652563230 ) ) ;
#6548 = CARTESIAN_POINT ( 'NONE',  ( 781.8018195045266339, 1.729033705215812011, -365.1927285166406705 ) ) ;
#6549 = CARTESIAN_POINT ( 'NONE',  ( 793.2243759319678702, -194.5328690171415644, 318.4439275373583200 ) ) ;
#6550 = DIRECTION ( 'NONE',  ( 0.000000000000000000, 0.000000000000000000, 1.000000000000000000 ) ) ;
#6551 = EDGE_CURVE ( 'NONE', #10806, #17231, #38671, .T. ) ;
#6552 = LINE ( 'NONE', #27801, #12513 ) ;
#6553 = ORIENTED_EDGE ( 'NONE', *, *, #11895, .T. ) ;
#6554 = CARTESIAN_POINT ( 'NONE',  ( 797.6776695296629214, 4.456306432488530866, -357.6776695296636603 ) ) ;
#6555 = PLANE ( 'NONE',  #17280 ) ;
#6556 = CARTESIAN_POINT ( 'NONE',  ( 831.1634899080286232, 258.0939999999998804, -199.9999999999999432 ) ) ;
#6557 = ORIENTED_EDGE ( 'NONE', *, *, #10256, .F. ) ;
#6558 = CARTESIAN_POINT ( 'NONE',  ( 773.7305795820266212, -225.2817908451527273, -374.8230680027170365 ) ) ;
#6559 = CARTESIAN_POINT ( 'NONE',  ( 814.8207195650702488, -122.1908817542439749, 336.2433038121456548 ) ) ;
#6561 = CARTESIAN_POINT ( 'NONE',  ( 759.7806653035534055, -222.9982390220561399, -324.8639956371180801 ) ) ;
#6560 = CARTESIAN_POINT ( 'NONE',  ( 914.9999999999992042, 99.99999999999984368, -350.0000000000000000 ) ) ;
#6562 = CARTESIAN_POINT ( 'NONE',  ( 766.7756240680305382, -398.5328690171409107, -361.5560724626415663 ) ) ;
#6563 = CARTESIAN_POINT ( 'NONE',  ( -208.8365100919714052, 260.0000000000001137, -199.9999999999926956 ) ) ;
#6564 = CARTESIAN_POINT ( 'NONE',  ( 778.1981804954715471, 13.72903370521577315, -314.8072714833591021 ) ) ;
#6565 = CARTESIAN_POINT ( 'NONE',  ( 798.5707757039680246, -77.46360902697138329, -356.7845633553585003 ) ) ;
#6566 = CARTESIAN_POINT ( 'NONE',  ( 814.4686193811664907, -387.2817908451522726, 346.2056067578752732 ) ) ;
#6567 = FACE_BOUND ( 'NONE', #38886, .T. ) ;
#6568 = CARTESIAN_POINT ( 'NONE',  ( 778.7502325331095108, 23.64894916467591912, -304.6391490659818828 ) ) ;
#6569 = CARTESIAN_POINT ( 'NONE',  ( 813.1304606946831655, -281.9073299311469327, -352.3570229623691716 ) ) ;
#6570 = CARTESIAN_POINT ( 'NONE',  ( -784.4999999999993179, -512.9681489794448908, -352.0000000000000000 ) ) ;
#6571 = CARTESIAN_POINT ( 'NONE',  ( 788.7366044899766848, -83.90732993114754379, -316.5762568750059813 ) ) ;
#6572 = CARTESIAN_POINT ( 'NONE',  ( 773.7305795820266212, -201.2817908451528126, 374.8230680027170365 ) ) ;
#6573 = CARTESIAN_POINT ( 'NONE',  ( 766.5853460496234675, -181.9874144716870887, -372.3518521366060554 ) ) ;
#6574 = CARTESIAN_POINT ( 'NONE',  ( 808.0189434323515343, -182.0891481129654323, 319.0252816721025511 ) ) ;
#6575 = CARTESIAN_POINT ( 'NONE',  ( 782.4968714119720516, -394.8164208402374697, -305.0891759886411023 ) ) ;
#6576 = CARTESIAN_POINT ( 'NONE',  ( -592.7175100919715760, 256.5000000000001705, -199.9999999999899671 ) ) ;
#6577 = EDGE_CURVE ( 'NONE', #20722, #29177, #35600, .T. ) ;
#6578 = CARTESIAN_POINT ( 'NONE',  ( 800.2193346964447755, -282.9982390220558841, 355.1360043628815788 ) ) ;
#6579 = CARTESIAN_POINT ( 'NONE',  ( 757.4527132478984868, -64.37269993606231822, 329.1273215169538844 ) ) ;
#6580 = CARTESIAN_POINT ( 'NONE',  ( 762.3223304703356007, -415.5436935675102177, -322.3223304703362828 ) ) ;
#6581 = VECTOR ( 'NONE', #18741, 1000.000000000000000 ) ;
#6582 = CARTESIAN_POINT ( 'NONE',  ( -858.8365100919713768, 256.5000000000002274, -202.7499999999880913 ) ) ;
#6583 = FACE_OUTER_BOUND ( 'NONE', #27409, .T. ) ;
#6585 = CARTESIAN_POINT ( 'NONE',  ( 788.8264449731200330, -333.1800572038740142, 363.6646147819171233 ) ) ;
#6584 = CARTESIAN_POINT ( 'NONE',  ( 780.5290396650775619, -132.3510508353235764, 365.2837595273619513 ) ) ;
#6586 = EDGE_LOOP ( 'NONE', ( #9517, #24298, #13776, #21381 ) ) ;
#6587 = CARTESIAN_POINT ( 'NONE',  ( 804.1601925771018387, -247.4419599262323004, -346.5483106153029098 ) ) ;
#6588 = CARTESIAN_POINT ( 'NONE',  ( 758.0580252608178853, -102.4527844766020337, 328.0187753319985404 ) ) ;
#6589 = CARTESIAN_POINT ( 'NONE',  ( 813.9316612368132837, -271.4419599262321867, -348.6739635108323228 ) ) ;
#6590 = DIRECTION ( 'NONE',  ( -0.000000000000000000, -1.000000000000000000, -0.000000000000000000 ) ) ;
#6591 = CARTESIAN_POINT ( 'NONE',  ( 747.3154664389472828, -403.9874144716863498, 326.4474001241230781 ) ) ;
#6592 = ORIENTED_EDGE ( 'NONE', *, *, #10942, .F. ) ;
#6593 = CARTESIAN_POINT ( 'NONE',  ( 774.6858677611749044, -297.7255117493286889, 315.5713283507209894 ) ) ;
#6594 = CARTESIAN_POINT ( 'NONE',  ( 779.4709603349208464, -48.35105083532386061, -314.7162404726379918 ) ) ;
#6595 = CARTESIAN_POINT ( 'NONE',  ( 767.8955696845333705, -168.4527844766018347, -362.1676090361162323 ) ) ;
#6596 = CARTESIAN_POINT ( 'NONE',  ( 757.8323909638827445, -194.6346026584198796, -352.1044303154654358 ) ) ;
#6597 = CARTESIAN_POINT ( 'NONE',  ( 792.1044303154645831, -420.4527844766009252, 317.8323909638837677 ) ) ;
#6598 = ADVANCED_FACE ( 'NONE', ( #16746, #9803 ), #20867, .F. ) ;
#6599 = CARTESIAN_POINT ( 'NONE',  ( 744.7301800767019131, -124.8164208402383508, -337.4774526936615757 ) ) ;
#6600 = CARTESIAN_POINT ( 'NONE',  ( 762.1405469898973024, -121.5436935675110561, -357.8594530101016176 ) ) ;
#6601 = ORIENTED_EDGE ( 'NONE', *, *, #39633, .T. ) ;
#6602 = CARTESIAN_POINT ( 'NONE',  ( 755.5913626894240451, -61.64542720878961291, -346.6156483768012890 ) ) ;
#6603 = CARTESIAN_POINT ( 'NONE',  ( 790.0220218866281812, -391.0999726633340288, -363.2186876482849129 ) ) ;
#6605 = CARTESIAN_POINT ( 'NONE',  ( 793.9708237608222134, -454.9181544815156713, 319.2295555964448681 ) ) ;
#6604 = CARTESIAN_POINT ( 'NONE',  ( 768.0187753319979720, -128.6346026584201354, 318.0580252608186242 ) ) ;
#6606 = CARTESIAN_POINT ( 'NONE',  ( 796.7845633553578182, -105.6237781080509421, 358.5707757039688204 ) ) ;
#6607 = EDGE_CURVE ( 'NONE', #19810, #3171, #35887, .T. ) ;
#6610 = CARTESIAN_POINT ( 'NONE',  ( 766.5853460496234675, -373.9874144716864066, 372.3518521366060554 ) ) ;
#6609 = DIRECTION ( 'NONE',  ( -0.000000000000000000, -1.000000000000000000, 0.000000000000000000 ) ) ;
#6608 = CARTESIAN_POINT ( 'NONE',  ( 879.9999999999992042, 99.99999999999984368, -350.0000000000000000 ) ) ;
#6611 = EDGE_CURVE ( 'NONE', #14349, #38546, #21561, .T. ) ;
#6612 = EDGE_LOOP ( 'NONE', ( #15855, #29638, #34728, #12062 ) ) ;
#6613 = CARTESIAN_POINT ( 'NONE',  ( 755.5913626894240451, -349.6454272087887603, -346.6156483768012890 ) ) ;
#6614 = CARTESIAN_POINT ( 'NONE',  ( 755.5713283507202505, -341.3618753856922012, -334.6858677611754729 ) ) ;
#6615 = CARTESIAN_POINT ( 'NONE',  ( 745.1792804349281596, -134.1908817542439181, -343.7566961878542884 ) ) ;
#6616 = VECTOR ( 'NONE', #38203, 1000.000000000000000 ) ;
#6617 = CARTESIAN_POINT ( 'NONE',  ( 814.4686193811664907, -27.28179084515336328, 346.2056067578752732 ) ) ;
#6619 = DIRECTION ( 'NONE',  ( 0.000000000000000000, -1.000000000000000000, 0.000000000000000000 ) ) ;
#6618 = DIRECTION ( 'NONE',  ( 1.000000000000000000, -0.000000000000000000, -0.000000000000000000 ) ) ;
#6620 = CARTESIAN_POINT ( 'NONE',  ( 766.7756240680305382, -278.5328690171412518, -361.5560724626415663 ) ) ;
#6621 = CARTESIAN_POINT ( 'NONE',  ( 783.7953271457878373, -152.1908817542438612, -375.1787889125761239 ) ) ;
#6622 = CARTESIAN_POINT ( 'NONE',  ( 989.9999999999992042, 62.79977829742938411, -207.3621835540872951 ) ) ;
#6623 = CARTESIAN_POINT ( 'NONE',  ( 190.7583438952258916, 294.6698570112193920, -244.9999999999999716 ) ) ;
#6624 = CARTESIAN_POINT ( 'NONE',  ( 758.4439275373578084, -348.5545181178796383, 353.2243759319684386 ) ) ;
#6625 = CARTESIAN_POINT ( 'NONE',  ( 752.7379699480933368, -300.0090635724252479, 361.9858362298580232 ) ) ;
#6626 = CARTESIAN_POINT ( 'NONE',  ( 745.4481719005789273, -171.7255117493290868, -347.5162901302853697 ) ) ;
#6627 = ADVANCED_FACE ( 'NONE', ( #35644, #558 ), #40036, .F. ) ;
#6628 = PLANE ( 'NONE',  #2503 ) ;
#6629 = CARTESIAN_POINT ( 'NONE',  ( 804.1009440267234822, -95.46360902697132644, 314.0944755984392600 ) ) ;
#6630 = ADVANCED_FACE ( 'NONE', ( #25717 ), #15099, .T. ) ;
#6631 = CARTESIAN_POINT ( 'NONE',  ( 759.0252816721024374, -288.9982390220559978, -368.0189434323527280 ) ) ;
#6632 = DIRECTION ( 'NONE',  ( -1.000000000000000000, -0.000000000000000000, 0.000000000000000000 ) ) ;
#6633 = DIRECTION ( 'NONE',  ( 0.000000000000000000, 0.3826834323650838421, 0.9238795325112891810 ) ) ;
#6634 = CARTESIAN_POINT ( 'NONE',  ( 755.3201227861273992, -171.7255117493291152, 345.3687786644892981 ) ) ;
#6635 = ORIENTED_EDGE ( 'NONE', *, *, #30587, .T. ) ;
#6636 = CARTESIAN_POINT ( 'NONE',  ( 783.7953271457878373, -416.1908817542430938, 375.1787889125761239 ) ) ;
#6637 = CARTESIAN_POINT ( 'NONE',  ( 815.0009284576459549, -366.3510508353228374, -338.7629533639073429 ) ) ;
#6638 = CARTESIAN_POINT ( 'NONE',  ( 810.7187646348534145, -138.4527844766019200, -356.7737145352016341 ) ) ;
#6639 = CARTESIAN_POINT ( 'NONE',  ( 761.4292242960306112, -65.46360902697142592, 323.2154366446414429 ) ) ;
#6640 = CARTESIAN_POINT ( 'NONE',  ( 749.2812353651451076, -390.4527844766011526, -323.2262854647983090 ) ) ;
#6641 = DIRECTION ( 'NONE',  ( 0.000000000000000000, 0.000000000000000000, -1.000000000000000000 ) ) ;
#6642 = CARTESIAN_POINT ( 'NONE',  ( 768.8385539511368734, 0.7398582555850804487, 306.4236121716840557 ) ) ;
#6643 = EDGE_LOOP ( 'NONE', ( #35857, #18885, #44425, #10145 ) ) ;
#6644 = CARTESIAN_POINT ( 'NONE',  ( 768.8385539511368734, -143.2601417444144829, -306.4236121716840557 ) ) ;
#6645 = CARTESIAN_POINT ( 'NONE',  ( 799.9999999999993179, -373.0259173205825505, -36.60293108048681887 ) ) ;
#6646 = CARTESIAN_POINT ( 'NONE',  ( 759.8311093483677041, -262.1692326535049347, 310.9282345327691814 ) ) ;
#6647 = CARTESIAN_POINT ( 'NONE',  ( 764.8639956371174549, -104.0891481129656739, 319.7806653035542581 ) ) ;
#6648 = EDGE_LOOP ( 'NONE', ( #32461, #24761, #13432, #33753 ) ) ;
#6649 = EDGE_CURVE ( 'NONE', #20679, #40483, #8392, .T. ) ;
#6650 = CARTESIAN_POINT ( 'NONE',  ( 755.5713283507202505, -293.3618753856923718, 334.6858677611754729 ) ) ;
#6651 = EDGE_CURVE ( 'NONE', #40320, #16409, #18353, .T. ) ;
#6652 = CARTESIAN_POINT ( 'NONE',  ( 814.2001403089898304, -17.36187538569322086, -347.4397851343538264 ) ) ;
#6653 = FACE_OUTER_BOUND ( 'NONE', #30548, .T. ) ;
#6654 = ORIENTED_EDGE ( 'NONE', *, *, #11087, .F. ) ;
#6655 = CARTESIAN_POINT ( 'NONE',  ( 746.4236121716829757, -423.8272453906067199, -328.8385539511384650 ) ) ;
#6656 = CARTESIAN_POINT ( 'NONE',  ( 800.2193346964447755, -18.99823902205683979, 355.1360043628815788 ) ) ;
#6657 = CARTESIAN_POINT ( 'NONE',  ( 759.7806653035534055, -270.9982390220561115, -324.8639956371180801 ) ) ;
#6658 = EDGE_CURVE ( 'NONE', #34587, #37957, #36334, .T. ) ;
#6660 = CARTESIAN_POINT ( 'NONE',  ( 803.8556311672234642, -249.6237781080505158, 365.6418435158340117 ) ) ;
#6659 = CARTESIAN_POINT ( 'NONE',  ( 746.8695393053151292, -365.9073299311466485, 327.6429770376306578 ) ) ;
#6661 = EDGE_CURVE ( 'NONE', #28937, #40519, #32165, .T. ) ;
#6662 = CARTESIAN_POINT ( 'NONE',  ( 801.5560724626406000, -240.5545181178798941, -326.7756240680316182 ) ) ;
#6663 = CARTESIAN_POINT ( 'NONE',  ( 797.8594530101008786, -253.5436935675104735, -322.1405469898980982 ) ) ;
#6664 = CARTESIAN_POINT ( 'NONE',  ( 779.9999999999992042, -452.9681489794448339, -309.9999999999998863 ) ) ;
#6665 = CARTESIAN_POINT ( 'NONE',  ( 791.9812246680005501, -92.63460265842026331, -361.9419747391813189 ) ) ;
#6666 = CARTESIAN_POINT ( 'NONE',  ( 802.1676090361156639, -230.6346026584197659, 327.8955696845344505 ) ) ;
#6667 = CARTESIAN_POINT ( 'NONE',  ( 763.0537975583475827, -360.4527844766010958, 371.0346526505627480 ) ) ;
#6668 = DIRECTION ( 'NONE',  ( -1.000000000000000000, -0.000000000000000000, -0.000000000000000000 ) ) ;
#6669 = CARTESIAN_POINT ( 'NONE',  ( 810.4231160770870019, -48.55451811788057626, -321.9338519418446936 ) ) ;
#6670 = CARTESIAN_POINT ( 'NONE',  ( 786.4999999999993179, -563.3203001761230553, -342.3463313526983143 ) ) ;
#6671 = CARTESIAN_POINT ( 'NONE',  ( 928.0249999999991815, 154.9999999999998863, 360.0000000000000000 ) ) ;
#6672 = CARTESIAN_POINT ( 'NONE',  ( 760.7433823573367135, -228.0090635724254753, 355.9930595647440441 ) ) ;
#6673 = CARTESIAN_POINT ( 'NONE',  ( 788.7366044899766848, -131.9073299311473875, 316.5762568750059813 ) ) ;
#6674 = EDGE_LOOP ( 'NONE', ( #23150, #24484, #26874, #15076 ) ) ;
#6675 = CARTESIAN_POINT ( 'NONE',  ( 804.8461984189677878, -26.19088175424427334, -336.9566956441385628 ) ) ;
#6676 = CARTESIAN_POINT ( 'NONE',  ( 755.2512626584698410, -55.54369356751127640, -315.2512626584710915 ) ) ;
#6677 = CARTESIAN_POINT ( 'NONE',  ( 784.0799538623451781, -275.8055962898685038, 364.6971507214555572 ) ) ;
#6678 = CARTESIAN_POINT ( 'NONE',  ( 781.7834795799800531, -442.8164208402372992, -315.0636971347436202 ) ) ;
#6679 = CARTESIAN_POINT ( 'NONE',  ( 755.5713283507202505, -53.36187538569310362, -334.6858677611754729 ) ) ;
#6680 = CARTESIAN_POINT ( 'NONE',  ( 749.5768839229115201, -12.55451811788067751, 358.0661480581553064 ) ) ;
#6681 = CARTESIAN_POINT ( 'NONE',  ( 808.0189434323515343, -206.0891481129653471, -319.0252816721025511 ) ) ;
#6682 = CARTESIAN_POINT ( 'NONE',  ( 800.9747183278959710, -180.9982390220563389, 311.9810565676471583 ) ) ;
#6683 = CARTESIAN_POINT ( 'NONE',  ( 795.1360043628807261, -92.08914811296568814, 360.2193346964456282 ) ) ;
#6684 = CARTESIAN_POINT ( 'NONE',  ( 784.9999999999992042, 240.0000000000000853, -275.0000000000000000 ) ) ;
#6685 = DIRECTION ( 'NONE',  ( 0.000000000000000000, -0.000000000000000000, 1.000000000000000000 ) ) ;
#6686 = CARTESIAN_POINT ( 'NONE',  ( 752.4576283171824116, -285.0783235625958127, -317.7880784355627952 ) ) ;
#6687 = CARTESIAN_POINT ( 'NONE',  ( 814.8207195650702488, -434.1908817542430370, 336.2433038121456548 ) ) ;
#6688 = CARTESIAN_POINT ( 'NONE',  ( 796.7737145352015204, -284.6346026584196807, -370.7187646348536987 ) ) ;
#6689 = CARTESIAN_POINT ( 'NONE',  ( -115.7583438952258774, 430.0000000000002842, -244.9999999999999716 ) ) ;
#6690 = CARTESIAN_POINT ( 'NONE',  ( 751.6929314249748586, -390.9982390220557136, 318.8095938919659034 ) ) ;
#6691 = CARTESIAN_POINT ( 'NONE',  ( 813.1304606946831655, -41.90732993114767879, 352.3570229623691716 ) ) ;
#6692 = CARTESIAN_POINT ( 'NONE',  ( 803.6646147819161570, -401.9073299311463643, -348.8264449731210561 ) ) ;
#6693 = CARTESIAN_POINT ( 'NONE',  ( 754.9735926884551418, -18.35105083532395298, 340.5236548041000333 ) ) ;
#6694 = CARTESIAN_POINT ( 'NONE',  ( 803.8556311672234642, -57.62377810805111267, -365.6418435158340117 ) ) ;
#6695 = CARTESIAN_POINT ( 'NONE',  ( 769.1273215169530886, -190.7146871989597798, -317.4527132478988847 ) ) ;
#6696 = CARTESIAN_POINT ( 'NONE',  ( 801.9858362298568863, -171.0783235625962106, 312.7379699480935642 ) ) ;
#6697 = CARTESIAN_POINT ( 'NONE',  ( 764.8639956371174549, -8.089148112965974136, 319.7806653035542581 ) ) ;
#6698 = ADVANCED_FACE ( 'NONE', ( #22461 ), #26260, .F. ) ;
#6699 = EDGE_LOOP ( 'NONE', ( #39109, #2326, #14048, #42847 ) ) ;
#6700 = CARTESIAN_POINT ( 'NONE',  ( 781.7834795799800531, -58.81642084023854267, -315.0636971347436202 ) ) ;
#6701 = CARTESIAN_POINT ( 'NONE',  ( 804.1601925771018387, -199.4419599262324709, -346.5483106153029098 ) ) ;
#6702 = UNCERTAINTY_MEASURE_WITH_UNIT (LENGTH_MEASURE( 1.000000000000000082E-05 ), #15190, 'distance_accuracy_value', 'NONE');
#6703 = CARTESIAN_POINT ( 'NONE',  ( 756.5762568750052424, -171.1800572038745543, 348.7366044899774238 ) ) ;
#6704 = CARTESIAN_POINT ( 'NONE',  ( 803.8556311672234642, 14.37622189194867417, -365.6418435158340117 ) ) ;
#6705 = CARTESIAN_POINT ( 'NONE',  ( 774.6858677611749044, -345.7255117493285184, 315.5713283507209894 ) ) ;
#6706 = CYLINDRICAL_SURFACE ( 'NONE', #3569, 6.118999999999985562 ) ;
#6707 = ORIENTED_EDGE ( 'NONE', *, *, #37624, .T. ) ;
#6708 = CARTESIAN_POINT ( 'NONE',  ( 786.6156483768007774, -1.441959926233096656, 315.5913626894246136 ) ) ;
#6709 = CARTESIAN_POINT ( 'NONE',  ( 791.0478386215596629, -309.8272453906070041, -306.7653713866226326 ) ) ;
#6710 = CARTESIAN_POINT ( 'NONE',  ( 787.5162901302840055, -251.3618753856923718, 305.4481719005793252 ) ) ;
#6711 = CARTESIAN_POINT ( 'NONE',  ( 769.0155153010367712, -346.3726999360614514, 362.7791456095907279 ) ) ;
#6712 = CARTESIAN_POINT ( 'NONE',  ( 764.0069404352550464, -423.0783235625953580, 359.2566176426627180 ) ) ;
#6713 = CARTESIAN_POINT ( 'NONE',  ( 793.9708237608222134, -142.9181544815166376, -319.2295555964448681 ) ) ;
#6714 = CARTESIAN_POINT ( 'NONE',  ( 778.2165204200184689, -142.8164208402382656, -364.9363028652563230 ) ) ;
#6715 = CIRCLE ( 'NONE', #18541, 2.749999999999919176 ) ;
#6716 = CARTESIAN_POINT ( 'NONE',  ( 768.0187753319979720, -320.6346026584195670, -318.0580252608186242 ) ) ;
#6717 = ORIENTED_EDGE ( 'NONE', *, *, #30074, .T. ) ;
#6718 = CARTESIAN_POINT ( 'NONE',  ( 804.6798772138708955, -447.7255117493280636, -334.6312213355107019 ) ) ;
#6719 = CARTESIAN_POINT ( 'NONE',  ( 756.7813123517142913, -331.9874144716865203, 329.9779781133712504 ) ) ;
#6720 = CARTESIAN_POINT ( 'NONE',  ( 998.9999999999992042, 249.9999999999998863, -199.9999999999999716 ) ) ;
#6721 = CARTESIAN_POINT ( 'NONE',  ( 755.3028492785439312, -111.2817908451530968, 335.9200461376539693 ) ) ;
#6722 = CARTESIAN_POINT ( 'NONE',  ( 754.8072714833581358, -4.816420840238714085, 338.1981804954720587 ) ) ;
#6723 = ORIENTED_EDGE ( 'NONE', *, *, #39390, .T. ) ;
#6724 = CARTESIAN_POINT ( 'NONE',  ( 797.8822607201568644, -366.5545181178795815, -370.1134526219340160 ) ) ;
#6725 = DIRECTION ( 'NONE',  ( -0.000000000000000000, -0.000000000000000000, 1.000000000000000000 ) ) ;
#6726 = CARTESIAN_POINT ( 'NONE',  ( 769.0155153010367712, -226.3726999360617924, 362.7791456095907279 ) ) ;
#6727 = CARTESIAN_POINT ( 'NONE',  ( 797.8822607201568644, -222.5545181178800362, 370.1134526219340160 ) ) ;
#6728 = CARTESIAN_POINT ( 'NONE',  ( 773.3843516231979720, -181.4419599262325278, 364.4086373105754433 ) ) ;
#6729 = CARTESIAN_POINT ( 'NONE',  ( 804.9363028652555840, -328.2709662947831362, -338.2165204200192079 ) ) ;
#6730 = DIRECTION ( 'NONE',  ( 1.000000000000000000, -0.000000000000000000, -0.000000000000000000 ) ) ;
#6731 = CARTESIAN_POINT ( 'NONE',  ( 759.0159684113467620, -208.9181544815164102, -325.8855110935213020 ) ) ;
#6732 = CARTESIAN_POINT ( 'NONE',  ( 782.5225473063381969, -22.27096629478410250, 375.2698199232970637 ) ) ;
#6733 = CARTESIAN_POINT ( 'NONE',  ( 772.4837098697144029, -71.36187538569302546, 374.5518280994205611 ) ) ;
#6734 = CARTESIAN_POINT ( 'NONE',  ( 792.6815175455323015, -452.9681489794447202, 361.6124358662449367 ) ) ;
#6735 = CARTESIAN_POINT ( 'NONE',  ( 814.2001403089898304, -425.3618753856919170, -347.4397851343538264 ) ) ;
#6736 = DIRECTION ( 'NONE',  ( 1.000000000000000000, 0.000000000000000000, 0.000000000000000000 ) ) ;
#6737 = CARTESIAN_POINT ( 'NONE',  ( 778.7629533639073998, -368.7363362996977685, 375.0009284576466371 ) ) ;
#6738 = DIRECTION ( 'NONE',  ( 0.000000000000000000, 0.000000000000000000, 1.000000000000000000 ) ) ;
#6739 = CARTESIAN_POINT ( 'NONE',  ( 810.7187646348534145, -282.4527844766014937, 356.7737145352016341 ) ) ;
#6740 = CARTESIAN_POINT ( 'NONE',  ( 801.1904061080336987, -68.08914811296575920, -368.3070685750235498 ) ) ;
#6741 = CARTESIAN_POINT ( 'NONE',  ( 785.3141322388236176, -285.7255117493286889, -364.4286716492789537 ) ) ;
#6742 = DIRECTION ( 'NONE',  ( -0.000000000000000000, 1.000000000000000000, -0.000000000000000000 ) ) ;
#6743 = CARTESIAN_POINT ( 'NONE',  ( 759.9864689768902508, -386.0891481129647786, 354.9819416627836404 ) ) ;
#6744 = VECTOR ( 'NONE', #39080, 1000.000000000000000 ) ;
#6745 = CARTESIAN_POINT ( 'NONE',  ( 786.5483106153019435, -151.6454272087892718, 364.1601925771022366 ) ) ;
#6746 = CARTESIAN_POINT ( 'NONE',  ( 810.4231160770870019, -24.55451811788064020, -321.9338519418446936 ) ) ;
#6747 = CARTESIAN_POINT ( 'NONE',  ( 784.0799538623451781, -35.80559628986934229, -364.6971507214555572 ) ) ;
#6748 = CARTESIAN_POINT ( 'NONE',  ( 746.0683387631852383, -67.44195992623289726, 331.3260364891676204 ) ) ;
#6749 = CARTESIAN_POINT ( 'NONE',  ( 778.1981804954715471, -394.2709662947829088, 314.8072714833591021 ) ) ;
#6750 = CARTESIAN_POINT ( 'NONE',  ( 796.9462024416508257, 11.54721552339759860, 308.9653473494370246 ) ) ;
#6751 = DIRECTION ( 'NONE',  ( 0.000000000000000000, 0.000000000000000000, 1.000000000000000000 ) ) ;
#6752 = CARTESIAN_POINT ( 'NONE',  ( 759.8311093483677041, -142.1692326535054178, 310.9282345327691814 ) ) ;
#6753 = CARTESIAN_POINT ( 'NONE',  ( 759.7806653035534055, -414.9982390220555430, 324.8639956371180801 ) ) ;
#6755 = ORIENTED_EDGE ( 'NONE', *, *, #8285, .F. ) ;
#6754 = CARTESIAN_POINT ( 'NONE',  ( 766.7756240680305382, -110.5328690171418629, -361.5560724626415663 ) ) ;
#6756 = CARTESIAN_POINT ( 'NONE',  ( 778.2165204200184689, -46.81642084023858530, -364.9363028652563230 ) ) ;
#6757 = CARTESIAN_POINT ( 'NONE',  ( 795.9930595647434757, -363.0783235625955854, -320.7433823573372820 ) ) ;
#6759 = CARTESIAN_POINT ( 'NONE',  ( 794.9819416627830151, -180.9982390220563389, 319.9864689768909898 ) ) ;
#6758 = CARTESIAN_POINT ( 'NONE',  ( 781.7834795799800531, -226.8164208402380098, 315.0636971347436202 ) ) ;
#6760 = EDGE_LOOP ( 'NONE', ( #26798, #39176 ) ) ;
#6761 = CARTESIAN_POINT ( 'NONE',  ( 801.9858362298568863, -387.0783235625955285, -312.7379699480935642 ) ) ;
#6762 = DIRECTION ( 'NONE',  ( -0.000000000000000000, 1.000000000000000000, -0.000000000000000000 ) ) ;
#6763 = VERTEX_POINT ( 'NONE', #28960 ) ;
#6764 = CARTESIAN_POINT ( 'NONE',  ( 767.8955696845333705, -408.4527844766009252, 362.1676090361162323 ) ) ;
#6765 = ORIENTED_EDGE ( 'NONE', *, *, #41342, .T. ) ;
#6766 = CARTESIAN_POINT ( 'NONE',  ( 814.9108240113580450, -208.2709662947835341, -337.5031285880265273 ) ) ;
#6767 = CARTESIAN_POINT ( 'NONE',  ( 805.0032342141413437, -157.5436935675109282, 314.9967657858572352 ) ) ;
#6768 = ORIENTED_EDGE ( 'NONE', *, *, #42448, .T. ) ;
#6769 = CARTESIAN_POINT ( 'NONE',  ( 794.9819416627830151, -228.9982390220561683, -319.9864689768909898 ) ) ;
#6770 = ORIENTED_EDGE ( 'NONE', *, *, #17975, .F. ) ;
#6771 = CARTESIAN_POINT ( 'NONE',  ( 800.0135310231082713, -350.0891481129648923, -325.0180583372163028 ) ) ;
#6772 = CARTESIAN_POINT ( 'NONE',  ( 771.1735550268778070, -9.180057203875058747, -316.3353852180827630 ) ) ;
#6773 = CARTESIAN_POINT ( 'NONE',  ( 801.3366627262608972, -224.5328690171415076, 353.0897708529566899 ) ) ;
#6774 = CARTESIAN_POINT ( 'NONE',  ( 784.4999999999993179, -513.1383975375929367, -367.9999999999999432 ) ) ;
#6775 = DIRECTION ( 'NONE',  ( -0.000000000000000000, 1.000000000000000000, -0.000000000000000000 ) ) ;
#6776 = VERTEX_POINT ( 'NONE', #31948 ) ;
#6777 = CARTESIAN_POINT ( 'NONE',  ( 804.6798772138708955, 8.274488250670337663, -334.6312213355107019 ) ) ;
#6778 = DIRECTION ( 'NONE',  ( 1.000000000000000000, 0.000000000000000000, 0.000000000000000000 ) ) ;
#6779 = CARTESIAN_POINT ( 'NONE',  ( 759.9999999999992042, -512.9681489794448908, 339.9999999999999432 ) ) ;
#6780 = CARTESIAN_POINT ( 'NONE',  ( 764.1737431748507561, -274.3726999360617356, -371.6461892240376415 ) ) ;
#6781 = VECTOR ( 'NONE', #11345, 1000.000000000000114 ) ;
#6782 = CARTESIAN_POINT ( 'NONE',  ( 807.2620300519052989, -144.0090635724257027, 318.0141637701419768 ) ) ;
#6784 = CARTESIAN_POINT ( 'NONE',  ( 804.4286716492782716, -233.3618753856925423, -345.3141322388244703 ) ) ;
#6783 = DIRECTION ( 'NONE',  ( -0.000000000000000000, 1.000000000000000000, -0.000000000000000000 ) ) ;
#6785 = CARTESIAN_POINT ( 'NONE',  ( 757.2208543904082489, -400.7146871989590977, -350.9844846989624330 ) ) ;
#6786 = DIRECTION ( 'NONE',  ( -0.000000000000000000, 1.000000000000000000, -0.000000000000000000 ) ) ;
#6787 = DIRECTION ( 'NONE',  ( -1.000000000000000000, -0.000000000000000000, -0.000000000000000000 ) ) ;
#6788 = CARTESIAN_POINT ( 'NONE',  ( 784.1219089521767955, -117.2817908451530684, -315.0488828828318333 ) ) ;
#6789 = CARTESIAN_POINT ( 'NONE',  ( 747.6481478633932056, -373.0999726633340856, 353.4146539503763620 ) ) ;
#6790 = LINE ( 'NONE', #24800, #28360 ) ;
#6791 = CARTESIAN_POINT ( 'NONE',  ( 790.8726784830453198, -442.7146871989589840, -362.5472867521010585 ) ) ;
#6792 = CARTESIAN_POINT ( 'NONE',  ( 763.2262854647970016, -320.6346026584195670, -309.2812353651462445 ) ) ;
#6793 = SURFACE_STYLE_FILL_AREA ( #21119 ) ;
#6794 = CARTESIAN_POINT ( 'NONE',  ( 762.3223304703356007, 16.45630643248849267, 322.3223304703362828 ) ) ;
#6795 = CARTESIAN_POINT ( 'NONE',  ( 797.6776695296629214, -67.54369356751125508, -357.6776695296636603 ) ) ;
#6796 = CARTESIAN_POINT ( 'NONE',  ( 814.8207195650702488, -242.1908817542435770, 336.2433038121456548 ) ) ;
#6797 = CARTESIAN_POINT ( 'NONE',  ( 781.2497674668890113, -204.3510508353233774, -375.3608509340180603 ) ) ;
#6798 = CARTESIAN_POINT ( 'NONE',  ( 772.5602148656447525, -177.7255117493290868, 305.7998596910095443 ) ) ;
#6799 = CARTESIAN_POINT ( 'NONE',  ( 745.0891759886404770, -436.2709662947827951, -342.4968714119734159 ) ) ;
#6800 = DIRECTION ( 'NONE',  ( 1.000000000000000000, 0.000000000000000000, -0.000000000000000000 ) ) ;
#6801 = CARTESIAN_POINT ( 'NONE',  ( 801.9419747391806368, -282.4527844766014937, 351.9812246680014027 ) ) ;
#6802 = CARTESIAN_POINT ( 'NONE',  ( 754.7162404726377645, -86.73633629969862113, 339.4709603349214717 ) ) ;
#6803 = CARTESIAN_POINT ( 'NONE',  ( 803.4237431249931660, -423.1800572038737300, -331.2633955100225194 ) ) ;
#6804 = CARTESIAN_POINT ( 'NONE',  ( -789.9999999999992042, 205.0000000000000568, -319.9999999999999432 ) ) ;
#6805 = CARTESIAN_POINT ( 'NONE',  ( 787.4999999999992042, -462.9681489794448339, 370.0000000000000568 ) ) ;
#6807 = CARTESIAN_POINT ( 'NONE',  ( 781.8018195045266339, -334.2709662947829656, 365.1927285166406705 ) ) ;
#6806 = CARTESIAN_POINT ( 'NONE',  ( 763.2154366446407039, -117.6237781080509279, 321.4292242960311228 ) ) ;
#6808 = VERTEX_POINT ( 'NONE', #39829 ) ;
#6809 = CARTESIAN_POINT ( 'NONE',  ( 789.9200121543843807, -265.9874144716867477, -317.0176451133914384 ) ) ;
#6810 = CARTESIAN_POINT ( 'NONE',  ( 759.7806653035534055, -102.9982390220565520, 324.8639956371180801 ) ) ;
#6811 = VECTOR ( 'NONE', #40991, 1000.000000000000000 ) ;
#6812 = CARTESIAN_POINT ( 'NONE',  ( 766.5853460496234675, -277.9874144716867477, -372.3518521366060554 ) ) ;
#6813 = FACE_BOUND ( 'NONE', #43414, .T. ) ;
#6814 = CARTESIAN_POINT ( 'NONE',  ( 752.4576283171824116, -405.0783235625954148, 317.7880784355627952 ) ) ;
#6815 = ORIENTED_EDGE ( 'NONE', *, *, #2421, .T. ) ;
#6816 = CARTESIAN_POINT ( 'NONE',  ( 774.6858677611749044, -273.7255117493288026, 315.5713283507209894 ) ) ;
#6817 = CARTESIAN_POINT ( 'NONE',  ( 758.6633372737375112, -44.53286901714205470, -326.9102291470432533 ) ) ;
#6818 = CARTESIAN_POINT ( 'NONE',  ( 762.1405469898971887, -169.5436935675108430, -357.8594530101015607 ) ) ;
#6819 = CARTESIAN_POINT ( 'NONE',  ( 756.5762568750052424, -219.1800572038744122, -348.7366044899774238 ) ) ;
#6820 = CARTESIAN_POINT ( 'NONE',  ( 774.6858677611749044, -417.7255117493283478, 315.5713283507209894 ) ) ;
#6821 = CARTESIAN_POINT ( 'NONE',  ( 767.7687537140311633, -95.90732993114751537, -372.7932403749916830 ) ) ;
#6822 = CARTESIAN_POINT ( 'NONE',  ( 762.1405469898973024, -97.54369356751114140, -357.8594530101016176 ) ) ;
#6823 = ORIENTED_EDGE ( 'NONE', *, *, #43817, .F. ) ;
#6824 = CARTESIAN_POINT ( 'NONE',  ( 790.9844846989617508, -382.3726999360613945, -317.2208543904092721 ) ) ;
#6826 = CARTESIAN_POINT ( 'NONE',  ( 799.2566176426618085, -432.0090635724247932, 324.0069404352559559 ) ) ;
#6825 = CARTESIAN_POINT ( 'NONE',  ( 778.2165204200184689, -118.8164208402383508, 364.9363028652563230 ) ) ;
#6827 = CARTESIAN_POINT ( 'NONE',  ( 763.2154366446407039, -117.6237781080509279, 321.4292242960311228 ) ) ;
#6830 = CARTESIAN_POINT ( 'NONE',  ( 803.8556311672234642, -345.6237781080501463, 365.6418435158340117 ) ) ;
#6829 = FACE_BOUND ( 'NONE', #13313, .T. ) ;
#6828 = DIRECTION ( 'NONE',  ( -0.000000000000000000, -0.3826834323650838421, -0.9238795325112891810 ) ) ;
#6831 = ORIENTED_EDGE ( 'NONE', *, *, #13708, .T. ) ;
#6832 = CARTESIAN_POINT ( 'NONE',  ( 798.5707757039680246, -365.4636090269705164, -356.7845633553585003 ) ) ;
#6833 = CARTESIAN_POINT ( 'NONE',  ( 759.7806653035534055, -342.9982390220557136, -324.8639956371180801 ) ) ;
#6834 = CIRCLE ( 'NONE', #35573, 7.999999999999896083 ) ;
#6835 = CARTESIAN_POINT ( 'NONE',  ( 745.1792804349281596, -182.1908817542437760, -343.7566961878542884 ) ) ;
#6836 = CARTESIAN_POINT ( 'NONE',  ( 807.2620300519052989, -24.00906357242609346, 318.0141637701419768 ) ) ;
#6838 = DIRECTION ( 'NONE',  ( -0.000000000000000000, 1.000000000000000000, -0.000000000000000000 ) ) ;
#6837 = CARTESIAN_POINT ( 'NONE',  ( 998.9999999999992042, 479.9999999999999432, -199.9999999999999716 ) ) ;
#6839 = CARTESIAN_POINT ( 'NONE',  ( 803.8651313633788504, -293.2601417444139429, -332.4468031744301015 ) ) ;
#6840 = CARTESIAN_POINT ( 'NONE',  ( 804.4286716492782716, -449.3618753856918602, -345.3141322388244703 ) ) ;
#6841 = CARTESIAN_POINT ( 'NONE',  ( 760.0363995740630116, -154.9181544815165523, -368.7758568127991907 ) ) ;
#6842 = LINE ( 'NONE', #7089, #44058 ) ;
#6843 = CARTESIAN_POINT ( 'NONE',  ( -879.9999999999992042, 260.0000000000002274, -219.9999999999999716 ) ) ;
#6844 = CARTESIAN_POINT ( 'NONE',  ( 769.9779781133707957, -379.0999726633341993, 316.7813123517150871 ) ) ;
#6845 = CARTESIAN_POINT ( 'NONE',  ( 791.0478386215596629, -333.8272453906070041, 306.7653713866226326 ) ) ;
#6846 = CARTESIAN_POINT ( 'NONE',  ( 763.0537975583476964, -216.4527844766016926, -371.0346526505628617 ) ) ;
#6847 = DIRECTION ( 'NONE',  ( 0.000000000000000000, 0.000000000000000000, -1.000000000000000000 ) ) ;
#6848 = CARTESIAN_POINT ( 'NONE',  ( 745.5313806188320314, -159.2817908451529547, 333.7943932421247268 ) ) ;
#6849 = CARTESIAN_POINT ( 'NONE',  ( 759.0252816721024374, -336.9982390220558273, -368.0189434323527280 ) ) ;
#6850 = ADVANCED_FACE ( 'NONE', ( #25489, #3791, #22237 ), #782, .T. ) ;
#6851 = CARTESIAN_POINT ( 'NONE',  ( 799.9999999999993179, -462.9681489794448339, -370.0000000000000568 ) ) ;
#6852 = CARTESIAN_POINT ( 'NONE',  ( 919.9999999999993179, 219.9999999999998863, -360.0000000000000000 ) ) ;
#6853 = CARTESIAN_POINT ( 'NONE',  ( 788.7366044899766848, -179.9073299311472454, 316.5762568750059813 ) ) ;
#6854 = VERTEX_POINT ( 'NONE', #11179 ) ;
#6855 = CARTESIAN_POINT ( 'NONE',  ( 807.2620300519052989, -408.0090635724249069, 318.0141637701419768 ) ) ;
#6856 = CARTESIAN_POINT ( 'NONE',  ( 744.9990715423526808, -378.3510508353227806, -341.2370466360926002 ) ) ;
#6857 = CARTESIAN_POINT ( 'NONE',  ( 748.9653473494363425, -122.6346026584201354, -356.9462024416521331 ) ) ;
#6858 = CARTESIAN_POINT ( 'NONE',  ( 813.1304606946830518, -425.9073299311463074, -352.3570229623690580 ) ) ;
#6859 = LINE ( 'NONE', #34807, #3329 ) ;
#6860 = CARTESIAN_POINT ( 'NONE',  ( 807.5423716828161105, -9.078323562596708030, 362.2119215644372048 ) ) ;
#6861 = ORIENTED_EDGE ( 'NONE', *, *, #44042, .T. ) ;
#6862 = EDGE_CURVE ( 'NONE', #42371, #40010, #8571, .T. ) ;
#6863 = CIRCLE ( 'NONE', #34887, 30.00000000000008171 ) ;
#6864 = CARTESIAN_POINT ( 'NONE',  ( 749.8865473780648472, -140.5328690171417634, -322.1177392798429082 ) ) ;
#6865 = CARTESIAN_POINT ( 'NONE',  ( -454.7528517110260964, 230.0000000000002274, 339.9999999999999432 ) ) ;
#6866 = CARTESIAN_POINT ( 'NONE',  ( 800.1688906516307043, -298.1692326535049347, 369.0717654672308186 ) ) ;
#6867 = CARTESIAN_POINT ( 'NONE',  ( 804.9363028652555840, -112.2709662947838325, 338.2165204200192079 ) ) ;
#6868 = CARTESIAN_POINT ( 'NONE',  ( 814.2001403089898304, -41.36187538569314626, 347.4397851343538264 ) ) ;
#6869 = EDGE_LOOP ( 'NONE', ( #38404, #20507, #32932, #20169 ) ) ;
#6870 = CARTESIAN_POINT ( 'NONE',  ( 801.9419747391806368, -306.4527844766013800, 351.9812246680014027 ) ) ;
#6871 = CARTESIAN_POINT ( 'NONE',  ( 801.1904061080336987, -20.08914811296592973, -368.3070685750235498 ) ) ;
#6872 = FACE_OUTER_BOUND ( 'NONE', #37158, .T. ) ;
#6873 = EDGE_CURVE ( 'NONE', #2099, #5978, #4693, .T. ) ;
#6874 = VERTEX_POINT ( 'NONE', #21793 ) ;
#6875 = CARTESIAN_POINT ( 'NONE',  ( 792.1044303154645831, -180.4527844766017211, -317.8323909638837677 ) ) ;
#6876 = CARTESIAN_POINT ( 'NONE',  ( 799.9636004259356241, -406.9181544815157849, -311.2241431872006956 ) ) ;
#6877 = EDGE_LOOP ( 'NONE', ( #26194, #37083, #40389, #16437 ) ) ;
#6878 = AXIS2_PLACEMENT_3D ( 'NONE', #2955, #24878, #31803 ) ;
#6879 = ADVANCED_FACE ( 'NONE', ( #36114 ), #42817, .F. ) ;
#6880 = CARTESIAN_POINT ( 'NONE',  ( 803.4237431249931660, -15.18005720387504631, 331.2633955100225194 ) ) ;
#6881 = CARTESIAN_POINT ( 'NONE',  ( 791.9812246680005501, -260.6346026584197375, -361.9419747391813189 ) ) ;
#6883 = CARTESIAN_POINT ( 'NONE',  ( 801.9858362298568863, -243.0783235625959833, 312.7379699480935642 ) ) ;
#6882 = CARTESIAN_POINT ( 'NONE',  ( 796.7737145352015204, -356.6346026584193964, 370.7187646348536987 ) ) ;
#6884 = CARTESIAN_POINT ( 'NONE',  ( 815.0009284576459549, -78.35105083532376113, 338.7629533639073429 ) ) ;
#6885 = CARTESIAN_POINT ( 'NONE',  ( 773.4516893846965786, -259.6454272087890445, -315.8398074228977066 ) ) ;
#6886 = CARTESIAN_POINT ( 'NONE',  ( 794.9819416627830151, -252.9982390220560831, -319.9864689768909898 ) ) ;
#6887 = CARTESIAN_POINT ( 'NONE',  ( -858.8365100919713768, 260.0000000000002274, -197.2499999999882903 ) ) ;
#6888 = CARTESIAN_POINT ( 'NONE',  ( 778.2165204200184689, -118.8164208402383508, -364.9363028652563230 ) ) ;
#6889 = CARTESIAN_POINT ( 'NONE',  ( 795.1360043628807261, -236.0891481129651766, 360.2193346964456282 ) ) ;
#6890 = VERTEX_POINT ( 'NONE', #14422 ) ;
#6891 = CARTESIAN_POINT ( 'NONE',  ( 749.2812353651451076, -390.4527844766011526, 323.2262854647983090 ) ) ;
#6892 = DIRECTION ( 'NONE',  ( 0.000000000000000000, 0.000000000000000000, -1.000000000000000000 ) ) ;
#6893 = CARTESIAN_POINT ( 'NONE',  ( 749.5768839229115201, -36.55451811788061178, -358.0661480581553064 ) ) ;
#6894 = DIRECTION ( 'NONE',  ( 0.000000000000000000, 0.000000000000000000, -1.000000000000000000 ) ) ;
#6895 = CARTESIAN_POINT ( 'NONE',  ( 927.9999999999992042, 219.9999999999998863, -360.0000000000000000 ) ) ;
#6896 = CARTESIAN_POINT ( 'NONE',  ( 763.8424801807145741, -258.0090635724253616, 320.5453621957614700 ) ) ;
#6897 = CARTESIAN_POINT ( 'NONE',  ( 781.8018195045266339, -118.2709662947837899, 365.1927285166406705 ) ) ;
#6898 = ORIENTED_EDGE ( 'NONE', *, *, #29198, .T. ) ;
#6899 = CARTESIAN_POINT ( 'NONE',  ( 772.4468031744293057, -9.827245390607961539, -363.8651313633793620 ) ) ;
#6900 = AXIS2_PLACEMENT_3D ( 'NONE', #21973, #935, #38668 ) ;
#6901 = CARTESIAN_POINT ( 'NONE',  ( 792.3570229623691148, -69.18005720387488111, -373.1304606946836770 ) ) ;
#6902 = VECTOR ( 'NONE', #40429, 1000.000000000000000 ) ;
#6903 = CARTESIAN_POINT ( 'NONE',  ( 765.8855110935204493, -286.1692326535048778, 319.0159684113471599 ) ) ;
#6904 = DIRECTION ( 'NONE',  ( 0.000000000000000000, -1.000000000000000000, 0.000000000000000000 ) ) ;
#6905 = EDGE_CURVE ( 'NONE', #23400, #8383, #28501, .T. ) ;
#6906 = CARTESIAN_POINT ( 'NONE',  ( 802.2119215644370342, -6.009063572426154742, 367.5423716828165084 ) ) ;
#6907 = CARTESIAN_POINT ( 'NONE',  ( 767.6429770376289525, -201.1800572038744690, -306.8695393053162093 ) ) ;
#6908 = EDGE_CURVE ( 'NONE', #1390, #6318, #25029, .T. ) ;
#6909 = CARTESIAN_POINT ( 'NONE',  ( 772.4837098697144029, -191.3618753856925991, 374.5518280994205611 ) ) ;
#6910 = CARTESIAN_POINT ( 'NONE',  ( 774.6858677611749044, -81.72551174932937101, 315.5713283507209894 ) ) ;
#6911 = CARTESIAN_POINT ( 'NONE',  ( 998.9999999999992042, 479.9999999999999432, -360.0000000000000000 ) ) ;
#6912 = CARTESIAN_POINT ( 'NONE',  ( 764.3348316497523456, -286.7146871989594388, -308.6759233522265617 ) ) ;
#6913 = CIRCLE ( 'NONE', #29050, 9.999999999999980460 ) ;
#6914 = CARTESIAN_POINT ( 'NONE',  ( 769.9779781133707957, 4.900027336664720679, 316.7813123517150871 ) ) ;
#6915 = CARTESIAN_POINT ( 'NONE',  ( 772.4837098697144029, -287.3618753856923718, -374.5518280994205611 ) ) ;
#6916 = CARTESIAN_POINT ( 'NONE',  ( 831.1634899080286232, 229.9999999999998863, -199.9999999999999432 ) ) ;
#6917 = CARTESIAN_POINT ( 'NONE',  ( 799.4546378042377910, -369.0783235625956422, 356.1575198192848006 ) ) ;
#6918 = CARTESIAN_POINT ( 'NONE',  ( 772.4837098697145166, -47.36187538569312494, 374.5518280994205611 ) ) ;
#6919 = EDGE_CURVE ( 'NONE', #20856, #7346, #12316, .T. ) ;
#6920 = CARTESIAN_POINT ( 'NONE',  ( 804.6798772138708955, -375.7255117493283478, -334.6312213355107019 ) ) ;
#6921 = EDGE_CURVE ( 'NONE', #11789, #11328, #40179, .T. ) ;
#6922 = CARTESIAN_POINT ( 'NONE',  ( 764.0069404352550464, -63.07832356259653750, 359.2566176426627180 ) ) ;
#6923 = CARTESIAN_POINT ( 'NONE',  ( 786.2056067578752163, -35.80559628986934229, -374.4686193811670023 ) ) ;
#6924 = CARTESIAN_POINT ( 'NONE',  ( 759.2295555964440155, -184.1692326535052757, -353.9708237608231229 ) ) ;
#6925 = CARTESIAN_POINT ( 'NONE',  ( 786.2056067578752163, -203.8055962898688449, 374.4686193811670023 ) ) ;
#6926 = CARTESIAN_POINT ( 'NONE',  ( 754.8072714833583632, -4.816420840238714085, 338.1981804954721156 ) ) ;
#6927 = CARTESIAN_POINT ( 'NONE',  ( 776.9566956441375396, -372.8965053807773415, 364.8461984189686405 ) ) ;
#6928 = VERTEX_POINT ( 'NONE', #5357 ) ;
#6929 = CARTESIAN_POINT ( 'NONE',  ( 756.1348686366196716, -185.2601417444143692, -347.5531968255698416 ) ) ;
#6930 = CARTESIAN_POINT ( 'NONE',  ( 765.0180583372156207, -192.9982390220562820, 360.0135310231089534 ) ) ;
#6931 = CARTESIAN_POINT ( 'NONE',  ( 807.5423716828161105, -33.07832356259662987, -362.2119215644372048 ) ) ;
#6932 = CARTESIAN_POINT ( 'NONE',  ( 756.3353852180820240, -341.9073299311466485, 331.1735550268787733 ) ) ;
#6933 = AXIS2_PLACEMENT_3D ( 'NONE', #27413, #42413, #23702 ) ;
#6934 = CARTESIAN_POINT ( 'NONE',  ( 831.1634899080286232, 239.9999999999998863, -202.7499999999998295 ) ) ;
#6935 = CIRCLE ( 'NONE', #36445, 8.025000000000003908 ) ;
#6936 = ORIENTED_EDGE ( 'NONE', *, *, #15003, .T. ) ;
#6937 = CARTESIAN_POINT ( 'NONE',  ( 761.2382568024794409, -39.62377810805116951, 356.9571628226838129 ) ) ;
#6938 = CARTESIAN_POINT ( 'NONE',  ( 807.2620300519052989, -312.0090635724251911, -318.0141637701419768 ) ) ;
#6939 = ADVANCED_FACE ( 'NONE', ( #30528 ), #36790, .T. ) ;
#6940 = CARTESIAN_POINT ( 'NONE',  ( 814.9108240113580450, -256.2709662947834204, 337.5031285880265273 ) ) ;
#6941 = CARTESIAN_POINT ( 'NONE',  ( 766.9102291470427417, -330.5545181178796952, 318.6633372737382501 ) ) ;
#6942 = CARTESIAN_POINT ( 'NONE',  ( 773.3843516231979720, -421.4419599262317888, 364.4086373105754433 ) ) ;
#6943 = CARTESIAN_POINT ( 'NONE',  ( 801.5560724626406000, -144.5545181178802636, -326.7756240680316182 ) ) ;
#6944 = CARTESIAN_POINT ( 'NONE',  ( 765.0180583372156207, -144.9982390220564525, -360.0135310231089534 ) ) ;
#6945 = CARTESIAN_POINT ( 'NONE',  ( 795.1360043628808398, -356.0891481129648355, -360.2193346964456282 ) ) ;
#6946 = ORIENTED_EDGE ( 'NONE', *, *, #26405, .F. ) ;
#6947 = CARTESIAN_POINT ( 'NONE',  ( 814.9108240113580450, -304.2709662947832499, 337.5031285880265273 ) ) ;
#6948 = AXIS2_PLACEMENT_3D ( 'NONE', #4159, #33020, #28854 ) ;
#6949 = CARTESIAN_POINT ( 'NONE',  ( 754.9735926884551418, -330.3510508353229511, 340.5236548041000333 ) ) ;
#6950 = DIRECTION ( 'NONE',  ( 0.000000000000000000, 0.000000000000000000, -1.000000000000000000 ) ) ;
#6951 = VECTOR ( 'NONE', #34287, 1000.000000000000000 ) ;
#6952 = CARTESIAN_POINT ( 'NONE',  ( 759.0159684113467620, -112.9181544815167229, 325.8855110935213020 ) ) ;
#6953 = CARTESIAN_POINT ( 'NONE',  ( 785.3141322388236176, -21.72551174932956641, 364.4286716492789537 ) ) ;
#6954 = EDGE_LOOP ( 'NONE', ( #33679, #29390, #23621, #12123 ) ) ;
#6955 = CARTESIAN_POINT ( 'NONE',  ( 786.2694204179717872, -381.2817908451523294, -305.1769319972829067 ) ) ;
#6956 = LINE ( 'NONE', #35127, #38755 ) ;
#6957 = CARTESIAN_POINT ( 'NONE',  ( 757.0176451133909268, -229.0999726633345404, 349.9200121543848354 ) ) ;
#6958 = CARTESIAN_POINT ( 'NONE',  ( 773.7305795820266212, -249.2817908451526421, 374.8230680027170365 ) ) ;
#6959 = CARTESIAN_POINT ( 'NONE',  ( 798.7617431975189675, -195.6237781080506863, 323.0428371773161871 ) ) ;
#6960 = CARTESIAN_POINT ( 'NONE',  ( 762.1405469898971887, -337.5436935675102177, -357.8594530101015607 ) ) ;
#6961 = EDGE_CURVE ( 'NONE', #16350, #3536, #16219, .T. ) ;
#6962 = CARTESIAN_POINT ( 'NONE',  ( 939.9999999999993179, -590.0000000000001137, 201.9999999999998579 ) ) ;
#6963 = CARTESIAN_POINT ( 'NONE',  ( 769.9779781133707957, -211.0999726633346540, -316.7813123517150871 ) ) ;
#6964 = EDGE_CURVE ( 'NONE', #24418, #16954, #29854, .T. ) ;
#6965 = VECTOR ( 'NONE', #8165, 1000.000000000000000 ) ;
#6966 = CARTESIAN_POINT ( 'NONE',  ( 749.2812353651451076, -30.45278447660226817, 323.2262854647983090 ) ) ;
#6967 = CARTESIAN_POINT ( 'NONE',  ( 758.8095938919642549, -80.08914811296574499, 311.6929314249763365 ) ) ;
#6968 = CARTESIAN_POINT ( 'NONE',  ( 804.5667330414263461, -452.9681489794450044, 348.7981942340067576 ) ) ;
#6969 = CARTESIAN_POINT ( 'NONE',  ( 767.6429770376291799, -417.1800572038736732, -306.8695393053162093 ) ) ;
#6970 = CIRCLE ( 'NONE', #34248, 2.749999999999835687 ) ;
#6971 = DIRECTION ( 'NONE',  ( 1.000000000000000000, 0.000000000000000000, 0.000000000000000000 ) ) ;
#6972 = CARTESIAN_POINT ( 'NONE',  ( 788.6739635108323228, -343.6454272087887603, 373.9316612368139090 ) ) ;
#6973 = CARTESIAN_POINT ( 'NONE',  ( 793.5337260303429048, -457.7979077669877483, -366.8220830107578649 ) ) ;
#6974 = CARTESIAN_POINT ( 'NONE',  ( 751.6929314249748586, -318.9982390220557704, 318.8095938919659034 ) ) ;
#6975 = CARTESIAN_POINT ( 'NONE',  ( 814.2001403089898304, -41.36187538569314626, -347.4397851343538264 ) ) ;
#6976 = CARTESIAN_POINT ( 'NONE',  ( 754.8072714833581358, -268.8164208402378108, -338.1981804954720587 ) ) ;
#6977 = FACE_BOUND ( 'NONE', #3494, .T. ) ;
#6978 = PRODUCT_RELATED_PRODUCT_CATEGORY ( 'part', '', ( #21473 ) ) ;
#6979 = CARTESIAN_POINT ( 'NONE',  ( 803.6646147819161570, -377.9073299311466485, 348.8264449731210561 ) ) ;
#6980 = CARTESIAN_POINT ( 'NONE',  ( 787.5531968255692163, -165.8272453906074873, 316.1348686366205811 ) ) ;
#6981 = CARTESIAN_POINT ( 'NONE',  ( 762.1177392798416577, -42.55451811788057626, -309.8865473780659272 ) ) ;
#6982 = CARTESIAN_POINT ( 'NONE',  ( 798.7617431975189675, -75.62377810805104161, -323.0428371773161871 ) ) ;
#6983 = CARTESIAN_POINT ( 'NONE',  ( 771.2368401574024119, -61.44195992623291147, 374.2805881961240857 ) ) ;
#6984 = CARTESIAN_POINT ( 'NONE',  ( 800.0135310231082713, -398.0891481129647218, 325.0180583372163028 ) ) ;
#6985 = CARTESIAN_POINT ( 'NONE',  ( 810.7187646348534145, 5.547215523397618142, 356.7737145352016341 ) ) ;
#6986 = AXIS2_PLACEMENT_3D ( 'NONE', #40613, #37368, #12652 ) ;
#6987 = DIRECTION ( 'NONE',  ( 0.000000000000000000, -0.9238795325112892920, 0.3826834323650836756 ) ) ;
#6988 = CARTESIAN_POINT ( 'NONE',  ( 778.1981804954714335, -10.27096629478414691, -314.8072714833589885 ) ) ;
#6990 = ORIENTED_EDGE ( 'NONE', *, *, #41635, .F. ) ;
#6989 = CARTESIAN_POINT ( 'NONE',  ( 790.8726784830453198, -106.7146871989600498, -362.5472867521010585 ) ) ;
#6991 = CARTESIAN_POINT ( 'NONE',  ( 785.3141322388236176, -69.72551174932942786, -364.4286716492789537 ) ) ;
#6992 = CIRCLE ( 'NONE', #15147, 9.999999999999980460 ) ;
#6993 = CARTESIAN_POINT ( 'NONE',  ( 757.2208543904082489, -400.7146871989590977, -350.9844846989624330 ) ) ;
#6995 = CARTESIAN_POINT ( 'NONE',  ( 756.3353852180820240, -221.9073299311471033, 331.1735550268787733 ) ) ;
#6994 = CARTESIAN_POINT ( 'NONE',  ( 803.6646147819161570, -233.9073299311470180, 348.8264449731210561 ) ) ;
#6996 = CARTESIAN_POINT ( 'NONE',  ( 776.2433038121456548, -396.8965053807772847, -374.8207195650711014 ) ) ;
#6997 = CARTESIAN_POINT ( 'NONE',  ( 767.6429770376289525, 14.81994279612486309, 306.8695393053162093 ) ) ;
#6998 = DIRECTION ( 'NONE',  ( 0.000000000000000000, 0.6755902076156505842, 0.7372773368101327440 ) ) ;
#6999 = ORIENTED_EDGE ( 'NONE', *, *, #4385, .F. ) ;
#7000 = CARTESIAN_POINT ( 'NONE',  ( 781.7834795799800531, -442.8164208402372992, 315.0636971347436202 ) ) ;
#7001 = VERTEX_POINT ( 'NONE', #9058 ) ;
#7002 = CARTESIAN_POINT ( 'NONE',  ( 772.5602148656447525, -249.7255117493288594, -305.7998596910095443 ) ) ;
#7003 = CARTESIAN_POINT ( 'NONE',  ( 796.9462024416508257, -156.4527844766018916, 308.9653473494370246 ) ) ;
#7004 = CLOSED_SHELL ( 'NONE', ( #11735, #8851, #8351, #2085, #35382, #6276, #36538, #13914 ) ) ;
#7005 = ORIENTED_EDGE ( 'NONE', *, *, #12262, .F. ) ;
#7006 = CARTESIAN_POINT ( 'NONE',  ( 801.9419747391806368, -234.4527844766016358, -351.9812246680014027 ) ) ;
#7007 = EDGE_LOOP ( 'NONE', ( #41414, #44382, #26150, #19772 ) ) ;
#7008 = CARTESIAN_POINT ( 'NONE',  ( 785.3141322388236176, -357.7255117493285184, -364.4286716492789537 ) ) ;
#7009 = CARTESIAN_POINT ( 'NONE',  ( 792.1044303154645831, -12.45278447660232146, -317.8323909638837677 ) ) ;
#7010 = CARTESIAN_POINT ( 'NONE',  ( 755.0488828828309806, -233.8055962898687028, 344.1219089521771934 ) ) ;
#7011 = PLANE ( 'NONE',  #21086 ) ;
#7012 = CARTESIAN_POINT ( 'NONE',  ( 180.7583438952258916, 294.6698570112193920, -274.9999999999999432 ) ) ;
#7013 = ORIENTED_EDGE ( 'NONE', *, *, #38114, .F. ) ;
#7014 = CARTESIAN_POINT ( 'NONE',  ( 805.1927285166397041, -16.81642084023866701, -341.8018195045277707 ) ) ;
#7015 = DIRECTION ( 'NONE',  ( 0.000000000000000000, -0.6594541114781790059, -0.7517448203044204691 ) ) ;
#7016 = EDGE_LOOP ( 'NONE', ( #4819, #3878 ) ) ;
#7017 = CARTESIAN_POINT ( 'NONE',  ( 814.8207195650702488, -266.1908817542435486, -336.2433038121456548 ) ) ;
#7018 = AXIS2_PLACEMENT_3D ( 'NONE', #17935, #32004, #14477 ) ;
#7019 = CARTESIAN_POINT ( 'NONE',  ( 776.2046728542105711, -140.1908817542438896, 304.8212110874238761 ) ) ;
#7020 = CIRCLE ( 'NONE', #34307, 10.00000000000000888 ) ;
#7022 = CARTESIAN_POINT ( 'NONE',  ( 778.2165204200184689, -238.8164208402379813, -364.9363028652563230 ) ) ;
#7021 = FACE_BOUND ( 'NONE', #21478, .T. ) ;
#7023 = CARTESIAN_POINT ( 'NONE',  ( 779.4709603349208464, -408.3510508353227806, -314.7162404726379918 ) ) ;
#7024 = DIRECTION ( 'NONE',  ( -1.000000000000000000, -0.000000000000000000, 0.000000000000000000 ) ) ;
#7025 = DIRECTION ( 'NONE',  ( -1.000000000000000000, -0.000000000000000000, -0.000000000000000000 ) ) ;
#7026 = CARTESIAN_POINT ( 'NONE',  ( 802.5472867521000353, -100.3726999360622187, -350.8726784830461156 ) ) ;
#7027 = AXIS2_PLACEMENT_3D ( 'NONE', #45159, #13521, #13756 ) ;
#7028 = AXIS2_PLACEMENT_3D ( 'NONE', #19278, #29904, #43094 ) ;
#7029 = CARTESIAN_POINT ( 'NONE',  ( 764.1737431748507561, -394.3726999360613377, 371.6461892240376415 ) ) ;
#7030 = CARTESIAN_POINT ( 'NONE',  ( 879.9999999999990905, 479.9999999999998863, 210.0000000000000000 ) ) ;
#7031 = CARTESIAN_POINT ( 'NONE',  ( 799.4546378042377910, -441.0783235625953580, -356.1575198192848006 ) ) ;
#7032 = CARTESIAN_POINT ( 'NONE',  ( 808.0189434323515343, -326.0891481129649492, -319.0252816721025511 ) ) ;
#7033 = DIRECTION ( 'NONE',  ( -0.000000000000000000, 1.000000000000000000, -0.000000000000000000 ) ) ;
#7034 = CYLINDRICAL_SURFACE ( 'NONE', #12830, 10.00000000000000888 ) ;
#7035 = CARTESIAN_POINT ( 'NONE',  ( 803.4237431249931660, -87.18005720387481006, -331.2633955100225194 ) ) ;
#7036 = CARTESIAN_POINT ( 'NONE',  ( 813.5763878283155464, -243.8272453906072030, 351.1614460488615350 ) ) ;
#7037 = CARTESIAN_POINT ( 'NONE',  ( 805.9055244015594326, -219.6237781080506295, -315.8990559732753240 ) ) ;
#7038 = CARTESIAN_POINT ( 'NONE',  ( 749.2812353651451076, -222.4527844766016642, 323.2262854647983090 ) ) ;
#7039 = CARTESIAN_POINT ( 'NONE',  ( 800.9747183278959710, -444.9982390220554862, -311.9810565676471583 ) ) ;
#7040 = DIRECTION ( 'NONE',  ( -1.000000000000000000, -0.000000000000000000, -0.000000000000000000 ) ) ;
#7041 = AXIS2_PLACEMENT_3D ( 'NONE', #42304, #17833, #21063 ) ;
#7042 = CARTESIAN_POINT ( 'NONE',  ( 803.6646147819161570, -305.9073299311467622, 348.8264449731210561 ) ) ;
#7043 = VECTOR ( 'NONE', #26872, 1000.000000000000000 ) ;
#7044 = CARTESIAN_POINT ( 'NONE',  ( 755.3028492785439312, -87.28179084515316788, 335.9200461376539693 ) ) ;
#7045 = CARTESIAN_POINT ( 'NONE',  ( 804.1601925771018387, 16.55804007376685050, -346.5483106153029098 ) ) ;
#7046 = AXIS2_PLACEMENT_3D ( 'NONE', #17229, #45422, #21156 ) ;
#7047 = CARTESIAN_POINT ( 'NONE',  ( 939.9999999999992042, 62.85347435602262323, -357.4246812887967621 ) ) ;
#7048 = CARTESIAN_POINT ( 'NONE',  ( -28.63011601220122415, -496.5085659523897448, -356.8883017825714319 ) ) ;
#7050 = CARTESIAN_POINT ( 'NONE',  ( 803.6646147819161570, -329.9073299311467053, 348.8264449731210561 ) ) ;
#7049 = CARTESIAN_POINT ( 'NONE',  ( 803.2186876482843445, -127.9874144716872308, 350.0220218866286928 ) ) ;
#7051 = ORIENTED_EDGE ( 'NONE', *, *, #39058, .F. ) ;
#7052 = VECTOR ( 'NONE', #44972, 1000.000000000000000 ) ;
#7053 = CARTESIAN_POINT ( 'NONE',  ( 760.5453621957607311, -261.0783235625959264, -323.8424801807151425 ) ) ;
#7054 = CARTESIAN_POINT ( 'NONE',  ( 762.3223304703356007, -103.5436935675111272, 322.3223304703362828 ) ) ;
#7055 = CARTESIAN_POINT ( 'NONE',  ( 798.0661480581538854, -290.5328690171412518, -309.5768839229118043 ) ) ;
#7056 = LINE ( 'NONE', #42153, #20163 ) ;
#7057 = CARTESIAN_POINT ( 'NONE',  ( 801.9858362298568863, -411.0783235625954717, 312.7379699480935642 ) ) ;
#7058 = ORIENTED_EDGE ( 'NONE', *, *, #17396, .F. ) ;
#7059 = CARTESIAN_POINT ( 'NONE',  ( 804.6798772138708955, -303.7255117493287457, 334.6312213355107019 ) ) ;
#7060 = VECTOR ( 'NONE', #39739, 1000.000000000000114 ) ;
#7061 = CARTESIAN_POINT ( 'NONE',  ( 804.1601925771018387, -31.44195992623299674, -346.5483106153029098 ) ) ;
#7062 = CARTESIAN_POINT ( 'NONE',  ( 774.6858677611749044, -177.7255117493290868, -315.5713283507209894 ) ) ;
#7063 = CARTESIAN_POINT ( 'NONE',  ( 785.3687786644884454, -203.3618753856925991, -315.3201227861279676 ) ) ;
#7064 = CARTESIAN_POINT ( 'NONE',  ( 754.8072714833581358, -412.8164208402372992, 338.1981804954720587 ) ) ;
#7065 = AXIS2_PLACEMENT_3D ( 'NONE', #32447, #39844, #32211 ) ;
#7066 = CARTESIAN_POINT ( 'NONE',  ( 814.5518280994195948, -159.7255117493291436, -332.4837098697145734 ) ) ;
#7067 = CIRCLE ( 'NONE', #8551, 10.00000000000000888 ) ;
#7068 = CARTESIAN_POINT ( 'NONE',  ( 795.1360043628808398, -92.08914811296570235, -360.2193346964456282 ) ) ;
#7069 = ORIENTED_EDGE ( 'NONE', *, *, #40142, .T. ) ;
#7070 = CARTESIAN_POINT ( 'NONE',  ( 787.5531968255692163, -381.8272453906068336, -316.1348686366205811 ) ) ;
#7072 = CARTESIAN_POINT ( 'NONE',  ( 757.4527132478984868, -448.3726999360611103, 329.1273215169538844 ) ) ;
#7071 = CARTESIAN_POINT ( 'NONE',  ( 771.2633955100217236, -119.9073299311474443, 363.4237431249939618 ) ) ;
#7073 = CARTESIAN_POINT ( 'NONE',  ( 776.9566956441375396, -132.8965053807781374, 364.8461984189686405 ) ) ;
#7076 = CARTESIAN_POINT ( 'NONE',  ( 778.7502325331095108, -408.3510508353227806, 304.6391490659818828 ) ) ;
#7075 = CARTESIAN_POINT ( 'NONE',  ( 799.9999999999993179, -512.9681489794448908, 339.9999999999999432 ) ) ;
#7074 = CARTESIAN_POINT ( 'NONE',  ( 999.9999999999992042, 248.9999999999998863, 360.0000000000000000 ) ) ;
#7077 = ORIENTED_EDGE ( 'NONE', *, *, #16579, .T. ) ;
#7078 = CARTESIAN_POINT ( 'NONE',  ( 790.0220218866281812, -367.0999726633342561, -363.2186876482849129 ) ) ;
#7079 = CARTESIAN_POINT ( 'NONE',  ( 804.4286716492782716, -353.3618753856922012, -345.3141322388244703 ) ) ;
#7080 = CARTESIAN_POINT ( 'NONE',  ( 760.0363995740630116, -154.9181544815165523, -368.7758568127991907 ) ) ;
#7081 = AXIS2_PLACEMENT_3D ( 'NONE', #41899, #7480, #45602 ) ;
#7082 = CARTESIAN_POINT ( 'NONE',  ( 814.8207195650702488, -50.19088175424420939, 336.2433038121456548 ) ) ;
#7083 = CIRCLE ( 'NONE', #1907, 24.99999999999991118 ) ;
#7085 = CARTESIAN_POINT ( 'NONE',  ( 879.9999999999992042, 99.99999999999984368, 350.0000000000000000 ) ) ;
#7084 = DIRECTION ( 'NONE',  ( 1.000000000000000000, 0.000000000000000000, 0.000000000000000000 ) ) ;
#7086 = CARTESIAN_POINT ( 'NONE',  ( 776.9566956441375396, -300.8965053807775689, -364.8461984189686405 ) ) ;
#7087 = CARTESIAN_POINT ( 'NONE',  ( 791.9812246680005501, -452.6346026584191691, -361.9419747391813189 ) ) ;
#7088 = CARTESIAN_POINT ( 'NONE',  ( 745.7194118038753459, -157.6454272087893287, -348.7631598425976449 ) ) ;
#7089 = CARTESIAN_POINT ( 'NONE',  ( -265.7583438952258916, 290.0000000000001705, -320.0000000000000000 ) ) ;
#7090 = FACE_OUTER_BOUND ( 'NONE', #2977, .T. ) ;
#7091 = CIRCLE ( 'NONE', #12981, 7.999999999999896083 ) ;
#7092 = CARTESIAN_POINT ( 'NONE',  ( 757.4527132478984868, -376.3726999360614514, 329.1273215169538844 ) ) ;
#7093 = CARTESIAN_POINT ( 'NONE',  ( 795.8262568251477660, -334.3726999360615082, 308.3538107759623585 ) ) ;
#7094 = CARTESIAN_POINT ( 'NONE',  ( 814.5518280994195948, -207.7255117493289731, -332.4837098697145166 ) ) ;
#7095 = DIRECTION ( 'NONE',  ( 0.000000000000000000, 0.000000000000000000, -1.000000000000000000 ) ) ;
#7096 = DIRECTION ( 'NONE',  ( -1.000000000000000000, 0.000000000000000000, 0.000000000000000000 ) ) ;
#7097 = VECTOR ( 'NONE', #33793, 1000.000000000000000 ) ;
#7098 = CARTESIAN_POINT ( 'NONE',  ( 814.4686193811664907, -147.2817908451529547, 346.2056067578752732 ) ) ;
#7099 = CARTESIAN_POINT ( 'NONE',  ( 783.7566961878529810, -96.89650538077825104, -305.1792804349288417 ) ) ;
#7100 = CARTESIAN_POINT ( 'NONE',  ( 812.7932403749906598, -327.1800572038741279, -327.7687537140311633 ) ) ;
#7101 = AXIS2_PLACEMENT_3D ( 'NONE', #27862, #41957, #10299 ) ;
#7102 = CARTESIAN_POINT ( 'NONE',  ( -784.4999999999993179, -365.3551492539851893, -18.13243251470705886 ) ) ;
#7103 = CARTESIAN_POINT ( 'NONE',  ( 786.4999999999993179, -110.5936016518799221, 750.6326042729449455 ) ) ;
#7104 = CARTESIAN_POINT ( 'NONE',  ( 768.0187753319979720, -176.6346026584199933, 318.0580252608186242 ) ) ;
#7105 = EDGE_LOOP ( 'NONE', ( #40674, #23927, #10024, #9838 ) ) ;
#7106 = CARTESIAN_POINT ( 'NONE',  ( 757.7880784355613741, -450.0090635724248500, 312.4576283171834916 ) ) ;
#7107 = CARTESIAN_POINT ( 'NONE',  ( 771.2368401574024119, -373.4419599262319593, -374.2805881961240857 ) ) ;
#7108 = CARTESIAN_POINT ( 'NONE',  ( 747.2067596250078623, -147.1800572038746395, -352.2312462859687230 ) ) ;
#7109 = CARTESIAN_POINT ( 'NONE',  ( 811.0346526505616112, -422.6346026584192259, -323.0537975583477532 ) ) ;
#7110 = CARTESIAN_POINT ( 'NONE',  ( 786.4999999999993179, 22.32581219114657856, 895.6886905569881492 ) ) ;
#7111 = CARTESIAN_POINT ( 'NONE',  ( 783.7566961878529810, -0.8965053807785533513, 305.1792804349288417 ) ) ;
#7112 = ORIENTED_EDGE ( 'NONE', *, *, #39964, .F. ) ;
#7113 = CARTESIAN_POINT ( 'NONE',  ( 752.4576283171824116, -189.0783235625961822, -317.7880784355627952 ) ) ;
#7114 = FILL_AREA_STYLE ('',( #19363 ) ) ;
#7115 = CARTESIAN_POINT ( 'NONE',  ( 758.0141637701419768, -303.0783235625957559, 367.2620300519063790 ) ) ;
#7116 = CARTESIAN_POINT ( 'NONE',  ( 768.0187753319979720, -104.6346026584202207, 318.0580252608186242 ) ) ;
#7117 = ORIENTED_EDGE ( 'NONE', *, *, #32297, .F. ) ;
#7118 = CARTESIAN_POINT ( 'NONE',  ( 758.0580252608178853, -318.4527844766014368, 328.0187753319985404 ) ) ;
#7119 = VECTOR ( 'NONE', #26208, 1000.000000000000114 ) ;
#7120 = CARTESIAN_POINT ( 'NONE',  ( 745.4481719005789273, -27.72551174932954510, -347.5162901302853129 ) ) ;
#7121 = CARTESIAN_POINT ( 'NONE',  ( 814.5518280994195948, -87.72551174932935680, 332.4837098697145166 ) ) ;
#7122 = ORIENTED_EDGE ( 'NONE', *, *, #26985, .F. ) ;
#7123 = CARTESIAN_POINT ( 'NONE',  ( 799.9636004259356241, -430.9181544815157849, -311.2241431872006956 ) ) ;
#7124 = ORIENTED_EDGE ( 'NONE', *, *, #43627, .T. ) ;
#7125 = CONTEXT_DEPENDENT_SHAPE_REPRESENTATION ( #25199, #33962 ) ;
#7126 = CARTESIAN_POINT ( 'NONE',  ( 755.3201227861273992, -27.72551174932954510, 345.3687786644892981 ) ) ;
#7127 = CARTESIAN_POINT ( 'NONE',  ( 785.3687786644884454, -251.3618753856923149, -315.3201227861279676 ) ) ;
#7128 = CIRCLE ( 'NONE', #1216, 10.00000000000000888 ) ;
#7130 = CARTESIAN_POINT ( 'NONE',  ( 766.5853460496234675, -277.9874144716867477, 372.3518521366060554 ) ) ;
#7129 = CARTESIAN_POINT ( 'NONE',  ( 751.9810565676468741, -362.0891481129648923, 360.9747183278973921 ) ) ;
#7131 = CARTESIAN_POINT ( 'NONE',  ( 793.4146539503750546, -73.98741447168741558, 307.6481478633938877 ) ) ;
#7132 = CARTESIAN_POINT ( 'NONE',  ( 766.9102291470427417, -258.5545181178799226, -318.6633372737382501 ) ) ;
#7133 = CARTESIAN_POINT ( 'NONE',  ( 781.8018195045266339, -262.2709662947831930, -365.1927285166406705 ) ) ;
#7134 = CARTESIAN_POINT ( 'NONE',  ( 803.4237431249931660, -447.1800572038736732, -331.2633955100225194 ) ) ;
#7135 = CARTESIAN_POINT ( 'NONE',  ( 788.8264449731200330, -117.1800572038746964, -363.6646147819171233 ) ) ;
#7136 = CARTESIAN_POINT ( 'NONE',  ( 762.3223304703356007, -247.5436935675106724, 322.3223304703362828 ) ) ;
#7137 = CARTESIAN_POINT ( 'NONE',  ( 814.9108240113580450, -376.2709662947829656, 337.5031285880265273 ) ) ;
#7139 = LINE ( 'NONE', #19905, #34404 ) ;
#7138 = FACE_OUTER_BOUND ( 'NONE', #18912, .T. ) ;
#7140 = CARTESIAN_POINT ( 'NONE',  ( 747.6481478633932056, -61.09997266333506616, -353.4146539503763620 ) ) ;
#7141 = DIRECTION ( 'NONE',  ( 1.000000000000000000, -0.000000000000000000, -0.000000000000000000 ) ) ;
#7142 = CARTESIAN_POINT ( 'NONE',  ( 939.9999999999994316, -428.4497686941065240, 352.6378164459125628 ) ) ;
#7143 = EDGE_CURVE ( 'NONE', #33570, #39336, #43847, .T. ) ;
#7144 = CARTESIAN_POINT ( 'NONE',  ( 786.5483106153019435, -271.6454272087889876, 364.1601925771022366 ) ) ;
#7145 = CARTESIAN_POINT ( 'NONE',  ( 800.0135310231082713, -110.0891481129656597, 325.0180583372163028 ) ) ;
#7146 = ORIENTED_EDGE ( 'NONE', *, *, #14334, .T. ) ;
#7147 = CARTESIAN_POINT ( 'NONE',  ( 779.4763451958990572, -8.736336299698871599, -365.0264073115438919 ) ) ;
#7148 = EDGE_CURVE ( 'NONE', #40010, #30797, #8630, .T. ) ;
#7149 = CARTESIAN_POINT ( 'NONE',  ( 810.7187646348534145, -90.45278447660209054, -356.7737145352016341 ) ) ;
#7150 = CARTESIAN_POINT ( 'NONE',  ( 763.2154366446407039, -285.6237781080502600, 321.4292242960311228 ) ) ;
#7151 = DIRECTION ( 'NONE',  ( 0.000000000000000000, -1.000000000000000000, 0.000000000000000000 ) ) ;
#7152 = CARTESIAN_POINT ( 'NONE',  ( 814.4686193811664907, -27.28179084515336328, 346.2056067578752732 ) ) ;
#7153 = AXIS2_PLACEMENT_3D ( 'NONE', #17028, #31105, #13565 ) ;
#7155 = VECTOR ( 'NONE', #7141, 1000.000000000000000 ) ;
#7154 = CARTESIAN_POINT ( 'NONE',  ( 792.2312462859673587, -251.9073299311470748, -307.2067596250082602 ) ) ;
#7156 = CARTESIAN_POINT ( 'NONE',  ( 767.6429770376289525, -177.1800572038744690, 306.8695393053162093 ) ) ;
#7157 = CARTESIAN_POINT ( 'NONE',  ( 765.0180583372156207, -96.99823902205660886, 360.0135310231089534 ) ) ;
#7158 = VECTOR ( 'NONE', #1763, 1000.000000000000000 ) ;
#7159 = CARTESIAN_POINT ( 'NONE',  ( 815.1787889125755555, -270.8965053807777394, -343.7953271457877804 ) ) ;
#7160 = VECTOR ( 'NONE', #17348, 1000.000000000000000 ) ;
#7161 = CARTESIAN_POINT ( 'NONE',  ( 773.7305795820266212, -441.2817908451521021, 374.8230680027170365 ) ) ;
#7162 = CARTESIAN_POINT ( 'NONE',  ( 812.7932403749906598, -303.1800572038740711, -327.7687537140311633 ) ) ;
#7163 = DIRECTION ( 'NONE',  ( 0.000000000000000000, 0.000000000000000000, 1.000000000000000000 ) ) ;
#7164 = CARTESIAN_POINT ( 'NONE',  ( 805.1016975059191054, -366.8965053807773984, 343.0745993439771837 ) ) ;
#7165 = CARTESIAN_POINT ( 'NONE',  ( 792.2312462859673587, -35.90732993114770011, 307.2067596250082602 ) ) ;
#7166 = CARTESIAN_POINT ( 'NONE',  ( 764.8639956371174549, -392.0891481129648355, -319.7806653035542013 ) ) ;
#7167 = CIRCLE ( 'NONE', #23358, 2.749999999999891642 ) ;
#7168 = CARTESIAN_POINT ( 'NONE',  ( 765.8855110935204493, -46.16923265350568784, 319.0159684113471599 ) ) ;
#7169 = CARTESIAN_POINT ( 'NONE',  ( 748.3538107759620743, -88.71468719896009247, -355.8262568251490165 ) ) ;
#7170 = CARTESIAN_POINT ( 'NONE',  ( 749.8865473780648472, -188.5328690171416497, 322.1177392798429082 ) ) ;
#7171 = CARTESIAN_POINT ( 'NONE',  ( 754.8072714833583632, -28.81642084023863504, 338.1981804954721156 ) ) ;
#7172 = CARTESIAN_POINT ( 'NONE',  ( 773.3843516231979720, -373.4419599262319593, 364.4086373105754433 ) ) ;
#7173 = EDGE_LOOP ( 'NONE', ( #5274, #37675, #45424, #10452 ) ) ;
#7174 = CARTESIAN_POINT ( 'NONE',  ( 804.6798772138708955, -87.72551174932937101, -334.6312213355107019 ) ) ;
#7175 = CARTESIAN_POINT ( 'NONE',  ( 756.1348686366196716, -209.2601417444142839, -347.5531968255698416 ) ) ;
#7176 = CARTESIAN_POINT ( 'NONE',  ( 762.1405469898971887, -193.5436935675108714, 357.8594530101015607 ) ) ;
#7177 = CARTESIAN_POINT ( 'NONE',  ( 783.7566961878529810, -48.89650538077840025, -305.1792804349288417 ) ) ;
#7178 = CARTESIAN_POINT ( 'NONE',  ( 778.2165204200184689, -334.8164208402376403, 364.9363028652563230 ) ) ;
#7179 = VERTEX_POINT ( 'NONE', #43708 ) ;
#7180 = CARTESIAN_POINT ( 'NONE',  ( 772.3691319403857278, -47.26014174441477422, 315.8894580844506663 ) ) ;
#7182 = AXIS2_PLACEMENT_3D ( 'NONE', #28623, #31621, #42704 ) ;
#7181 = CARTESIAN_POINT ( 'NONE',  ( 757.7880784355613741, -306.0090635724252479, -312.4576283171834916 ) ) ;
#7183 = AXIS2_PLACEMENT_3D ( 'NONE', #4140, #22337, #15444 ) ;
#7184 = CARTESIAN_POINT ( 'NONE',  ( 747.2067596250078623, -243.1800572038743269, 352.2312462859687230 ) ) ;
#7185 = EDGE_CURVE ( 'NONE', #25647, #34950, #26391, .T. ) ;
#7186 = CARTESIAN_POINT ( 'NONE',  ( 813.2346286133761168, -5.260141744414903897, 328.9521613784389160 ) ) ;
#7187 = CARTESIAN_POINT ( 'NONE',  ( 766.0291762391763086, -154.9181544815165523, -360.7704444035551319 ) ) ;
#7188 = CARTESIAN_POINT ( 'NONE',  ( 797.8594530101008786, -133.5436935675110135, -322.1405469898980982 ) ) ;
#7189 = CARTESIAN_POINT ( 'NONE',  ( 755.0636971347428243, -340.2709662947831362, -341.7834795799807353 ) ) ;
#7190 = EDGE_LOOP ( 'NONE', ( #42020, #36578, #13036, #37313 ) ) ;
#7191 = AXIS2_PLACEMENT_3D ( 'NONE', #40056, #22718, #36812 ) ;
#7192 = CARTESIAN_POINT ( 'NONE',  ( 777.4774526936600978, -298.2709662947830793, 304.7301800767027657 ) ) ;
#7193 = LINE ( 'NONE', #35345, #4173 ) ;
#7194 = CARTESIAN_POINT ( 'NONE',  ( 795.9930595647434757, -339.0783235625956422, 320.7433823573372820 ) ) ;
#7195 = EDGE_CURVE ( 'NONE', #15686, #1155, #33545, .T. ) ;
#7196 = DIRECTION ( 'NONE',  ( 0.000000000000000000, 0.7071067811865501263, 0.7071067811865449082 ) ) ;
#7197 = EDGE_CURVE ( 'NONE', #40483, #21723, #6353, .T. ) ;
#7198 = CARTESIAN_POINT ( 'NONE',  ( 780.5236548040995785, -140.7363362996984506, 314.9735926884559944 ) ) ;
#7199 = CARTESIAN_POINT ( 'NONE',  ( 804.6798772138708955, -15.72551174932958951, 334.6312213355107019 ) ) ;
#7200 = ORIENTED_EDGE ( 'NONE', *, *, #39132, .F. ) ;
#7201 = CARTESIAN_POINT ( 'NONE',  ( 778.7629533639073998, -392.7363362996977116, -375.0009284576466371 ) ) ;
#7202 = CARTESIAN_POINT ( 'NONE',  ( 815.2698199232962679, -16.81642084023867412, -342.5225473063383674 ) ) ;
#7203 = CARTESIAN_POINT ( 'NONE',  ( 805.6418435158337843, -221.4636090269709428, 363.8556311672236916 ) ) ;
#7204 = CARTESIAN_POINT ( 'NONE',  ( 805.1016975059191054, -198.8965053807779384, 343.0745993439771837 ) ) ;
#7205 = CARTESIAN_POINT ( 'NONE',  ( 797.8594530101008786, -349.5436935675102745, -322.1405469898980982 ) ) ;
#7206 = CARTESIAN_POINT ( 'NONE',  ( 804.6971507214547046, -459.2817908451519884, 344.0799538623459739 ) ) ;
#7207 = CARTESIAN_POINT ( 'NONE',  ( 939.9999999999992042, 56.73212367640090292, 362.5753187112032947 ) ) ;
#7208 = CARTESIAN_POINT ( 'NONE',  ( 763.8424801807145741, -234.0090635724255037, -320.5453621957614700 ) ) ;
#7209 = CARTESIAN_POINT ( 'NONE',  ( 812.7932403749906598, -15.18005720387504631, 327.7687537140311633 ) ) ;
#7210 = CARTESIAN_POINT ( 'NONE',  ( 748.9653473494363425, -74.63460265842032015, 356.9462024416521331 ) ) ;
#7211 = LINE ( 'NONE', #21284, #10700 ) ;
#7212 = CARTESIAN_POINT ( 'NONE',  ( 787.5162901302840055, -419.3618753856918602, -305.4481719005793252 ) ) ;
#7213 = CARTESIAN_POINT ( 'NONE',  ( 187.1337867209877857, -179.7356316342496143, -69.11609595480014434 ) ) ;
#7214 = ADVANCED_FACE ( 'NONE', ( #26604 ), #44167, .T. ) ;
#7215 = CARTESIAN_POINT ( 'NONE',  ( 771.3260364891663130, -355.6454272087887603, 306.0683387631859773 ) ) ;
#7216 = EDGE_CURVE ( 'NONE', #3415, #14853, #16002, .T. ) ;
#7217 = DIRECTION ( 'NONE',  ( -1.000000000000000000, -0.000000000000000000, -0.000000000000000000 ) ) ;
#7218 = CARTESIAN_POINT ( 'NONE',  ( 755.2512626584698410, -319.5436935675104451, 315.2512626584710915 ) ) ;
#7219 = CARTESIAN_POINT ( 'NONE',  ( 759.0252816721024374, -48.99823902205675807, -368.0189434323527280 ) ) ;
#7220 = CARTESIAN_POINT ( 'NONE',  ( 756.5762568750052424, -267.1800572038742985, -348.7366044899774238 ) ) ;
#7221 = DIRECTION ( 'NONE',  ( -0.000000000000000000, -0.000000000000000000, 1.000000000000000000 ) ) ;
#7222 = APPLICATION_CONTEXT ( 'automotive_design' ) ;
#7223 = CARTESIAN_POINT ( 'NONE',  ( 788.7366044899766848, -419.9073299311465348, 316.5762568750059813 ) ) ;
#7224 = CARTESIAN_POINT ( 'NONE',  ( 759.0159684113467620, -184.9181544815165239, 325.8855110935213020 ) ) ;
#7225 = CARTESIAN_POINT ( 'NONE',  ( 776.2046728542105711, -20.19088175424429110, -304.8212110874238761 ) ) ;
#7226 = CARTESIAN_POINT ( 'NONE',  ( 769.1273215169530886, -70.71468719896014932, -317.4527132478988847 ) ) ;
#7227 = CARTESIAN_POINT ( 'NONE',  ( 744.8212110874229666, -114.8965053807782226, 336.2046728542121627 ) ) ;
#7228 = CARTESIAN_POINT ( 'NONE',  ( 755.0636971347428243, -412.2709662947829088, 341.7834795799807353 ) ) ;
#7229 = CIRCLE ( 'NONE', #2056, 18.00000000000001421 ) ;
#7230 = DIRECTION ( 'NONE',  ( 1.000000000000000000, 0.000000000000000000, 0.000000000000000000 ) ) ;
#7231 = CARTESIAN_POINT ( 'NONE',  ( 754.0944755984390895, -159.6237781080508285, 364.1009440267246760 ) ) ;
#7232 = CARTESIAN_POINT ( 'NONE',  ( 790.8050863131179540, -452.8379544210779954, 362.5841948692291226 ) ) ;
#7233 = EDGE_LOOP ( 'NONE', ( #6601, #4596 ) ) ;
#7234 = CARTESIAN_POINT ( 'NONE',  ( 778.1981804954714335, -106.2709662947838467, -314.8072714833589885 ) ) ;
#7235 = CARTESIAN_POINT ( 'NONE',  ( 756.7813123517142913, -403.9874144716863498, -329.9779781133712504 ) ) ;
#7237 = CARTESIAN_POINT ( 'NONE',  ( 755.0636971347428243, -220.2709662947834772, 341.7834795799807353 ) ) ;
#7236 = CARTESIAN_POINT ( 'NONE',  ( 804.9363028652555840, -232.2709662947834488, 338.2165204200192079 ) ) ;
#7238 = CARTESIAN_POINT ( 'NONE',  ( 773.7943932421234194, -407.8055962898681628, -305.5313806188329409 ) ) ;
#7239 = CARTESIAN_POINT ( 'NONE',  ( 751.9810565676468741, -2.089148112965993231, 360.9747183278973921 ) ) ;
#7240 = CARTESIAN_POINT ( 'NONE',  ( 799.9999999999993179, -512.9681489794448908, -370.0000000000000000 ) ) ;
#7241 = ORIENTED_EDGE ( 'NONE', *, *, #29695, .F. ) ;
#7242 = CARTESIAN_POINT ( 'NONE',  ( 756.5762568750052424, -411.1800572038738437, 348.7366044899774238 ) ) ;
#7243 = EDGE_CURVE ( 'NONE', #1813, #2103, #19916, .T. ) ;
#7244 = ORIENTED_EDGE ( 'NONE', *, *, #44042, .F. ) ;
#7245 = CARTESIAN_POINT ( 'NONE',  ( 815.2698199232961542, -256.8164208402379245, -342.5225473063383106 ) ) ;
#7246 = CARTESIAN_POINT ( 'NONE',  ( 808.3070685750232087, -162.9982390220563673, 361.1904061080339829 ) ) ;
#7247 = EDGE_CURVE ( 'NONE', #44144, #37112, #40704, .T. ) ;
#7248 = ORIENTED_EDGE ( 'NONE', *, *, #15570, .F. ) ;
#7249 = CARTESIAN_POINT ( 'NONE',  ( 778.7502325331095108, -192.3510508353233774, 304.6391490659818828 ) ) ;
#7250 = CARTESIAN_POINT ( 'NONE',  ( 794.9819416627830151, -252.9982390220560831, -319.9864689768909898 ) ) ;
#7251 = ORIENTED_EDGE ( 'NONE', *, *, #5182, .T. ) ;
#7252 = CARTESIAN_POINT ( 'NONE',  ( 756.5762568750052424, -363.1800572038739006, -348.7366044899774238 ) ) ;
#7253 = CARTESIAN_POINT ( 'NONE',  ( 755.5713283507202505, -29.36187538569318178, -334.6858677611754729 ) ) ;
#7254 = CARTESIAN_POINT ( 'NONE',  ( 775.9200461376533440, -239.8055962898687028, 315.3028492785443291 ) ) ;
#7255 = DIRECTION ( 'NONE',  ( 0.7071067811865753283, 0.000000000000000000, 0.7071067811865198172 ) ) ;
#7256 = CARTESIAN_POINT ( 'NONE',  ( 879.9999999999992042, 479.9999999999998863, 210.0000000000000000 ) ) ;
#7257 = ORIENTED_EDGE ( 'NONE', *, *, #34820, .F. ) ;
#7258 = CARTESIAN_POINT ( 'NONE',  ( 774.6858677611749044, -9.725511749329603717, -315.5713283507209894 ) ) ;
#7259 = CARTESIAN_POINT ( 'NONE',  ( -775.4999999999993179, -512.9681489794448908, -339.9999999999999432 ) ) ;
#7260 = DIRECTION ( 'NONE',  ( 0.000000000000000000, 0.000000000000000000, -1.000000000000000000 ) ) ;
#7261 = ORIENTED_EDGE ( 'NONE', *, *, #45035, .F. ) ;
#7262 = CARTESIAN_POINT ( 'NONE',  ( 748.6759233522253680, -280.3726999360616787, -324.3348316497537098 ) ) ;
#7263 = CARTESIAN_POINT ( 'NONE',  ( 778.7629533639073998, -152.7363362996983938, 375.0009284576466371 ) ) ;
#7264 = VECTOR ( 'NONE', #7403, 1000.000000000000000 ) ;
#7266 = CARTESIAN_POINT ( 'NONE',  ( 755.3201227861273992, -267.7255117493286320, -345.3687786644892981 ) ) ;
#7265 = DIRECTION ( 'NONE',  ( -0.000000000000000000, 1.000000000000000000, -0.000000000000000000 ) ) ;
#7267 = CARTESIAN_POINT ( 'NONE',  ( 802.7791456095903868, -388.7146871989592114, -329.0155153010375102 ) ) ;
#7268 = CARTESIAN_POINT ( 'NONE',  ( 879.9999999999990905, 479.9999999999998863, -199.9999999999999716 ) ) ;
#7269 = CARTESIAN_POINT ( 'NONE',  ( 760.7433823573367135, -132.0090635724257595, -355.9930595647440441 ) ) ;
#7270 = CARTESIAN_POINT ( 'NONE',  ( 762.1177392798416577, -378.5545181178795247, 309.8865473780659272 ) ) ;
#7271 = LINE ( 'NONE', #31275, #25431 ) ;
#7272 = CARTESIAN_POINT ( 'NONE',  ( 788.7631598425961101, -1.441959926233096656, -305.7194118038759143 ) ) ;
#7273 = CARTESIAN_POINT ( 'NONE',  ( 745.4481719005789273, -315.7255117493286320, -347.5162901302853697 ) ) ;
#7274 = CARTESIAN_POINT ( 'NONE',  ( 786.4999999999993179, -512.9681489794448908, -339.9999999999999432 ) ) ;
#7275 = CARTESIAN_POINT ( 'NONE',  ( 800.2193346964447755, -18.99823902205683979, 355.1360043628815788 ) ) ;
#7276 = CARTESIAN_POINT ( 'NONE',  ( 758.0580252608178853, -78.45278447660211896, -328.0187753319985404 ) ) ;
#7277 = CARTESIAN_POINT ( 'NONE',  ( 788.6739635108323228, -247.6454272087890160, 373.9316612368139090 ) ) ;
#7278 = CARTESIAN_POINT ( 'NONE',  ( 810.1134526219336749, -200.5328690171415644, -357.8822607201570349 ) ) ;
#7279 = CARTESIAN_POINT ( 'NONE',  ( 814.9108240113580450, -208.2709662947835341, 337.5031285880265273 ) ) ;
#7280 = CARTESIAN_POINT ( 'NONE',  ( 782.4968714119720516, -442.8164208402372992, -305.0891759886411023 ) ) ;
#7281 = DIRECTION ( 'NONE',  ( 0.000000000000000000, 0.000000000000000000, -1.000000000000000000 ) ) ;
#7282 = CARTESIAN_POINT ( 'NONE',  ( 754.8072714833581358, -340.8164208402376971, 338.1981804954720587 ) ) ;
#7283 = CARTESIAN_POINT ( 'NONE',  ( 800.9840315886518738, -76.91815448151683654, 354.1144889064786412 ) ) ;
#7284 = CARTESIAN_POINT ( 'NONE',  ( 756.1348686366196716, 6.739858255585061464, -347.5531968255698416 ) ) ;
#7285 = DIRECTION ( 'NONE',  ( 0.000000000000000000, 0.000000000000000000, 1.000000000000000000 ) ) ;
#7286 = CARTESIAN_POINT ( 'NONE',  ( 187.1337867209877857, -179.7356316342496143, 69.11609595480014434 ) ) ;
#7288 = CARTESIAN_POINT ( 'NONE',  ( 800.0135310231082713, -350.0891481129648923, 325.0180583372163028 ) ) ;
#7287 = CARTESIAN_POINT ( 'NONE',  ( 770.0799878456142551, -109.9874144716873019, 362.9823548866085616 ) ) ;
#7289 = ORIENTED_EDGE ( 'NONE', *, *, #5689, .T. ) ;
#7290 = CARTESIAN_POINT ( 'NONE',  ( 776.9566956441375396, -300.8965053807775689, -364.8461984189686405 ) ) ;
#7291 = CARTESIAN_POINT ( 'NONE',  ( 774.6858677611749044, -105.7255117493293000, 315.5713283507209894 ) ) ;
#7292 = CARTESIAN_POINT ( 'NONE',  ( 758.0141637701419768, -279.0783235625958127, -367.2620300519063790 ) ) ;
#7293 = DIRECTION ( 'NONE',  ( -0.000000000000000000, -0.000000000000000000, -1.000000000000000000 ) ) ;
#7294 = CARTESIAN_POINT ( 'NONE',  ( 810.1134526219336749, -416.5328690171409107, 357.8822607201570349 ) ) ;
#7295 = ORIENTED_EDGE ( 'NONE', *, *, #7452, .T. ) ;
#7296 = CARTESIAN_POINT ( 'NONE',  ( 771.2633955100217236, -311.9073299311468759, 363.4237431249939618 ) ) ;
#7297 = CARTESIAN_POINT ( 'NONE',  ( 799.4546378042377910, -57.07832356259658013, -356.1575198192848006 ) ) ;
#7298 = CARTESIAN_POINT ( 'NONE',  ( 794.9819416627830151, -156.9982390220564241, -319.9864689768909898 ) ) ;
#7299 = CARTESIAN_POINT ( 'NONE',  ( 758.0580252608178853, -222.4527844766016642, -328.0187753319985404 ) ) ;
#7300 = CARTESIAN_POINT ( 'NONE',  ( 756.5762568750052424, -411.1800572038738437, 348.7366044899774238 ) ) ;
#7301 = CARTESIAN_POINT ( 'NONE',  ( 763.2262854647970016, -152.6346026584200786, -309.2812353651462445 ) ) ;
#7302 = ORIENTED_EDGE ( 'NONE', *, *, #38540, .T. ) ;
#7303 = CARTESIAN_POINT ( 'NONE',  ( 756.3353852180820240, -125.9073299311474159, -331.1735550268787733 ) ) ;
#7304 = ORIENTED_EDGE ( 'NONE', *, *, #38557, .T. ) ;
#7305 = CARTESIAN_POINT ( 'NONE',  ( 758.4439275373578084, -396.5545181178794678, -353.2243759319684386 ) ) ;
#7307 = CARTESIAN_POINT ( 'NONE',  ( 769.0155153010367712, -442.3726999360611103, 362.7791456095907279 ) ) ;
#7306 = CARTESIAN_POINT ( 'NONE',  ( 804.9363028652555840, -136.2709662947837330, 338.2165204200192079 ) ) ;
#7308 = CARTESIAN_POINT ( 'NONE',  ( 799.4546378042377910, -129.0783235625963243, 356.1575198192848006 ) ) ;
#7311 = CARTESIAN_POINT ( 'NONE',  ( 815.1787889125755555, -390.8965053807772279, 343.7953271457877804 ) ) ;
#7310 = FACE_OUTER_BOUND ( 'NONE', #16254, .T. ) ;
#7309 = DIRECTION ( 'NONE',  ( 0.000000000000000000, 0.000000000000000000, -1.000000000000000000 ) ) ;
#7312 = EDGE_LOOP ( 'NONE', ( #17467, #34606 ) ) ;
#7313 = CARTESIAN_POINT ( 'NONE',  ( 784.1219089521767955, -405.2817908451522158, -315.0488828828318333 ) ) ;
#7314 = CARTESIAN_POINT ( 'NONE',  ( 774.6858677611749044, -369.7255117493284615, -315.5713283507209894 ) ) ;
#7315 = CARTESIAN_POINT ( 'NONE',  ( 771.3260364891663130, -163.6454272087893003, -306.0683387631859773 ) ) ;
#7316 = CARTESIAN_POINT ( 'NONE',  ( 747.6481478633932056, -37.09997266333514432, 353.4146539503763620 ) ) ;
#7318 = DIRECTION ( 'NONE',  ( -0.000000000000000000, -1.110223024625155554E-15, -1.000000000000000000 ) ) ;
#7317 = CARTESIAN_POINT ( 'NONE',  ( 989.9999999999992042, -590.0000000000001137, -360.0000000000000000 ) ) ;
#7319 = CARTESIAN_POINT ( 'NONE',  ( 770.0799878456142551, -301.9874144716867477, -362.9823548866085616 ) ) ;
#7320 = DIRECTION ( 'NONE',  ( 0.000000000000000000, 0.000000000000000000, 1.000000000000000000 ) ) ;
#7321 = CARTESIAN_POINT ( 'NONE',  ( 804.1009440267234822, -191.4636090269709996, -314.0944755984392600 ) ) ;
#7322 = CARTESIAN_POINT ( 'NONE',  ( 879.9999999999990905, 469.9999999999998863, -210.0000000000000000 ) ) ;
#7323 = DIRECTION ( 'NONE',  ( -0.000000000000000000, -0.000000000000000000, 1.000000000000000000 ) ) ;
#7324 = CARTESIAN_POINT ( 'NONE',  ( 763.0428371773158460, -371.4636090269705164, 358.7617431975195359 ) ) ;
#7325 = CARTESIAN_POINT ( 'NONE',  ( 773.7305795820266212, -321.2817908451525000, 374.8230680027170365 ) ) ;
#7326 = CARTESIAN_POINT ( 'NONE',  ( 796.7737145352015204, -212.6346026584198796, -370.7187646348536987 ) ) ;
#7327 = CARTESIAN_POINT ( 'NONE',  ( -598.8365100919716042, 230.0000000000001421, -202.7499999999898250 ) ) ;
#7328 = CARTESIAN_POINT ( 'NONE',  ( -769.9999999999992042, 205.0000000000000568, -339.9999999999999432 ) ) ;
#7329 = CARTESIAN_POINT ( 'NONE',  ( 757.7880784355613741, -162.0090635724256742, 312.4576283171834916 ) ) ;
#7330 = CARTESIAN_POINT ( 'NONE',  ( 810.1134526219336749, -80.53286901714194812, -357.8822607201570349 ) ) ;
#7331 = CARTESIAN_POINT ( 'NONE',  ( 755.2512626584698410, -103.5436935675111272, 315.2512626584710915 ) ) ;
#7332 = CARTESIAN_POINT ( 'NONE',  ( 804.7487373415286811, -355.5436935675103882, -364.7487373415288516 ) ) ;
#7333 = FACE_OUTER_BOUND ( 'NONE', #5754, .T. ) ;
#7334 = CARTESIAN_POINT ( 'NONE',  ( -728.8365100919714905, 260.0000000000001705, -199.9999999999890861 ) ) ;
#7335 = CARTESIAN_POINT ( 'NONE',  ( 762.3223304703356007, -175.5436935675108998, 322.3223304703362828 ) ) ;
#7336 = CARTESIAN_POINT ( 'NONE',  ( 804.8461984189677878, -2.190881754244347945, 336.9566956441385628 ) ) ;
#7337 = CARTESIAN_POINT ( 'NONE',  ( 746.0683387631852383, -427.4419599262317888, -331.3260364891676204 ) ) ;
#7338 = CARTESIAN_POINT ( 'NONE',  ( 745.7998596910086917, -437.3618753856919170, -332.5602148656461168 ) ) ;
#7339 = CARTESIAN_POINT ( 'NONE',  ( 911.9999999999993179, 154.9999999999998863, 360.0000000000000000 ) ) ;
#7340 = CARTESIAN_POINT ( 'NONE',  ( 814.8230680027162407, -5.805596289869448867, 333.7305795820267917 ) ) ;
#7341 = ORIENTED_EDGE ( 'NONE', *, *, #24465, .F. ) ;
#7342 = CARTESIAN_POINT ( 'NONE',  ( 744.9990715423526808, -186.3510508353234343, -341.2370466360926002 ) ) ;
#7343 = DIRECTION ( 'NONE',  ( -0.000000000000000000, -0.000000000000000000, 1.000000000000000000 ) ) ;
#7344 = CARTESIAN_POINT ( 'NONE',  ( 766.5853460496234675, -325.9874144716865771, 372.3518521366060554 ) ) ;
#7345 = CARTESIAN_POINT ( 'NONE',  ( 805.1927285166399315, -112.8164208402383650, 341.8018195045277707 ) ) ;
#7346 = VERTEX_POINT ( 'NONE', #19686 ) ;
#7347 = CARTESIAN_POINT ( 'NONE',  ( 759.7806653035534055, -318.9982390220557704, 324.8639956371180801 ) ) ;
#7348 = CARTESIAN_POINT ( 'NONE',  ( 754.9967657858570647, -49.54369356751129061, -365.0032342141425374 ) ) ;
#7349 = CARTESIAN_POINT ( 'NONE',  ( 748.9653473494365699, -98.63460265842023489, 356.9462024416520762 ) ) ;
#7350 = ORIENTED_EDGE ( 'NONE', *, *, #16570, .F. ) ;
#7351 = CARTESIAN_POINT ( 'NONE',  ( 815.3608509340175488, -458.7363362996973706, -341.2497674668889545 ) ) ;
#7352 = AXIS2_PLACEMENT_3D ( 'NONE', #44672, #23628, #9568 ) ;
#7353 = ORIENTED_EDGE ( 'NONE', *, *, #15376, .F. ) ;
#7354 = APPLICATION_PROTOCOL_DEFINITION ( 'draft international standard', 'automotive_design', 1998, #16041 ) ;
#7355 = CARTESIAN_POINT ( 'NONE',  ( 764.8639956371174549, -32.08914811296588709, 319.7806653035542013 ) ) ;
#7356 = CARTESIAN_POINT ( 'NONE',  ( 791.9812246680005501, -308.6346026584195670, -361.9419747391813189 ) ) ;
#7358 = CARTESIAN_POINT ( 'NONE',  ( 766.5853460496234675, -301.9874144716867477, 372.3518521366060554 ) ) ;
#7357 = CARTESIAN_POINT ( 'NONE',  ( 744.7301800767020268, -412.8164208402373561, 337.4774526936615189 ) ) ;
#7359 = CARTESIAN_POINT ( 'NONE',  ( 761.9338519418445230, -86.53286901714194812, 370.4231160770881957 ) ) ;
#7360 = CARTESIAN_POINT ( 'NONE',  ( 760.7433823573367135, -300.0090635724252479, -355.9930595647440441 ) ) ;
#7361 = CARTESIAN_POINT ( 'NONE',  ( 755.0636971347428243, -244.2709662947834204, -341.7834795799807353 ) ) ;
#7362 = CARTESIAN_POINT ( 'NONE',  ( 791.9812246680005501, -452.6346026584191691, -361.9419747391813189 ) ) ;
#7363 = CARTESIAN_POINT ( 'NONE',  ( 791.9812246680005501, -116.6346026584201780, -361.9419747391813189 ) ) ;
#7364 = DIRECTION ( 'NONE',  ( 0.000000000000000000, -0.9238795325112892920, 0.3826834323650836756 ) ) ;
#7365 = CARTESIAN_POINT ( 'NONE',  ( 813.1304606946830518, -401.9073299311463643, 352.3570229623690580 ) ) ;
#7367 = CARTESIAN_POINT ( 'NONE',  ( 789.9999999999992042, 205.0000000000000568, -360.0000000000000000 ) ) ;
#7366 = LINE ( 'NONE', #21217, #10792 ) ;
#7368 = CARTESIAN_POINT ( 'NONE',  ( 747.6481478633932056, -37.09997266333514432, -353.4146539503763620 ) ) ;
#7369 = DIRECTION ( 'NONE',  ( -1.000000000000000000, -0.000000000000000000, -0.000000000000000000 ) ) ;
#7370 = FACE_OUTER_BOUND ( 'NONE', #43640, .T. ) ;
#7371 = CARTESIAN_POINT ( 'NONE',  ( 776.9254006560222479, -260.1908817542435486, 314.8983024940802125 ) ) ;
#7372 = CARTESIAN_POINT ( 'NONE',  ( 788.8264449731200330, -165.1800572038745258, 363.6646147819171233 ) ) ;
#7373 = ORIENTED_EDGE ( 'NONE', *, *, #6505, .T. ) ;
#7374 = CARTESIAN_POINT ( 'NONE',  ( 773.4516893846965786, -19.64542720878974791, -315.8398074228977066 ) ) ;
#7375 = CARTESIAN_POINT ( 'NONE',  ( 801.1904061080338124, -92.08914811296570235, -368.3070685750236066 ) ) ;
#7376 = CARTESIAN_POINT ( 'NONE',  ( 758.6633372737375112, -308.5328690171412518, 326.9102291470432533 ) ) ;
#7377 = FACE_OUTER_BOUND ( 'NONE', #8364, .T. ) ;
#7378 = CARTESIAN_POINT ( 'NONE',  ( 778.7629533639073998, -32.73633629969879877, 375.0009284576466371 ) ) ;
#7379 = CARTESIAN_POINT ( 'NONE',  ( 767.6429770376289525, -225.1800572038743269, -306.8695393053162093 ) ) ;
#7380 = CARTESIAN_POINT ( 'NONE',  ( 796.7737145352015204, -212.6346026584198796, 370.7187646348536987 ) ) ;
#7381 = CARTESIAN_POINT ( 'NONE',  ( 765.0180583372156207, -72.99823902205667991, 360.0135310231089534 ) ) ;
#7382 = DIRECTION ( 'NONE',  ( 0.000000000000000000, -0.6755902076156505842, -0.7372773368101328550 ) ) ;
#7383 = CARTESIAN_POINT ( 'NONE',  ( 805.9055244015594326, -291.6237781080503169, -315.8990559732753240 ) ) ;
#7384 = CARTESIAN_POINT ( 'NONE',  ( 783.7953271457878373, -440.1908817542430370, 375.1787889125761239 ) ) ;
#7385 = CARTESIAN_POINT ( 'NONE',  ( 767.6429770376289525, -321.1800572038740142, -306.8695393053162093 ) ) ;
#7386 = DIRECTION ( 'NONE',  ( -1.000000000000000000, 0.000000000000000000, 0.000000000000000000 ) ) ;
#7387 = CARTESIAN_POINT ( 'NONE',  ( 766.7756240680305382, -374.5328690171410813, 361.5560724626415663 ) ) ;
#7388 = CARTESIAN_POINT ( 'NONE',  ( 755.2512626584698410, -31.54369356751135456, 315.2512626584710915 ) ) ;
#7389 = CARTESIAN_POINT ( 'NONE',  ( 791.9812246680005501, -404.6346026584193396, -361.9419747391813189 ) ) ;
#7390 = CARTESIAN_POINT ( 'NONE',  ( 761.2382568024794409, -63.62377810805107714, 356.9571628226838129 ) ) ;
#7391 = CARTESIAN_POINT ( 'NONE',  ( 797.8594530101008786, -205.5436935675108430, -322.1405469898980982 ) ) ;
#7393 = ADVANCED_FACE ( 'NONE', ( #41172, #44627 ), #44391, .F. ) ;
#7392 = CARTESIAN_POINT ( 'NONE',  ( 746.7653713866222915, -89.26014174441463922, -351.0478386215610271 ) ) ;
#7394 = CARTESIAN_POINT ( 'NONE',  ( 813.2346286133761168, -221.2601417444142271, 328.9521613784389160 ) ) ;
#7395 = CARTESIAN_POINT ( 'NONE',  ( 795.1360043628808398, -20.08914811296593328, 360.2193346964456282 ) ) ;
#7396 = EDGE_LOOP ( 'NONE', ( #39858, #16678, #2238, #24707 ) ) ;
#7397 = CARTESIAN_POINT ( 'NONE',  ( 758.6633372737375112, -188.5328690171416497, -326.9102291470432533 ) ) ;
#7398 = CARTESIAN_POINT ( 'NONE',  ( 778.1981804954714335, -202.2709662947834772, 314.8072714833589885 ) ) ;
#7399 = EDGE_CURVE ( 'NONE', #9202, #38196, #44623, .T. ) ;
#7400 = CARTESIAN_POINT ( 'NONE',  ( 746.7653713866222915, -17.26014174441486659, -351.0478386215610271 ) ) ;
#7401 = CARTESIAN_POINT ( 'NONE',  ( 758.0580252608178853, -318.4527844766014368, 328.0187753319985404 ) ) ;
#7402 = DIRECTION ( 'NONE',  ( -0.000000000000000000, -0.000000000000000000, 1.000000000000000000 ) ) ;
#7403 = DIRECTION ( 'NONE',  ( 0.000000000000000000, 0.000000000000000000, -1.000000000000000000 ) ) ;
#7404 = VERTEX_POINT ( 'NONE', #5831 ) ;
#7405 = CARTESIAN_POINT ( 'NONE',  ( 780.5290396650775619, -60.35105083532383219, 365.2837595273619513 ) ) ;
#7406 = CARTESIAN_POINT ( 'NONE',  ( 814.4686193811664907, -339.2817908451524431, -346.2056067578752732 ) ) ;
#7407 = CARTESIAN_POINT ( 'NONE',  ( 758.8095938919644823, -248.0891481129651766, 311.6929314249762797 ) ) ;
#7408 = CARTESIAN_POINT ( 'NONE',  ( 811.6461892240364477, -4.714687198960358039, 324.1737431748509835 ) ) ;
#7409 = CARTESIAN_POINT ( 'NONE',  ( 766.9102291470427417, -162.5545181178802352, -318.6633372737382501 ) ) ;
#7410 = CARTESIAN_POINT ( 'NONE',  ( 756.3353852180819104, -149.9073299311473875, -331.1735550268788302 ) ) ;
#7411 = CARTESIAN_POINT ( 'NONE',  ( 788.8264449731201466, -357.1800572038739574, -363.6646147819170665 ) ) ;
#7412 = ORIENTED_EDGE ( 'NONE', *, *, #28627, .T. ) ;
#7413 = CARTESIAN_POINT ( 'NONE',  ( 810.7187646348534145, -282.4527844766014937, 356.7737145352016341 ) ) ;
#7414 = CARTESIAN_POINT ( 'NONE',  ( 810.2700907235021077, -453.7763741861470521, 341.5253149289871999 ) ) ;
#7415 = CARTESIAN_POINT ( 'NONE',  ( 773.4516893846965786, -211.6454272087891582, 315.8398074228977066 ) ) ;
#7416 = CARTESIAN_POINT ( 'NONE',  ( 780.5290396650775619, -324.3510508353229511, 365.2837595273619513 ) ) ;
#7417 = FACE_BOUND ( 'NONE', #11138, .T. ) ;
#7418 = CARTESIAN_POINT ( 'NONE',  ( 804.4086373105744769, -169.6454272087892718, 333.3843516231986541 ) ) ;
#7419 = CARTESIAN_POINT ( 'NONE',  ( 755.0636971347428243, -28.27096629478409540, 341.7834795799807353 ) ) ;
#7420 = EDGE_CURVE ( 'NONE', #5430, #41190, #386, .T. ) ;
#7421 = ORIENTED_EDGE ( 'NONE', *, *, #24171, .F. ) ;
#7422 = CARTESIAN_POINT ( 'NONE',  ( 773.7305795820266212, -369.2817908451523294, -374.8230680027170365 ) ) ;
#7423 = CARTESIAN_POINT ( 'NONE',  ( 805.0032342141413437, -13.54369356751140963, -314.9967657858572352 ) ) ;
#7424 = CARTESIAN_POINT ( 'NONE',  ( 795.8262568251477660, -262.3726999360617924, 308.3538107759623585 ) ) ;
#7425 = CARTESIAN_POINT ( 'NONE',  ( 780.5290396650775619, -204.3510508353233774, 365.2837595273619513 ) ) ;
#7426 = CARTESIAN_POINT ( 'NONE',  ( 785.3687786644884454, -347.3618753856922012, -315.3201227861279676 ) ) ;
#7427 = CARTESIAN_POINT ( 'NONE',  ( 804.4086373105744769, -457.6454272087884760, 333.3843516231986541 ) ) ;
#7428 = CARTESIAN_POINT ( 'NONE',  ( 799.9999999999993179, -462.9681489794448339, -309.9999999999998863 ) ) ;
#7429 = CARTESIAN_POINT ( 'NONE',  ( 779.4763451958990572, -224.7363362996982232, -365.0264073115438919 ) ) ;
#7430 = CARTESIAN_POINT ( 'NONE',  ( 792.3570229623688874, -21.18005720387502677, 373.1304606946836202 ) ) ;
#7431 = CARTESIAN_POINT ( 'NONE',  ( 751.9810565676468741, -74.08914811296577341, 360.9747183278973921 ) ) ;
#7432 = CARTESIAN_POINT ( 'NONE',  ( -809.9999999999993179, -512.9681489794448908, -350.0000000000000000 ) ) ;
#7433 = CARTESIAN_POINT ( 'NONE',  ( 772.4837098697145166, -431.3618753856918602, -374.5518280994205611 ) ) ;
#7434 = CARTESIAN_POINT ( 'NONE',  ( -468.8365100919714337, 260.0000000000001705, -199.9999999999908766 ) ) ;
#7435 = CARTESIAN_POINT ( 'NONE',  ( 783.7953271457878373, -368.1908817542433212, 375.1787889125761239 ) ) ;
#7436 = CARTESIAN_POINT ( 'NONE',  ( 759.9999999999992042, 205.0000000000000568, -350.0000000000000000 ) ) ;
#7437 = CARTESIAN_POINT ( 'NONE',  ( 792.2312462859673587, -323.9073299311468190, 307.2067596250082602 ) ) ;
#7438 = CARTESIAN_POINT ( 'NONE',  ( 810.7187646348534145, -66.45278447660216159, -356.7737145352016341 ) ) ;
#7439 = CARTESIAN_POINT ( 'NONE',  ( 765.0180583372156207, -288.9982390220559978, -360.0135310231089534 ) ) ;
#7440 = EDGE_CURVE ( 'NONE', #23506, #11791, #29629, .T. ) ;
#7441 = CARTESIAN_POINT ( 'NONE',  ( 799.9999999999993179, 205.0000000000000568, -339.9999999999999432 ) ) ;
#7442 = CARTESIAN_POINT ( 'NONE',  ( 791.9812246680005501, -428.6346026584192259, 361.9419747391813189 ) ) ;
#7443 = CARTESIAN_POINT ( 'NONE',  ( 783.0745993439762742, -176.1908817542438328, 365.1016975059196739 ) ) ;
#7444 = CARTESIAN_POINT ( 'NONE',  ( 778.7629533639073998, -56.73633629969872771, -375.0009284576466371 ) ) ;
#7445 = CARTESIAN_POINT ( 'NONE',  ( 779.4709603349208464, -72.35105083532378956, -314.7162404726379918 ) ) ;
#7446 = CARTESIAN_POINT ( 'NONE',  ( 815.1787889125755555, -102.8965053807782368, 343.7953271457877804 ) ) ;
#7447 = CARTESIAN_POINT ( 'NONE',  ( 794.9819416627830151, -396.9982390220556567, 319.9864689768909898 ) ) ;
#7448 = CARTESIAN_POINT ( 'NONE',  ( 813.9316612368132837, -151.4419599262326415, 348.6739635108323228 ) ) ;
#7449 = CARTESIAN_POINT ( 'NONE',  ( 794.9819416627830151, 11.00176097794305541, -319.9864689768909898 ) ) ;
#7450 = EDGE_LOOP ( 'NONE', ( #23019, #42379, #13587, #39320 ) ) ;
#7451 = CARTESIAN_POINT ( 'NONE',  ( 785.3687786644884454, -83.36187538569296862, -315.3201227861279676 ) ) ;
#7452 = EDGE_CURVE ( 'NONE', #22109, #23565, #13906, .T. ) ;
#7453 = CARTESIAN_POINT ( 'NONE',  ( 780.5290396650775619, -396.3510508353228374, -365.2837595273619513 ) ) ;
#7455 = CARTESIAN_POINT ( 'NONE',  ( 800.2193346964446619, -210.9982390220562252, 355.1360043628816925 ) ) ;
#7454 = CARTESIAN_POINT ( 'NONE',  ( 797.6776695296629214, -235.5436935675107293, 357.6776695296636603 ) ) ;
#7456 = ORIENTED_EDGE ( 'NONE', *, *, #3842, .T. ) ;
#7457 = CARTESIAN_POINT ( 'NONE',  ( 815.1787889125755555, -414.8965053807771710, -343.7953271457877804 ) ) ;
#7458 = DIRECTION ( 'NONE',  ( -0.000000000000000000, 1.000000000000000000, -0.000000000000000000 ) ) ;
#7459 = ORIENTED_EDGE ( 'NONE', *, *, #16727, .F. ) ;
#7460 = CARTESIAN_POINT ( 'NONE',  ( 781.7834795799800531, -418.8164208402374129, 315.0636971347436202 ) ) ;
#7461 = EDGE_LOOP ( 'NONE', ( #36375, #36614, #41484, #42094 ) ) ;
#7462 = CARTESIAN_POINT ( 'NONE',  ( 749.2812353651451076, -246.4527844766016074, -323.2262854647983090 ) ) ;
#7463 = CARTESIAN_POINT ( 'NONE',  ( 759.0252816721024374, -144.9982390220564525, 368.0189434323527280 ) ) ;
#7464 = CARTESIAN_POINT ( 'NONE',  ( 790.9844846989617508, -262.3726999360617924, 317.2208543904092721 ) ) ;
#7465 = CARTESIAN_POINT ( 'NONE',  ( 756.7813123517142913, -379.9874144716865203, 329.9779781133712504 ) ) ;
#7466 = EDGE_LOOP ( 'NONE', ( #21881, #31490, #16621, #44658, #25867, #3116, #13071 ) ) ;
#7467 = CARTESIAN_POINT ( 'NONE',  ( 763.8424801807145741, -42.00906357242603661, -320.5453621957614700 ) ) ;
#7468 = CARTESIAN_POINT ( 'NONE',  ( 778.2165204200184689, -262.8164208402379245, -364.9363028652563230 ) ) ;
#7469 = VERTEX_POINT ( 'NONE', #28202 ) ;
#7470 = EDGE_CURVE ( 'NONE', #38419, #21828, #42689, .T. ) ;
#7471 = CARTESIAN_POINT ( 'NONE',  ( 800.0135310231082713, -374.0891481129647786, -325.0180583372163028 ) ) ;
#7472 = CARTESIAN_POINT ( 'NONE',  ( 794.9819416627830151, -12.99823902205686821, -319.9864689768909898 ) ) ;
#7473 = EDGE_CURVE ( 'NONE', #12764, #32851, #24501, .T. ) ;
#7474 = CARTESIAN_POINT ( 'NONE',  ( 804.9511171171677688, -221.8055962898687881, 335.8780910478229202 ) ) ;
#7475 = LINE ( 'NONE', #35627, #27014 ) ;
#7476 = CARTESIAN_POINT ( 'NONE',  ( 794.9999999999993179, 239.9999999999998863, -235.0000000000000000 ) ) ;
#7477 = PRODUCT_DEFINITION_SHAPE ( 'NONE', 'NONE',  #39755 ) ;
#7478 = VERTEX_POINT ( 'NONE', #31452 ) ;
#7479 = CARTESIAN_POINT ( 'NONE',  ( 785.3141322388236176, -21.72551174932956641, -364.4286716492789537 ) ) ;
#7480 = DIRECTION ( 'NONE',  ( 0.9164815115825496461, 0.1263042864341401839, 0.3796167358741286413 ) ) ;
#7481 = CARTESIAN_POINT ( 'NONE',  ( -786.4999999999993179, -544.8427095258973623, -350.0000000000000000 ) ) ;
#7482 = ORIENTED_EDGE ( 'NONE', *, *, #43367, .T. ) ;
#7483 = CARTESIAN_POINT ( 'NONE',  ( 762.1177392798416577, -282.5545181178798657, -309.8865473780659272 ) ) ;
#7484 = CARTESIAN_POINT ( 'NONE',  ( 754.3581564841646241, -137.4636090269711985, 316.1443688327762516 ) ) ;
#7486 = CARTESIAN_POINT ( 'NONE',  ( 764.8639956371174549, -272.0891481129651197, -319.7806653035542013 ) ) ;
#7485 = CARTESIAN_POINT ( 'NONE',  ( 829.9999999999992042, 430.0000000000002842, -320.0000000000000568 ) ) ;
#7487 = CARTESIAN_POINT ( 'NONE',  ( 914.9999999999990905, 469.9999999999999432, -350.0000000000000000 ) ) ;
#7488 = CARTESIAN_POINT ( 'NONE',  ( 755.1538015810308480, -134.1908817542439181, -343.0433043558613804 ) ) ;
#7489 = DIRECTION ( 'NONE',  ( 0.000000000000000000, 0.000000000000000000, 1.000000000000000000 ) ) ;
#7490 = CARTESIAN_POINT ( 'NONE',  ( 776.2433038121456548, 11.10349461922141145, -374.8207195650711014 ) ) ;
#7491 = CARTESIAN_POINT ( 'NONE',  ( 811.0346526505617248, -326.6346026584194533, -323.0537975583478101 ) ) ;
#7492 = CARTESIAN_POINT ( 'NONE',  ( -208.8365100919714052, 258.0940000000001078, -199.9999999999926956 ) ) ;
#7493 = CARTESIAN_POINT ( 'NONE',  ( 785.3141322388236176, 2.274488250670355871, 364.4286716492789537 ) ) ;
#7494 = EDGE_CURVE ( 'NONE', #36773, #31071, #3044, .T. ) ;
#7495 = CARTESIAN_POINT ( 'NONE',  ( 747.6481478633932056, -253.0999726633345119, 353.4146539503763620 ) ) ;
#7496 = CARTESIAN_POINT ( 'NONE',  ( 807.5423716828161105, -201.0783235625961254, -362.2119215644372048 ) ) ;
#7497 = CARTESIAN_POINT ( 'NONE',  ( 813.1304606946830518, -233.9073299311470180, 352.3570229623690580 ) ) ;
#7498 = CARTESIAN_POINT ( 'NONE',  ( 792.3570229623688874, -429.1800572038737869, -373.1304606946836202 ) ) ;
#7499 = DIRECTION ( 'NONE',  ( 1.000000000000000000, 0.000000000000000000, 0.000000000000000000 ) ) ;
#7500 = EDGE_CURVE ( 'NONE', #31261, #22826, #5540, .T. ) ;
#7501 = CARTESIAN_POINT ( 'NONE',  ( 759.9864689768902508, -314.0891481129650629, 354.9819416627836404 ) ) ;
#7502 = CARTESIAN_POINT ( 'NONE',  ( 798.5707757039680246, -101.4636090269713264, 356.7845633553585003 ) ) ;
#7503 = CARTESIAN_POINT ( 'NONE',  ( 790.0220218866281812, -103.0999726633349525, 363.2186876482849129 ) ) ;
#7504 = CARTESIAN_POINT ( 'NONE',  ( 804.6798772138708955, -447.7255117493280636, -334.6312213355107019 ) ) ;
#7505 = DIRECTION ( 'NONE',  ( -1.000000000000000000, 1.880165489482579047E-16, 0.000000000000000000 ) ) ;
#7506 = LINE ( 'NONE', #21578, #15912 ) ;
#7508 = CARTESIAN_POINT ( 'NONE',  ( 762.3223304703356007, -343.5436935675103314, 322.3223304703362828 ) ) ;
#7507 = CARTESIAN_POINT ( 'NONE',  ( 784.0799538623451781, -155.8055962898689586, 364.6971507214555572 ) ) ;
#7509 = ORIENTED_EDGE ( 'NONE', *, *, #16501, .F. ) ;
#7510 = EDGE_CURVE ( 'NONE', #3427, #33397, #40218, .T. ) ;
#7511 = CARTESIAN_POINT ( 'NONE',  ( 801.3366627262608972, -296.5328690171411949, -353.0897708529566899 ) ) ;
#7512 = CARTESIAN_POINT ( 'NONE',  ( 785.3141322388236176, -117.7255117493292715, 364.4286716492789537 ) ) ;
#7513 = CARTESIAN_POINT ( 'NONE',  ( 761.9338519418445230, -302.5328690171411949, -370.4231160770881957 ) ) ;
#7514 = DIRECTION ( 'NONE',  ( -1.000000000000000000, -0.000000000000000000, -0.000000000000000000 ) ) ;
#7515 = CARTESIAN_POINT ( 'NONE',  ( 768.8385539511368734, -431.2601417444136018, 306.4236121716840557 ) ) ;
#7516 = ORIENTED_EDGE ( 'NONE', *, *, #1182, .T. ) ;
#7517 = CARTESIAN_POINT ( 'NONE',  ( 755.3201227861273992, -315.7255117493286320, 345.3687786644892981 ) ) ;
#7518 = CARTESIAN_POINT ( 'NONE',  ( 758.6633372737375112, -92.53286901714190549, -326.9102291470432533 ) ) ;
#7519 = CARTESIAN_POINT ( 'NONE',  ( 754.8072714833581358, -148.8164208402382656, -338.1981804954720587 ) ) ;
#7520 = CARTESIAN_POINT ( 'NONE',  ( 805.1927285166397041, -208.8164208402380666, -341.8018195045277707 ) ) ;
#7521 = CARTESIAN_POINT ( 'NONE',  ( 756.3353852180819104, -413.9073299311465348, 331.1735550268788302 ) ) ;
#7522 = CARTESIAN_POINT ( 'NONE',  ( 814.2001403089898304, -161.3618753856927697, -347.4397851343538264 ) ) ;
#7523 = ORIENTED_EDGE ( 'NONE', *, *, #23757, .F. ) ;
#7524 = COLOUR_RGB ( '',0.7921568627450980005, 0.8196078431372548767, 0.9333333333333333481 ) ;
#7525 = CARTESIAN_POINT ( 'NONE',  ( 754.8072714833583632, -148.8164208402382656, -338.1981804954721156 ) ) ;
#7526 = EDGE_LOOP ( 'NONE', ( #44778, #13250, #12647, #22491 ) ) ;
#7527 = CARTESIAN_POINT ( 'NONE',  ( 793.9708237608222134, -406.9181544815157849, -319.2295555964448681 ) ) ;
#7528 = CARTESIAN_POINT ( 'NONE',  ( 757.0176451133909268, -445.0999726633338582, 349.9200121543848354 ) ) ;
#7529 = CARTESIAN_POINT ( 'NONE',  ( 763.2154366446407039, -141.6237781080508569, 321.4292242960311228 ) ) ;
#7532 = CARTESIAN_POINT ( 'NONE',  ( 805.9055244015594326, -387.6237781080499758, 315.8990559732753240 ) ) ;
#7531 = DIRECTION ( 'NONE',  ( -0.000000000000000000, 1.000000000000000000, 6.938893903907241197E-16 ) ) ;
#7530 = DIRECTION ( 'NONE',  ( 0.000000000000000000, 0.000000000000000000, -1.000000000000000000 ) ) ;
#7533 = ORIENTED_EDGE ( 'NONE', *, *, #18143, .F. ) ;
#7534 = CARTESIAN_POINT ( 'NONE',  ( 793.9708237608222134, -382.9181544815159555, -319.2295555964448681 ) ) ;
#7535 = DIRECTION ( 'NONE',  ( -1.000000000000000000, -0.000000000000000000, -0.000000000000000000 ) ) ;
#7536 = CARTESIAN_POINT ( 'NONE',  ( 746.4236121716829757, -183.8272453906074020, -328.8385539511384650 ) ) ;
#7537 = CARTESIAN_POINT ( 'NONE',  ( 813.5763878283155464, -27.82724539060790292, 351.1614460488615350 ) ) ;
#7539 = CARTESIAN_POINT ( 'NONE',  ( 787.4999999999992042, -462.9681489794447771, -310.9526249034443026 ) ) ;
#7538 = FACE_OUTER_BOUND ( 'NONE', #9091, .T. ) ;
#7540 = CARTESIAN_POINT ( 'NONE',  ( 754.9735926884551418, -306.3510508353230648, -340.5236548041000333 ) ) ;
#7541 = CARTESIAN_POINT ( 'NONE',  ( 187.1337867209877857, -422.8782571739196783, 207.4246812887968190 ) ) ;
#7542 = CARTESIAN_POINT ( 'NONE',  ( 766.4474001241216001, -187.0999726633346825, -307.3154664389482491 ) ) ;
#7543 = DIRECTION ( 'NONE',  ( 0.000000000000000000, 0.000000000000000000, 1.000000000000000000 ) ) ;
#7544 = DIRECTION ( 'NONE',  ( -1.000000000000000000, -8.326672684688676025E-16, 0.000000000000000000 ) ) ;
#7545 = CARTESIAN_POINT ( 'NONE',  ( 772.4468031744293057, -369.8272453906068904, 363.8651313633793620 ) ) ;
#7546 = CARTESIAN_POINT ( 'NONE',  ( 744.6391490659812007, -326.7363362996979390, 338.7502325331110455 ) ) ;
#7547 = CARTESIAN_POINT ( 'NONE',  ( 755.2512626584698410, -223.5436935675107577, -315.2512626584710915 ) ) ;
#7548 = PLANE ( 'NONE',  #29072 ) ;
#7549 = CARTESIAN_POINT ( 'NONE',  ( 764.8639956371174549, 15.91085188703394238, -319.7806653035542013 ) ) ;
#7550 = EDGE_CURVE ( 'NONE', #10866, #11865, #2578, .T. ) ;
#7551 = CARTESIAN_POINT ( 'NONE',  ( 744.6391490659812007, -158.7363362996984222, 338.7502325331110455 ) ) ;
#7552 = CARTESIAN_POINT ( 'NONE',  ( 803.8556311672234642, -81.62377810805104161, -365.6418435158340117 ) ) ;
#7553 = CARTESIAN_POINT ( 'NONE',  ( 808.3070685750230950, -114.9982390220565236, 361.1904061080339261 ) ) ;
#7554 = CARTESIAN_POINT ( 'NONE',  ( 801.1904061080336987, -356.0891481129647218, -368.3070685750235498 ) ) ;
#7555 = PLANE ( 'NONE',  #29280 ) ;
#7556 = DIRECTION ( 'NONE',  ( -1.084653538143406060E-16, 0.6594541114781790059, -0.7517448203044204691 ) ) ;
#7557 = CARTESIAN_POINT ( 'NONE',  ( 788.7366044899766848, -203.9073299311471885, 316.5762568750059813 ) ) ;
#7558 = VECTOR ( 'NONE', #34734, 1000.000000000000000 ) ;
#7559 = CARTESIAN_POINT ( 'NONE',  ( 802.5472867521000353, -4.372699936062523385, 350.8726784830461156 ) ) ;
#7560 = CARTESIAN_POINT ( 'NONE',  ( 748.3538107759620743, -400.7146871989590977, -355.8262568251490165 ) ) ;
#7561 = CARTESIAN_POINT ( 'NONE',  ( 744.7301800767019131, -412.8164208402372992, -337.4774526936615757 ) ) ;
#7562 = DIRECTION ( 'NONE',  ( 0.000000000000000000, 0.000000000000000000, 1.000000000000000000 ) ) ;
#7563 = CARTESIAN_POINT ( 'NONE',  ( 803.8556311672234642, 14.37622189194867417, 365.6418435158340117 ) ) ;
#7564 = ORIENTED_EDGE ( 'NONE', *, *, #41585, .F. ) ;
#7565 = CARTESIAN_POINT ( 'NONE',  ( 791.9812246680005501, -20.63460265842048003, 361.9419747391813189 ) ) ;
#7566 = CARTESIAN_POINT ( 'NONE',  ( 745.1769319972822814, -185.8055962898689302, -346.2694204179732083 ) ) ;
#7567 = CARTESIAN_POINT ( 'NONE',  ( 998.9999999999992042, 249.9999999999998863, 360.0000000000000000 ) ) ;
#7568 = CARTESIAN_POINT ( 'NONE',  ( 791.1614460488616487, -299.2601417444139997, 373.5763878283158874 ) ) ;
#7569 = CARTESIAN_POINT ( 'NONE',  ( 756.3353852180820240, -149.9073299311473875, 331.1735550268787733 ) ) ;
#7570 = ORIENTED_EDGE ( 'NONE', *, *, #15389, .T. ) ;
#7571 = CARTESIAN_POINT ( 'NONE',  ( 754.8072714833581358, -292.8164208402376971, 338.1981804954720587 ) ) ;
#7572 = CARTESIAN_POINT ( 'NONE',  ( 746.8695393053150156, -29.90732993114771787, -327.6429770376306010 ) ) ;
#7573 = AXIS2_PLACEMENT_3D ( 'NONE', #34573, #37575, #33658 ) ;
#7574 = CARTESIAN_POINT ( 'NONE',  ( 777.5031285880264704, -70.81642084023850714, 374.9108240113588408 ) ) ;
#7575 = VERTEX_POINT ( 'NONE', #37695 ) ;
#7576 = CARTESIAN_POINT ( 'NONE',  ( 814.8207195650702488, -458.1908817542429802, -336.2433038121456548 ) ) ;
#7577 = ORIENTED_EDGE ( 'NONE', *, *, #22046, .F. ) ;
#7578 = APPLICATION_PROTOCOL_DEFINITION ( 'draft international standard', 'automotive_design', 1998, #23707 ) ;
#7579 = CARTESIAN_POINT ( 'NONE',  ( 794.9819416627830151, -36.99823902205679360, 319.9864689768909898 ) ) ;
#7580 = CARTESIAN_POINT ( 'NONE',  ( 754.8072714833581358, -292.8164208402376971, -338.1981804954720587 ) ) ;
#7582 = CARTESIAN_POINT ( 'NONE',  ( 781.2497674668890113, -276.3510508353231785, 375.3608509340180603 ) ) ;
#7581 = CARTESIAN_POINT ( 'NONE',  ( 792.3570229623691148, -405.1800572038737869, 373.1304606946836770 ) ) ;
#7583 = CARTESIAN_POINT ( 'NONE',  ( 768.8385539511368734, -71.26014174441469606, 306.4236121716840557 ) ) ;
#7584 = CARTESIAN_POINT ( 'NONE',  ( 757.0176451133909268, -277.0999726633344267, -349.9200121543848354 ) ) ;
#7585 = CARTESIAN_POINT ( 'NONE',  ( 804.6798772138708955, -303.7255117493287457, -334.6312213355107019 ) ) ;
#7586 = CARTESIAN_POINT ( 'NONE',  ( 791.0208441182601291, -452.8006503659887585, -362.4663821942984328 ) ) ;
#7587 = CARTESIAN_POINT ( 'NONE',  ( 797.8594530101008786, -133.5436935675110135, -322.1405469898980982 ) ) ;
#7588 = CARTESIAN_POINT ( 'NONE',  ( 879.9999999999992042, 469.9999999999998863, -210.0000000000000000 ) ) ;
#7589 = CARTESIAN_POINT ( 'NONE',  ( 746.8695393053150156, -389.9073299311465348, 327.6429770376306010 ) ) ;
#7591 = LINE ( 'NONE', #1105, #27781 ) ;
#7590 = LINE ( 'NONE', #26493, #27788 ) ;
#7592 = CARTESIAN_POINT ( 'NONE',  ( 809.0717654672305343, -76.91815448151683654, -360.1688906516309885 ) ) ;
#7593 = LINE ( 'NONE', #27687, #18246 ) ;
#7594 = FACE_OUTER_BOUND ( 'NONE', #11213, .T. ) ;
#7595 = CARTESIAN_POINT ( 'NONE',  ( 769.0155153010367712, -250.3726999360618208, 362.7791456095907279 ) ) ;
#7596 = CARTESIAN_POINT ( 'NONE',  ( 756.5762568750052424, -147.1800572038746395, 348.7366044899774238 ) ) ;
#7597 = ORIENTED_EDGE ( 'NONE', *, *, #29470, .F. ) ;
#7598 = CARTESIAN_POINT ( 'NONE',  ( 757.0176451133909268, -37.09997266333514432, -349.9200121543848354 ) ) ;
#7599 = CARTESIAN_POINT ( 'NONE',  ( 777.5031285880264704, -118.8164208402383508, -374.9108240113588408 ) ) ;
#7600 = CARTESIAN_POINT ( 'NONE',  ( 798.7617431975189675, -339.6237781080502600, 323.0428371773161871 ) ) ;
#7601 = CARTESIAN_POINT ( 'NONE',  ( 914.9999999999992042, 99.99999999999984368, 360.0000000000000000 ) ) ;
#7602 = CARTESIAN_POINT ( 'NONE',  ( 773.7305795820266212, -33.28179084515333130, 374.8230680027170365 ) ) ;
#7603 = CARTESIAN_POINT ( 'NONE',  ( 800.9747183278959710, -228.9982390220561683, -311.9810565676471583 ) ) ;
#7604 = CARTESIAN_POINT ( 'NONE',  ( 748.9653473494363425, -194.6346026584198796, 356.9462024416521331 ) ) ;
#7605 = CARTESIAN_POINT ( 'NONE',  ( 805.1927285166397041, -112.8164208402383508, 341.8018195045277707 ) ) ;
#7606 = VECTOR ( 'NONE', #37984, 1000.000000000000000 ) ;
#7607 = CARTESIAN_POINT ( 'NONE',  ( 766.5853460496234675, -301.9874144716867477, -372.3518521366060554 ) ) ;
#7608 =( GEOMETRIC_REPRESENTATION_CONTEXT ( 3 ) GLOBAL_UNCERTAINTY_ASSIGNED_CONTEXT ( ( #45520 ) ) GLOBAL_UNIT_ASSIGNED_CONTEXT ( ( #36091, #25692, #4668 ) ) REPRESENTATION_CONTEXT ( 'NONE', 'WORKASPACE' ) );
#7609 = CARTESIAN_POINT ( 'NONE',  ( 814.8207195650702488, -458.1908817542429802, 336.2433038121456548 ) ) ;
#7610 = CARTESIAN_POINT ( 'NONE',  ( 755.2512626584698410, -319.5436935675104451, -315.2512626584710915 ) ) ;
#7611 = CARTESIAN_POINT ( 'NONE',  ( 265.7583438952258916, 290.0000000000001137, -320.0000000000000568 ) ) ;
#7612 = CARTESIAN_POINT ( 'NONE',  ( 755.0488828828309806, -377.8055962898682765, 344.1219089521771934 ) ) ;
#7613 = CARTESIAN_POINT ( 'NONE',  ( 812.7932403749906598, -63.18005720387488822, 327.7687537140311633 ) ) ;
#7614 = CARTESIAN_POINT ( 'NONE',  ( 778.2165204200184689, -406.8164208402375266, -364.9363028652563230 ) ) ;
#7615 = CARTESIAN_POINT ( 'NONE',  ( 803.8651313633788504, -53.26014174441475291, 332.4468031744301015 ) ) ;
#7616 = CARTESIAN_POINT ( 'NONE',  ( 755.3201227861273992, -195.7255117493289731, -345.3687786644892981 ) ) ;
#7617 = CARTESIAN_POINT ( 'NONE',  ( 810.1134526219336749, -80.53286901714194812, -357.8822607201570349 ) ) ;
#7618 = CARTESIAN_POINT ( 'NONE',  ( 783.7566961878529810, -216.8965053807778816, 305.1792804349288417 ) ) ;
#7619 = CARTESIAN_POINT ( 'NONE',  ( 778.1981804954715471, -10.27096629478415046, 314.8072714833591021 ) ) ;
#7620 = ORIENTED_EDGE ( 'NONE', *, *, #8626, .T. ) ;
#7621 = CARTESIAN_POINT ( 'NONE',  ( 755.8398074228967971, -211.4419599262324709, -333.4516893846970333 ) ) ;
#7622 = CARTESIAN_POINT ( 'NONE',  ( 764.8639956371174549, -200.0891481129653187, 319.7806653035542013 ) ) ;
#7623 = CARTESIAN_POINT ( 'NONE',  ( 773.7943932421234194, -23.80559628986938847, -305.5313806188329409 ) ) ;
#7624 = CARTESIAN_POINT ( 'NONE',  ( 804.6798772138710092, -327.7255117493285752, 334.6312213355106451 ) ) ;
#7625 = CARTESIAN_POINT ( 'NONE',  ( 801.0087853405226497, -452.9681489794447202, -354.4092604580203556 ) ) ;
#7626 = CARTESIAN_POINT ( 'NONE',  ( 998.9999999999992042, 479.9999999999998863, 199.9999999999999716 ) ) ;
#7627 = VERTEX_POINT ( 'NONE', #2822 ) ;
#7628 = CARTESIAN_POINT ( 'NONE',  ( 783.0433043558608688, -48.89650538077840025, 315.1538015810313027 ) ) ;
#7629 = CARTESIAN_POINT ( 'NONE',  ( 745.5313806188320314, -327.2817908451525000, -333.7943932421247268 ) ) ;
#7630 = CARTESIAN_POINT ( 'NONE',  ( 763.2262854647970016, -296.6346026584195670, 309.2812353651462445 ) ) ;
#7631 = CARTESIAN_POINT ( 'NONE',  ( 813.9316612368132837, -7.441959926233078448, 348.6739635108323228 ) ) ;
#7632 = CARTESIAN_POINT ( 'NONE',  ( 755.3028492785439312, -183.2817908451528695, -335.9200461376539693 ) ) ;
#7633 = CARTESIAN_POINT ( 'NONE',  ( 755.0636971347428243, -172.2709662947836478, -341.7834795799807353 ) ) ;
#7634 = VECTOR ( 'NONE', #10539, 1000.000000000000000 ) ;
#7635 = CARTESIAN_POINT ( 'NONE',  ( 771.1735550268780344, -345.1800572038739574, -316.3353852180828198 ) ) ;
#7636 = EDGE_LOOP ( 'NONE', ( #35810, #25110 ) ) ;
#7637 = CIRCLE ( 'NONE', #23100, 30.00000000000002842 ) ;
#7638 = CARTESIAN_POINT ( 'NONE',  ( 759.2295555964440155, 7.830767346494148740, -353.9708237608231229 ) ) ;
#7639 = CARTESIAN_POINT ( 'NONE',  ( 763.2262854647970016, -296.6346026584195670, 309.2812353651462445 ) ) ;
#7640 = LINE ( 'NONE', #8110, #14493 ) ;
#7641 = CARTESIAN_POINT ( 'NONE',  ( 879.9999999999990905, 479.9999999999998863, -360.0000000000000000 ) ) ;
#7642 = CARTESIAN_POINT ( 'NONE',  ( 804.4086373105744769, -145.6454272087893287, 333.3843516231986541 ) ) ;
#7643 = CARTESIAN_POINT ( 'NONE',  ( 803.6646147819161570, -65.90732993114758642, 348.8264449731210561 ) ) ;
#7644 = ORIENTED_EDGE ( 'NONE', *, *, #43110, .T. ) ;
#7645 = CARTESIAN_POINT ( 'NONE',  ( 754.3581564841646241, -425.4636090269703459, -316.1443688327762516 ) ) ;
#7646 = CARTESIAN_POINT ( 'NONE',  ( 745.7998596910086917, -5.361875385693257279, -332.5602148656461168 ) ) ;
#7647 = CARTESIAN_POINT ( 'NONE',  ( 762.1177392798416577, -258.5545181178799226, 309.8865473780659272 ) ) ;
#7648 = CARTESIAN_POINT ( 'NONE',  ( 759.2295555964440155, -232.1692326535051620, 353.9708237608231229 ) ) ;
#7649 = CARTESIAN_POINT ( 'NONE',  ( 797.6776695296629214, -355.5436935675103882, -357.6776695296636603 ) ) ;
#7650 = COLOUR_RGB ( '',0.7921568627450980005, 0.8196078431372548767, 0.9333333333333333481 ) ;
#7651 = CARTESIAN_POINT ( 'NONE',  ( 801.9419747391806368, 5.547215523397618142, 351.9812246680014027 ) ) ;
#7652 = FACE_OUTER_BOUND ( 'NONE', #4893, .T. ) ;
#7653 = CARTESIAN_POINT ( 'NONE',  ( 757.0176451133909268, -229.0999726633345404, -349.9200121543848354 ) ) ;
#7654 = CARTESIAN_POINT ( 'NONE',  ( 755.2512626584698410, -7.543693567511430942, 315.2512626584710915 ) ) ;
#7655 = CARTESIAN_POINT ( 'NONE',  ( 808.0189434323515343, -110.0891481129656597, 319.0252816721025511 ) ) ;
#7656 = CARTESIAN_POINT ( 'NONE',  ( 181.1634899080285948, 260.0000000000000000, -191.9749999999953900 ) ) ;
#7657 = DIRECTION ( 'NONE',  ( 0.000000000000000000, -1.000000000000000000, 0.000000000000000000 ) ) ;
#7658 = EDGE_CURVE ( 'NONE', #9644, #41015, #2584, .T. ) ;
#7659 = CARTESIAN_POINT ( 'NONE',  ( 914.9999999999992042, 74.99999999999984368, -350.0000000000000000 ) ) ;
#7660 = CARTESIAN_POINT ( 'NONE',  ( 814.8207195650702488, -386.1908817542432075, 336.2433038121456548 ) ) ;
#7661 = DIRECTION ( 'NONE',  ( -0.000000000000000000, 1.000000000000000000, -0.000000000000000000 ) ) ;
#7662 = CARTESIAN_POINT ( 'NONE',  ( 745.4481719005789273, -315.7255117493286320, 347.5162901302853129 ) ) ;
#7663 = CARTESIAN_POINT ( 'NONE',  ( 758.8095938919642549, -104.0891481129656881, -311.6929314249763365 ) ) ;
#7664 = CARTESIAN_POINT ( 'NONE',  ( 785.3687786644884454, -299.3618753856922581, -315.3201227861279676 ) ) ;
#7665 = PLANE ( 'NONE',  #3350 ) ;
#7666 = CARTESIAN_POINT ( 'NONE',  ( 774.6858677611749044, -441.7255117493282910, 315.5713283507209894 ) ) ;
#7667 = CIRCLE ( 'NONE', #42340, 7.999999999999785061 ) ;
#7668 = CARTESIAN_POINT ( 'NONE',  ( 755.1538015810308480, -182.1908817542437760, 343.0433043558613804 ) ) ;
#7669 = CARTESIAN_POINT ( 'NONE',  ( 783.7953271457878373, -56.19088175424417386, -375.1787889125761239 ) ) ;
#7670 = CARTESIAN_POINT ( 'NONE',  ( 790.8726784830453198, -82.71468719896012090, -362.5472867521010585 ) ) ;
#7671 = CARTESIAN_POINT ( 'NONE',  ( 781.2497674668890113, -84.35105083532374692, 375.3608509340180603 ) ) ;
#7672 = CARTESIAN_POINT ( 'NONE',  ( 804.4286716492782716, -401.3618753856920307, 345.3141322388244703 ) ) ;
#7673 = CARTESIAN_POINT ( 'NONE',  ( 755.3201227861273992, -3.725511749329622813, -345.3687786644892981 ) ) ;
#7675 = VERTEX_POINT ( 'NONE', #45091 ) ;
#7674 = CARTESIAN_POINT ( 'NONE',  ( 780.5290396650775619, -108.3510508353236759, -365.2837595273619513 ) ) ;
#7676 = CARTESIAN_POINT ( 'NONE',  ( 781.7834795799800531, -82.81642084023846451, -315.0636971347436202 ) ) ;
#7677 = CARTESIAN_POINT ( 'NONE',  ( 803.8651313633788504, -413.2601417444136018, -332.4468031744301015 ) ) ;
#7678 = ADVANCED_FACE ( 'NONE', ( #15045 ), #14360, .T. ) ;
#7680 = CARTESIAN_POINT ( 'NONE',  ( 804.4286716492782716, -209.3618753856926276, 345.3141322388244703 ) ) ;
#7679 = CARTESIAN_POINT ( 'NONE',  ( 800.2193346964447755, -234.9982390220561683, 355.1360043628815788 ) ) ;
#7681 = CARTESIAN_POINT ( 'NONE',  ( 778.7502325331095108, -408.3510508353227806, -304.6391490659818828 ) ) ;
#7682 = DIRECTION ( 'NONE',  ( -0.000000000000000000, 1.000000000000000000, -0.000000000000000000 ) ) ;
#7683 = ORIENTED_EDGE ( 'NONE', *, *, #8040, .F. ) ;
#7684 = CARTESIAN_POINT ( 'NONE',  ( 774.6312213355099630, -431.3618753856918033, 364.6798772138717482 ) ) ;
#7685 = VECTOR ( 'NONE', #1888, 1000.000000000000114 ) ;
#7686 = ORIENTED_EDGE ( 'NONE', *, *, #11685, .F. ) ;
#7687 = CARTESIAN_POINT ( 'NONE',  ( 777.5031285880264704, -238.8164208402379813, -374.9108240113588408 ) ) ;
#7688 = CARTESIAN_POINT ( 'NONE',  ( 813.1304606946831655, -185.9073299311472169, 352.3570229623691716 ) ) ;
#7689 = CARTESIAN_POINT ( 'NONE',  ( 766.9102291470427417, -258.5545181178799226, 318.6633372737382501 ) ) ;
#7690 = ORIENTED_EDGE ( 'NONE', *, *, #32569, .T. ) ;
#7691 = CARTESIAN_POINT ( 'NONE',  ( 755.3028492785439312, -63.28179084515324604, -335.9200461376539693 ) ) ;
#7692 = CARTESIAN_POINT ( 'NONE',  ( 788.8264449731201466, -261.1800572038742416, -363.6646147819170665 ) ) ;
#7693 = ORIENTED_EDGE ( 'NONE', *, *, #45012, .T. ) ;
#7694 = CARTESIAN_POINT ( 'NONE',  ( 756.5762568750052424, -387.1800572038738437, -348.7366044899774238 ) ) ;
#7695 = CARTESIAN_POINT ( 'NONE',  ( 788.7366044899766848, -59.90732993114762905, -316.5762568750059813 ) ) ;
#7696 = CARTESIAN_POINT ( 'NONE',  ( 803.8651313633788504, -245.2601417444141987, 332.4468031744301015 ) ) ;
#7697 = CARTESIAN_POINT ( 'NONE',  ( 999.9999999999992042, -599.5857864376268935, 359.5857864376268935 ) ) ;
#7698 = DIRECTION ( 'NONE',  ( -0.000000000000000000, 1.000000000000000000, -0.000000000000000000 ) ) ;
#7699 = ADVANCED_FACE ( 'NONE', ( #28680 ), #12905, .F. ) ;
#7700 = ORIENTED_EDGE ( 'NONE', *, *, #28642, .T. ) ;
#7701 = CARTESIAN_POINT ( 'NONE',  ( 758.0580252608178853, -6.452784476602343666, -328.0187753319985404 ) ) ;
#7702 = DIRECTION ( 'NONE',  ( 0.000000000000000000, 0.000000000000000000, 1.000000000000000000 ) ) ;
#7703 = DIRECTION ( 'NONE',  ( -0.000000000000000000, 1.000000000000000000, -0.000000000000000000 ) ) ;
#7704 =( GEOMETRIC_REPRESENTATION_CONTEXT ( 3 ) GLOBAL_UNCERTAINTY_ASSIGNED_CONTEXT ( ( #39382 ) ) GLOBAL_UNIT_ASSIGNED_CONTEXT ( ( #6539, #17854, #42788 ) ) REPRESENTATION_CONTEXT ( 'NONE', 'WORKASPACE' ) );
#7705 = ORIENTED_EDGE ( 'NONE', *, *, #25271, .F. ) ;
#7706 = CARTESIAN_POINT ( 'NONE',  ( 762.1177392798416577, -306.5545181178797520, -309.8865473780659272 ) ) ;
#7707 = CARTESIAN_POINT ( 'NONE',  ( 754.3581564841646241, -185.4636090269710280, 316.1443688327762516 ) ) ;
#7709 = CARTESIAN_POINT ( 'NONE',  ( 801.9419747391806368, -258.4527844766016074, -351.9812246680014027 ) ) ;
#7708 = DIRECTION ( 'NONE',  ( -0.000000000000000000, -0.6755902076156505842, -0.7372773368101328550 ) ) ;
#7710 = CARTESIAN_POINT ( 'NONE',  ( 786.4999999999993179, -513.1383975375929367, -369.9999999999999432 ) ) ;
#7711 = CARTESIAN_POINT ( 'NONE',  ( 801.5560724626406000, -120.5545181178803205, -326.7756240680316182 ) ) ;
#7712 = ADVANCED_FACE ( 'NONE', ( #3737 ), #18738, .T. ) ;
#7713 = DIRECTION ( 'NONE',  ( -1.000000000000000000, -0.000000000000000000, 0.000000000000000000 ) ) ;
#7714 = CARTESIAN_POINT ( 'NONE',  ( 805.0032342141413437, -325.5436935675104451, -314.9967657858572352 ) ) ;
#7715 = DIRECTION ( 'NONE',  ( -0.000000000000000000, 1.000000000000000000, -0.000000000000000000 ) ) ;
#7716 = CARTESIAN_POINT ( 'NONE',  ( 759.7806653035534055, -6.998239022056885972, 324.8639956371180801 ) ) ;
#7717 = VECTOR ( 'NONE', #28869, 1000.000000000000000 ) ;
#7718 = CARTESIAN_POINT ( 'NONE',  ( 757.7880784355613741, -234.0090635724255037, 312.4576283171834916 ) ) ;
#7719 = CARTESIAN_POINT ( 'NONE',  ( 764.3348316497523456, -214.7146871989597230, -308.6759233522265617 ) ) ;
#7720 = CARTESIAN_POINT ( 'NONE',  ( 747.2067596250078623, -219.1800572038744122, 352.2312462859687230 ) ) ;
#7721 = CARTESIAN_POINT ( 'NONE',  ( 804.7487373415286811, -427.5436935675101040, -364.7487373415288516 ) ) ;
#7722 = CARTESIAN_POINT ( 'NONE',  ( 939.9999999999993179, -600.0000000000001137, 360.0000000000000000 ) ) ;
#7723 = VECTOR ( 'NONE', #25318, 1000.000000000000000 ) ;
#7724 = CARTESIAN_POINT ( 'NONE',  ( 762.3223304703356007, -319.5436935675104451, 322.3223304703362828 ) ) ;
#7725 = CARTESIAN_POINT ( 'NONE',  ( 757.0176451133909268, -85.09997266333499510, 349.9200121543848354 ) ) ;
#7726 = CARTESIAN_POINT ( 'NONE',  ( 757.4527132478984868, -88.37269993606226137, 329.1273215169538844 ) ) ;
#7727 = CARTESIAN_POINT ( 'NONE',  ( 803.2186876482843445, 16.01258552831230375, -350.0220218866286928 ) ) ;
#7728 = FACE_OUTER_BOUND ( 'NONE', #22615, .T. ) ;
#7730 = ADVANCED_FACE ( 'NONE', ( #11120 ), #43215, .F. ) ;
#7729 = CARTESIAN_POINT ( 'NONE',  ( 939.9999999999993179, 56.78581973499407809, 212.6378164459127618 ) ) ;
#7732 = CARTESIAN_POINT ( 'NONE',  ( 755.5713283507202505, -365.3618753856920875, 334.6858677611754729 ) ) ;
#7731 = CARTESIAN_POINT ( 'NONE',  ( 772.3691319403857278, -167.2601417444143976, 315.8894580844506663 ) ) ;
#7733 = ORIENTED_EDGE ( 'NONE', *, *, #21305, .F. ) ;
#7734 = CLOSED_SHELL ( 'NONE', ( #18555, #27777, #6630, #41065, #10811, #12974, #23831, #28874, #36584, #32049, #44130 ) ) ;
#7735 = CARTESIAN_POINT ( 'NONE',  ( 773.3843516231979720, -277.4419599262322436, -364.4086373105754433 ) ) ;
#7736 = CARTESIAN_POINT ( 'NONE',  ( 758.0580252608178853, -126.4527844766019626, 328.0187753319985404 ) ) ;
#7737 = CIRCLE ( 'NONE', #36509, 10.00000000000000888 ) ;
#7738 = CARTESIAN_POINT ( 'NONE',  ( 744.9990715423526808, -282.3510508353230080, -341.2370466360926002 ) ) ;
#7739 = LINE ( 'NONE', #21586, #562 ) ;
#7740 = CARTESIAN_POINT ( 'NONE',  ( 800.1688906516307043, -442.1692326535044231, 369.0717654672308186 ) ) ;
#7741 = ORIENTED_EDGE ( 'NONE', *, *, #37087, .T. ) ;
#7742 = CARTESIAN_POINT ( 'NONE',  ( 762.1405469898971887, -337.5436935675102177, 357.8594530101015607 ) ) ;
#7743 = AXIS2_PLACEMENT_3D ( 'NONE', #32884, #18571, #14660 ) ;
#7744 = CARTESIAN_POINT ( 'NONE',  ( 754.8983024940795303, -66.89650538077835051, -336.9254006560228163 ) ) ;
#7745 = CARTESIAN_POINT ( 'NONE',  ( 804.6798772138708955, -447.7255117493280636, 334.6312213355107019 ) ) ;
#7746 = CARTESIAN_POINT ( 'NONE',  ( 813.1304606946830518, -137.9073299311473875, -352.3570229623690580 ) ) ;
#7747 = VERTEX_POINT ( 'NONE', #35584 ) ;
#7748 = CARTESIAN_POINT ( 'NONE',  ( 781.7834795799800531, -130.8164208402383224, -315.0636971347436202 ) ) ;
#7749 = VERTEX_POINT ( 'NONE', #731 ) ;
#7750 = CARTESIAN_POINT ( 'NONE',  ( 755.1538015810308480, -422.1908817542430370, -343.0433043558613804 ) ) ;
#7751 = ADVANCED_FACE ( 'NONE', ( #1177, #4640 ), #18300, .F. ) ;
#7752 = CARTESIAN_POINT ( 'NONE',  ( 796.1575198192839480, -462.0090635724247932, 359.4546378042384163 ) ) ;
#7753 = CARTESIAN_POINT ( 'NONE',  ( 770.0799878456142551, -133.9874144716872024, 362.9823548866085616 ) ) ;
#7756 = CARTESIAN_POINT ( 'NONE',  ( 771.2368401574024119, -397.4419599262317320, 374.2805881961240857 ) ) ;
#7755 = CARTESIAN_POINT ( 'NONE',  ( 989.9999999999992042, 46.15097736693707020, -350.0000000000000000 ) ) ;
#7754 = DIRECTION ( 'NONE',  ( 0.000000000000000000, 0.000000000000000000, 1.000000000000000000 ) ) ;
#7757 = CIRCLE ( 'NONE', #23219, 12.00000000000001066 ) ;
#7758 = ADVANCED_FACE ( 'NONE', ( #28903 ), #18519, .F. ) ;
#7759 = AXIS2_PLACEMENT_3D ( 'NONE', #25766, #32479, #5191 ) ;
#7760 = EDGE_LOOP ( 'NONE', ( #40509, #37942, #883, #18815 ) ) ;
#7761 = CARTESIAN_POINT ( 'NONE',  ( 766.9102291470427417, -378.5545181178795247, -318.6633372737382501 ) ) ;
#7762 = DIRECTION ( 'NONE',  ( 0.000000000000000000, 0.000000000000000000, 1.000000000000000000 ) ) ;
#7763 = CARTESIAN_POINT ( 'NONE',  ( 778.7629533639073998, -176.7363362996983369, -375.0009284576466371 ) ) ;
#7764 = CARTESIAN_POINT ( 'NONE',  ( 811.3240766477731540, -76.37269993606228979, 355.6651683502462902 ) ) ;
#7766 = CARTESIAN_POINT ( 'NONE',  ( 187.1337867209877857, 56.73212367640085318, 362.5753187112032379 ) ) ;
#7765 = LINE ( 'NONE', #7317, #20438 ) ;
#7767 = CARTESIAN_POINT ( 'NONE',  ( 794.1144889064781864, -322.1692326535048210, -360.9840315886528401 ) ) ;
#7768 = PLANE ( 'NONE',  #43890 ) ;
#7769 = CARTESIAN_POINT ( 'NONE',  ( 802.2119215644370342, -198.0090635724255606, -367.5423716828165084 ) ) ;
#7770 = CARTESIAN_POINT ( 'NONE',  ( 571.1634899080285095, 259.9999999999999432, -199.9999999999981526 ) ) ;
#7772 = EDGE_CURVE ( 'NONE', #23907, #22842, #11472, .T. ) ;
#7771 = PLANE ( 'NONE',  #45215 ) ;
#7773 = ADVANCED_FACE ( 'NONE', ( #11349 ), #25427, .F. ) ;
#7774 = CARTESIAN_POINT ( 'NONE',  ( 758.4439275373578084, -372.5545181178796383, 353.2243759319684386 ) ) ;
#7775 = CIRCLE ( 'NONE', #1129, 2.749999999999891642 ) ;
#7776 = CARTESIAN_POINT ( 'NONE',  ( 814.8207195650702488, -338.1908817542433212, 336.2433038121456548 ) ) ;
#7777 = VECTOR ( 'NONE', #9489, 1000.000000000000000 ) ;
#7778 = CARTESIAN_POINT ( 'NONE',  ( 744.7301800767020268, -220.8164208402380098, -337.4774526936615189 ) ) ;
#7779 = DIRECTION ( 'NONE',  ( 0.000000000000000000, 0.000000000000000000, 1.000000000000000000 ) ) ;
#7780 = CARTESIAN_POINT ( 'NONE',  ( 762.3223304703356007, -31.54369356751135456, -322.3223304703362828 ) ) ;
#7781 = AXIS2_PLACEMENT_3D ( 'NONE', #14828, #21505, #36064 ) ;
#7782 = CARTESIAN_POINT ( 'NONE',  ( 778.7629533639073998, -128.7363362996984790, 375.0009284576466371 ) ) ;
#7783 = CARTESIAN_POINT ( 'NONE',  ( 788.7631598425961101, -97.44195992623281199, -305.7194118038759143 ) ) ;
#7784 = CARTESIAN_POINT ( 'NONE',  ( 751.6929314249748586, -102.9982390220565520, 318.8095938919659034 ) ) ;
#7785 = CARTESIAN_POINT ( 'NONE',  ( 746.8695393053150156, -341.9073299311465917, -327.6429770376306010 ) ) ;
#7786 = DIRECTION ( 'NONE',  ( -1.000000000000000000, 0.000000000000000000, 0.000000000000000000 ) ) ;
#7787 = CARTESIAN_POINT ( 'NONE',  ( 879.9999999999992042, 249.9999999999998295, -360.0000000000000000 ) ) ;
#7788 = CARTESIAN_POINT ( 'NONE',  ( 797.8594530101008786, -205.5436935675108430, 322.1405469898980982 ) ) ;
#7789 = AXIS2_PLACEMENT_3D ( 'NONE', #7328, #7096, #34399 ) ;
#7790 = CARTESIAN_POINT ( 'NONE',  ( 766.9102291470427417, 5.445481882119263872, 318.6633372737382501 ) ) ;
#7791 = EDGE_CURVE ( 'NONE', #32511, #21321, #32136, .T. ) ;
#7792 = CARTESIAN_POINT ( 'NONE',  ( 793.4146539503750546, -409.9874144716863498, -307.6481478633938877 ) ) ;
#7793 = VECTOR ( 'NONE', #42146, 1000.000000000000000 ) ;
#7794 = CARTESIAN_POINT ( 'NONE',  ( 745.0891759886404770, -412.2709662947829088, -342.4968714119734159 ) ) ;
#7796 = EDGE_CURVE ( 'NONE', #33292, #15749, #21734, .T. ) ;
#7795 = DIRECTION ( 'NONE',  ( 0.000000000000000000, 0.3826834323650838421, 0.9238795325112891810 ) ) ;
#7797 = CARTESIAN_POINT ( 'NONE',  ( 786.2056067578752163, -35.80559628986934229, 374.4686193811670023 ) ) ;
#7798 = ORIENTED_EDGE ( 'NONE', *, *, #21358, .T. ) ;
#7799 = AXIS2_PLACEMENT_3D ( 'NONE', #14200, #4707, #7285 ) ;
#7800 = CARTESIAN_POINT ( 'NONE',  ( 805.0264073115434940, -174.3510508353234627, -339.4763451958999099 ) ) ;
#7801 = CARTESIAN_POINT ( 'NONE',  ( 802.1676090361156639, -14.63460265842049424, 327.8955696845344505 ) ) ;
#7802 = CARTESIAN_POINT ( 'NONE',  ( 795.6651683502461765, -202.7146871989597514, -371.3240766477733814 ) ) ;
#7803 = CARTESIAN_POINT ( 'NONE',  ( 989.9999999999992042, 56.60618624968560653, 350.0000000000000000 ) ) ;
#7804 = CARTESIAN_POINT ( 'NONE',  ( 778.7502325331095108, -312.3510508353230080, 304.6391490659818828 ) ) ;
#7805 = CARTESIAN_POINT ( 'NONE',  ( 755.0636971347428243, -148.2709662947837330, 341.7834795799807353 ) ) ;
#7806 = VERTEX_POINT ( 'NONE', #22191 ) ;
#7807 = CARTESIAN_POINT ( 'NONE',  ( 774.6858677611749044, -321.7255117493286320, 315.5713283507209894 ) ) ;
#7808 = CARTESIAN_POINT ( 'NONE',  ( 792.3570229623688874, -45.18005720387493085, -373.1304606946836202 ) ) ;
#7809 = CIRCLE ( 'NONE', #20960, 12.00000000000001066 ) ;
#7810 = EDGE_CURVE ( 'NONE', #30700, #40621, #36511, .T. ) ;
#7811 = VERTEX_POINT ( 'NONE', #8128 ) ;
#7812 = CARTESIAN_POINT ( 'NONE',  ( 813.5763878283155464, -435.8272453906066062, -351.1614460488615350 ) ) ;
#7813 = CIRCLE ( 'NONE', #17399, 18.00000000000001421 ) ;
#7814 = VERTEX_POINT ( 'NONE', #32825 ) ;
#7815 = APPLICATION_PROTOCOL_DEFINITION ( 'draft international standard', 'automotive_design', 1998, #17542 ) ;
#7816 = EDGE_CURVE ( 'NONE', #19677, #28770, #22488, .T. ) ;
#7818 = CARTESIAN_POINT ( 'NONE',  ( 804.4086373105744769, -385.6454272087888171, 333.3843516231986541 ) ) ;
#7817 = CARTESIAN_POINT ( 'NONE',  ( 762.1405469898971887, -49.54369356751129061, 357.8594530101015607 ) ) ;
#7819 = CARTESIAN_POINT ( 'NONE',  ( 762.3223304703356007, -295.5436935675105588, -322.3223304703362828 ) ) ;
#7821 = CARTESIAN_POINT ( 'NONE',  ( 754.0944755984390895, -279.6237781080503737, 364.1009440267246760 ) ) ;
#7820 = CARTESIAN_POINT ( 'NONE',  ( 811.0346526505617248, -398.6346026584193396, 323.0537975583478101 ) ) ;
#7822 = EDGE_CURVE ( 'NONE', #36156, #45518, #7211, .T. ) ;
#7823 = CARTESIAN_POINT ( 'NONE',  ( 781.2497674668890113, -60.35105083532383219, 375.3608509340180603 ) ) ;
#7824 = CARTESIAN_POINT ( 'NONE',  ( 757.4527132478984868, -304.3726999360615082, -329.1273215169538844 ) ) ;
#7825 = CARTESIAN_POINT ( 'NONE',  ( 788.8264449731200330, -285.1800572038740711, -363.6646147819171233 ) ) ;
#7826 = DIRECTION ( 'NONE',  ( 0.000000000000000000, 0.000000000000000000, -1.000000000000000000 ) ) ;
#7827 = CARTESIAN_POINT ( 'NONE',  ( 785.3141322388236176, -117.7255117493292715, -364.4286716492789537 ) ) ;
#7828 = DIRECTION ( 'NONE',  ( -1.000000000000000000, 0.000000000000000000, 0.000000000000000000 ) ) ;
#7829 = EDGE_LOOP ( 'NONE', ( #19942, #40796, #21647, #32915, #37820, #44988, #44830 ) ) ;
#7830 = CARTESIAN_POINT ( 'NONE',  ( 805.0032342141412300, -397.5436935675100472, 314.9967657858571783 ) ) ;
#7831 =( GEOMETRIC_REPRESENTATION_CONTEXT ( 3 ) GLOBAL_UNCERTAINTY_ASSIGNED_CONTEXT ( ( #43509 ) ) GLOBAL_UNIT_ASSIGNED_CONTEXT ( ( #24063, #41636, #34227 ) ) REPRESENTATION_CONTEXT ( 'NONE', 'WORKASPACE' ) );
#7833 = DIRECTION ( 'NONE',  ( -0.000000000000000000, 1.000000000000000000, -0.000000000000000000 ) ) ;
#7832 = DIRECTION ( 'NONE',  ( 1.000000000000000000, 0.000000000000000000, 0.000000000000000000 ) ) ;
#7834 = CARTESIAN_POINT ( 'NONE',  ( 757.7880784355613741, -90.00906357242590161, -312.4576283171834916 ) ) ;
#7835 = CARTESIAN_POINT ( 'NONE',  ( 311.1634899080286232, 260.0000000000000000, -199.9999999999963336 ) ) ;
#7837 = EDGE_CURVE ( 'NONE', #20106, #6, #39508, .T. ) ;
#7836 = LINE ( 'NONE', #42467, #12729 ) ;
#7838 = CIRCLE ( 'NONE', #38823, 10.00000000000000888 ) ;
#7839 = CARTESIAN_POINT ( 'NONE',  ( 793.9708237608222134, -262.9181544815162965, 319.2295555964448681 ) ) ;
#7840 = CARTESIAN_POINT ( 'NONE',  ( 801.9419747391806368, -138.4527844766019200, 351.9812246680014027 ) ) ;
#7841 = VERTEX_POINT ( 'NONE', #7432 ) ;
#7842 = CARTESIAN_POINT ( 'NONE',  ( 751.9810565676468741, -98.08914811296568814, -360.9747183278973921 ) ) ;
#7843 = CARTESIAN_POINT ( 'NONE',  ( 783.0433043558608688, -336.8965053807774552, 315.1538015810313027 ) ) ;
#7844 = DIRECTION ( 'NONE',  ( 1.000000000000000000, 0.000000000000000000, -0.000000000000000000 ) ) ;
#7845 = CARTESIAN_POINT ( 'NONE',  ( 748.6759233522253680, -40.37269993606240348, 324.3348316497537098 ) ) ;
#7846 = CARTESIAN_POINT ( 'NONE',  ( 777.5031285880264704, -238.8164208402379813, -374.9108240113588408 ) ) ;
#7847 = CARTESIAN_POINT ( 'NONE',  ( 814.5518280994195948, -207.7255117493289447, 332.4837098697145734 ) ) ;
#7848 = CARTESIAN_POINT ( 'NONE',  ( 762.1405469898971887, -121.5436935675110419, 357.8594530101015607 ) ) ;
#7849 = DIRECTION ( 'NONE',  ( -1.000000000000000000, -0.000000000000000000, -0.000000000000000000 ) ) ;
#7850 = CARTESIAN_POINT ( 'NONE',  ( 808.7758568127978833, -292.1692326535048210, -320.0363995740631822 ) ) ;
#7851 = VECTOR ( 'NONE', #32931, 1000.000000000000000 ) ;
#7852 = CARTESIAN_POINT ( 'NONE',  ( 813.5763878283155464, -435.8272453906066062, 351.1614460488615350 ) ) ;
#7853 = CARTESIAN_POINT ( 'NONE',  ( 767.7687537140311633, -311.9073299311468759, -372.7932403749916830 ) ) ;
#7854 = CARTESIAN_POINT ( 'NONE',  ( 794.9999999999993179, 197.3292319334027241, -273.4704985657796783 ) ) ;
#7855 = CARTESIAN_POINT ( 'NONE',  ( 803.2186876482843445, -391.9874144716864066, 350.0220218866286928 ) ) ;
#7856 = VERTEX_POINT ( 'NONE', #501 ) ;
#7857 = CYLINDRICAL_SURFACE ( 'NONE', #36491, 10.00000000000000888 ) ;
#7858 = CARTESIAN_POINT ( 'NONE',  ( 802.1676090361156639, -422.6346026584192259, -327.8955696845344505 ) ) ;
#7859 = CARTESIAN_POINT ( 'NONE',  ( 758.6633372737375112, -44.53286901714205470, 326.9102291470432533 ) ) ;
#7860 = CARTESIAN_POINT ( 'NONE',  ( 792.1044303154645831, -204.4527844766016926, -317.8323909638837677 ) ) ;
#7861 = CARTESIAN_POINT ( 'NONE',  ( 768.8385539511368734, -95.26014174441461080, -306.4236121716840557 ) ) ;
#7862 = CARTESIAN_POINT ( 'NONE',  ( 756.1443688327750579, -213.6237781080506011, 314.3581564841659315 ) ) ;
#7863 = CARTESIAN_POINT ( 'NONE',  ( 794.9819416627830151, -36.99823902205679360, 319.9864689768909898 ) ) ;
#7864 = AXIS2_PLACEMENT_3D ( 'NONE', #4600, #1364, #4829 ) ;
#7865 = ORIENTED_EDGE ( 'NONE', *, *, #26116, .F. ) ;
#7866 = CARTESIAN_POINT ( 'NONE',  ( 798.7617431975189675, -219.6237781080506295, -323.0428371773161871 ) ) ;
#7867 = CARTESIAN_POINT ( 'NONE',  ( 802.1676090361156639, -206.6346026584198512, 327.8955696845344505 ) ) ;
#7868 = AXIS2_PLACEMENT_3D ( 'NONE', #25863, #32580, #39973 ) ;
#7869 = CARTESIAN_POINT ( 'NONE',  ( 786.2056067578752163, -35.80559628986934229, -374.4686193811670023 ) ) ;
#7870 = CARTESIAN_POINT ( 'NONE',  ( 794.9819416627830151, -348.9982390220558273, 319.9864689768909898 ) ) ;
#7871 = CARTESIAN_POINT ( 'NONE',  ( 787.4999999999992042, -512.9681489794448908, 370.0000000000000000 ) ) ;
#7872 = LINE ( 'NONE', #35333, #40454 ) ;
#7873 = ORIENTED_EDGE ( 'NONE', *, *, #4887, .F. ) ;
#7874 = CARTESIAN_POINT ( 'NONE',  ( 784.0799538623451781, -59.80559628986927834, 364.6971507214555572 ) ) ;
#7875 = CARTESIAN_POINT ( 'NONE',  ( 745.7194118038753459, -325.6454272087888739, -348.7631598425976449 ) ) ;
#7876 = PRODUCT_RELATED_PRODUCT_CATEGORY ( 'part', '', ( #9267 ) ) ;
#7877 = CARTESIAN_POINT ( 'NONE',  ( 782.4968714119720516, -274.8164208402378108, 305.0891759886411023 ) ) ;
#7878 = CARTESIAN_POINT ( 'NONE',  ( 747.3154664389472828, 4.012585528312341054, 326.4474001241230781 ) ) ;
#7879 = CARTESIAN_POINT ( 'NONE',  ( 787.5531968255692163, -189.8272453906073736, -316.1348686366205811 ) ) ;
#7880 = CARTESIAN_POINT ( 'NONE',  ( 785.3141322388236176, -189.7255117493290300, -364.4286716492789537 ) ) ;
#7881 = CARTESIAN_POINT ( 'NONE',  ( 762.3223304703356007, -343.5436935675103314, -322.3223304703362828 ) ) ;
#7882 = ORIENTED_EDGE ( 'NONE', *, *, #41294, .F. ) ;
#7883 = CARTESIAN_POINT ( 'NONE',  ( 803.2186876482843445, 16.01258552831230375, -350.0220218866286928 ) ) ;
#7884 = AXIS2_PLACEMENT_3D ( 'NONE', #198, #20351, #41162 ) ;
#7885 = CARTESIAN_POINT ( 'NONE',  ( 782.4968714119720516, -274.8164208402378108, 305.0891759886411023 ) ) ;
#7886 = CARTESIAN_POINT ( 'NONE',  ( 939.9999999999993179, -600.0000000000001137, -350.0000000000000000 ) ) ;
#7887 = CARTESIAN_POINT ( 'NONE',  ( 796.9571628226829034, -215.4636090269709712, 321.2382568024804641 ) ) ;
#7888 = CIRCLE ( 'NONE', #21885, 2.749999999999835687 ) ;
#7889 = PLANE ( 'NONE',  #15988 ) ;
#7890 = CARTESIAN_POINT ( 'NONE',  ( 786.5483106153019435, -151.6454272087892718, 364.1601925771022366 ) ) ;
#7891 = CARTESIAN_POINT ( 'NONE',  ( 774.6312213355099630, -47.36187538569312494, 364.6798772138717482 ) ) ;
#7892 = ORIENTED_EDGE ( 'NONE', *, *, #20407, .T. ) ;
#7893 = CARTESIAN_POINT ( 'NONE',  ( 745.5313806188320314, -399.2817908451522726, -333.7943932421247268 ) ) ;
#7894 = VECTOR ( 'NONE', #5246, 1000.000000000000000 ) ;
#7895 = CARTESIAN_POINT ( 'NONE',  ( 745.0891759886404770, -4.270966294784170003, -342.4968714119734159 ) ) ;
#7896 = CARTESIAN_POINT ( 'NONE',  ( 754.3581564841646241, -257.4636090269708575, 316.1443688327762516 ) ) ;
#7897 = CARTESIAN_POINT ( 'NONE',  ( 765.8855110935204493, -214.1692326535052189, 319.0159684113471599 ) ) ;
#7898 = VECTOR ( 'NONE', #14870, 1000.000000000000000 ) ;
#7899 = CARTESIAN_POINT ( 'NONE',  ( 785.3141322388236176, -357.7255117493285184, -364.4286716492789537 ) ) ;
#7900 = CARTESIAN_POINT ( 'NONE',  ( 914.9999999999992042, 74.99999999999984368, -350.0000000000000000 ) ) ;
#7901 = CARTESIAN_POINT ( 'NONE',  ( 771.2633955100217236, 0.09267006885218045942, 363.4237431249939618 ) ) ;
#7902 = PRESENTATION_STYLE_ASSIGNMENT (( #38855 ) ) ;
#7903 = CARTESIAN_POINT ( 'NONE',  ( 755.5913626894240451, -253.6454272087889876, -346.6156483768012890 ) ) ;
#7904 = AXIS2_PLACEMENT_3D ( 'NONE', #6153, #34568, #20917 ) ;
#7905 = CARTESIAN_POINT ( 'NONE',  ( 800.9747183278959710, -60.99823902205671544, 311.9810565676471583 ) ) ;
#7906 = CARTESIAN_POINT ( 'NONE',  ( 749.2812353651451076, -102.4527844766020337, 323.2262854647983090 ) ) ;
#7907 = CARTESIAN_POINT ( 'NONE',  ( 772.4999999999993179, -512.9681489794448908, 339.9999999999999432 ) ) ;
#7908 =( LENGTH_UNIT ( ) NAMED_UNIT ( * ) SI_UNIT ( .MILLI., .METRE. ) );
#7909 = CARTESIAN_POINT ( 'NONE',  ( 786.2694204179717872, -381.2817908451523294, 305.1769319972829067 ) ) ;
#7910 = CARTESIAN_POINT ( 'NONE',  ( 772.4999999999993179, -462.9681489794447771, -309.9999999999998863 ) ) ;
#7911 = CARTESIAN_POINT ( 'NONE',  ( 815.2698199232961542, -328.8164208402375834, 342.5225473063383106 ) ) ;
#7912 = CARTESIAN_POINT ( 'NONE',  ( 792.1044303154645831, -324.4527844766013231, -317.8323909638837677 ) ) ;
#7913 = DIRECTION ( 'NONE',  ( -1.000000000000000000, 4.147566128926363633E-16, 0.000000000000000000 ) ) ;
#7914 = CARTESIAN_POINT ( 'NONE',  ( 797.8594530101008786, -445.5436935675098766, 322.1405469898980982 ) ) ;
#7915 = CARTESIAN_POINT ( 'NONE',  ( 798.5707757039680246, -197.4636090269709996, 356.7845633553585003 ) ) ;
#7916 = CARTESIAN_POINT ( 'NONE',  ( 747.6481478633932056, -61.09997266333506616, -353.4146539503763620 ) ) ;
#7917 = CARTESIAN_POINT ( 'NONE',  ( 754.8983024940795303, -90.89650538077827946, -336.9254006560228163 ) ) ;
#7918 = CARTESIAN_POINT ( 'NONE',  ( 758.0141637701419768, -111.0783235625964096, 367.2620300519063790 ) ) ;
#7919 = CARTESIAN_POINT ( 'NONE',  ( 794.9819416627830151, -444.9982390220554862, 319.9864689768909898 ) ) ;
#7920 = CARTESIAN_POINT ( 'NONE',  ( 801.9419747391806368, 5.547215523397618142, -351.9812246680014027 ) ) ;
#7922 = ORIENTED_EDGE ( 'NONE', *, *, #27251, .T. ) ;
#7921 = CARTESIAN_POINT ( 'NONE',  ( 805.0264073115434940, -126.3510508353236048, -339.4763451958999099 ) ) ;
#7923 = CARTESIAN_POINT ( 'NONE',  ( 794.9819416627830151, -108.9982390220565804, -319.9864689768909898 ) ) ;
#7924 = VECTOR ( 'NONE', #31830, 1000.000000000000114 ) ;
#7925 = CARTESIAN_POINT ( 'NONE',  ( 772.3691319403857278, -383.2601417444137155, -315.8894580844506663 ) ) ;
#7927 = CARTESIAN_POINT ( 'NONE',  ( 771.2633955100217236, -215.9073299311471317, 363.4237431249939618 ) ) ;
#7926 = CARTESIAN_POINT ( 'NONE',  ( 804.6798772138708955, -279.7255117493288026, 334.6312213355107019 ) ) ;
#7928 = DIRECTION ( 'NONE',  ( 1.892425610156518354E-16, 1.000000000000000000, -0.000000000000000000 ) ) ;
#7929 = ORIENTED_EDGE ( 'NONE', *, *, #28639, .T. ) ;
#7930 = CARTESIAN_POINT ( 'NONE',  ( 778.1981804954714335, -418.2709662947827383, 314.8072714833589885 ) ) ;
#7931 = VECTOR ( 'NONE', #4043, 1000.000000000000000 ) ;
#7932 = ORIENTED_EDGE ( 'NONE', *, *, #2999, .T. ) ;
#7933 = CARTESIAN_POINT ( 'NONE',  ( 0.000000000000000000, 0.000000000000000000, 0.000000000000000000 ) ) ;
#7934 = AXIS2_PLACEMENT_3D ( 'NONE', #14014, #30874, #34331 ) ;
#7935 = CARTESIAN_POINT ( 'NONE',  ( 811.0346526505617248, -182.6346026584199649, 323.0537975583478101 ) ) ;
#7936 = CARTESIAN_POINT ( 'NONE',  ( 766.0291762391763086, -250.9181544815163534, 360.7704444035551319 ) ) ;
#7937 = EDGE_LOOP ( 'NONE', ( #28588, #37208, #32066, #23296 ) ) ;
#7938 = CARTESIAN_POINT ( 'NONE',  ( 773.4516893846965786, -67.64542720878958448, -315.8398074228977066 ) ) ;
#7939 = CARTESIAN_POINT ( 'NONE',  ( 807.5423716828161105, -225.0783235625959833, 362.2119215644372048 ) ) ;
#7940 = CARTESIAN_POINT ( 'NONE',  ( 800.0135310231082713, -254.0891481129652334, -325.0180583372163028 ) ) ;
#7941 = ORIENTED_EDGE ( 'NONE', *, *, #2415, .F. ) ;
#7942 = CARTESIAN_POINT ( 'NONE',  ( 755.3201227861273992, -387.7255117493283478, -345.3687786644892981 ) ) ;
#7943 = CARTESIAN_POINT ( 'NONE',  ( 778.1981804954714335, -58.27096629478398171, -314.8072714833589885 ) ) ;
#7944 = CARTESIAN_POINT ( 'NONE',  ( 754.9735926884551418, -258.3510508353231785, 340.5236548041000333 ) ) ;
#7945 = DIRECTION ( 'NONE',  ( -0.7014439490181308967, 0.1263042864341425708, 0.7014439490181749726 ) ) ;
#7946 = DIRECTION ( 'NONE',  ( 0.000000000000000000, 0.000000000000000000, 1.000000000000000000 ) ) ;
#7947 = CARTESIAN_POINT ( 'NONE',  ( 755.0636971347428243, -28.27096629478409540, -341.7834795799807353 ) ) ;
#7948 = LINE ( 'NONE', #25918, #11389 ) ;
#7949 = EDGE_LOOP ( 'NONE', ( #42912, #32586 ) ) ;
#7950 = CARTESIAN_POINT ( 'NONE',  ( 750.9282345327678740, -304.9181544815161828, -319.8311093483690115 ) ) ;
#7951 = CARTESIAN_POINT ( 'NONE',  ( 810.4231160770870019, -168.5545181178802352, 321.9338519418446936 ) ) ;
#7953 = CARTESIAN_POINT ( 'NONE',  ( 788.7366044899766848, -251.9073299311470748, -316.5762568750059813 ) ) ;
#7952 = LINE ( 'NONE', #43032, #8407 ) ;
#7954 = PLANE ( 'NONE',  #42983 ) ;
#7955 = CARTESIAN_POINT ( 'NONE',  ( 783.0745993439762742, -152.1908817542438612, -365.1016975059196739 ) ) ;
#7956 = CARTESIAN_POINT ( 'NONE',  ( 777.5031285880264704, -22.81642084023865280, 374.9108240113588408 ) ) ;
#7957 = DIRECTION ( 'NONE',  ( 1.000000000000000000, 0.000000000000000000, -0.000000000000000000 ) ) ;
#7958 = CARTESIAN_POINT ( 'NONE',  ( 747.3154664389472828, -19.98741447168758256, -326.4474001241230781 ) ) ;
#7959 = CARTESIAN_POINT ( 'NONE',  ( 808.3070685750232087, -354.9982390220557136, -361.1904061080339829 ) ) ;
#7960 = CYLINDRICAL_SURFACE ( 'NONE', #12086, 2.749999999999863665 ) ;
#7961 = CARTESIAN_POINT ( 'NONE',  ( 764.8639956371174549, -8.089148112965974136, 319.7806653035542013 ) ) ;
#7962 = VECTOR ( 'NONE', #5328, 1000.000000000000000 ) ;
#7963 = CARTESIAN_POINT ( 'NONE',  ( 799.9636004259356241, -286.9181544815161828, 311.2241431872006956 ) ) ;
#7964 = CARTESIAN_POINT ( 'NONE',  ( 800.1688906516307043, -250.1692326535050199, -369.0717654672308186 ) ) ;
#7965 = CARTESIAN_POINT ( 'NONE',  ( 763.0537975583475827, -240.4527844766015221, 371.0346526505627480 ) ) ;
#7966 = CARTESIAN_POINT ( 'NONE',  ( 811.6461892240364477, -436.7146871989589272, -324.1737431748509835 ) ) ;
#7967 = FACE_BOUND ( 'NONE', #5503, .T. ) ;
#7968 = EDGE_LOOP ( 'NONE', ( #7577, #15368 ) ) ;
#7969 = CARTESIAN_POINT ( 'NONE',  ( 788.8264449731200330, -333.1800572038740142, 363.6646147819171233 ) ) ;
#7970 = CARTESIAN_POINT ( 'NONE',  ( 804.4086373105744769, -97.64542720878949922, 333.3843516231986541 ) ) ;
#7971 = CARTESIAN_POINT ( 'NONE',  ( 791.9812246680005501, -452.6346026584191691, -361.9419747391813189 ) ) ;
#7972 = LINE ( 'NONE', #107, #4104 ) ;
#7973 = CYLINDRICAL_SURFACE ( 'NONE', #4099, 8.024999999999948841 ) ;
#7975 = CARTESIAN_POINT ( 'NONE',  ( 759.7806653035534055, -366.9982390220556567, 324.8639956371180801 ) ) ;
#7974 = CARTESIAN_POINT ( 'NONE',  ( 803.8651313633788504, -149.2601417444144261, 332.4468031744301015 ) ) ;
#7976 = ORIENTED_EDGE ( 'NONE', *, *, #31749, .T. ) ;
#7977 = CARTESIAN_POINT ( 'NONE',  ( 755.0488828828309806, -305.8055962898684470, -344.1219089521771934 ) ) ;
#7978 = CARTESIAN_POINT ( 'NONE',  ( 762.1405469898971887, -145.5436935675109851, 357.8594530101015607 ) ) ;
#7979 = UNCERTAINTY_MEASURE_WITH_UNIT (LENGTH_MEASURE( 1.000000000000000082E-05 ), #38802, 'distance_accuracy_value', 'NONE');
#7980 = CARTESIAN_POINT ( 'NONE',  ( 798.0661480581538854, -338.5328690171411381, -309.5768839229118043 ) ) ;
#7981 = DIRECTION ( 'NONE',  ( 0.000000000000000000, 0.000000000000000000, 1.000000000000000000 ) ) ;
#7982 = CARTESIAN_POINT ( 'NONE',  ( 815.1787889125755555, -438.8965053807771710, 343.7953271457877804 ) ) ;
#7983 = EDGE_CURVE ( 'NONE', #7806, #37281, #12188, .T. ) ;
#7984 = VERTEX_POINT ( 'NONE', #25879 ) ;
#7985 = CARTESIAN_POINT ( 'NONE',  ( 778.2165204200184689, -310.8164208402377540, 364.9363028652563230 ) ) ;
#7986 = CARTESIAN_POINT ( 'NONE',  ( 769.1273215169530886, -94.71468719896007826, -317.4527132478988847 ) ) ;
#7987 = CARTESIAN_POINT ( 'NONE',  ( 778.1981804954714335, -442.2709662947826814, 314.8072714833589885 ) ) ;
#7988 = EDGE_CURVE ( 'NONE', #23858, #41096, #22873, .T. ) ;
#7989 = CARTESIAN_POINT ( 'NONE',  ( 814.5518280994195948, -135.7255117493291152, -332.4837098697145734 ) ) ;
#7990 = VERTEX_POINT ( 'NONE', #12034 ) ;
#7991 = CARTESIAN_POINT ( 'NONE',  ( 800.0135310231082713, -158.0891481129655176, -325.0180583372163028 ) ) ;
#7992 = EDGE_LOOP ( 'NONE', ( #3780, #19102, #5077, #31856, #16612, #5054, #3619 ) ) ;
#7993 = CARTESIAN_POINT ( 'NONE',  ( 769.9779781133707957, -427.0999726633338582, -316.7813123517150871 ) ) ;
#7994 = CARTESIAN_POINT ( 'NONE',  ( 762.3223304703356007, 16.45630643248849267, 322.3223304703362828 ) ) ;
#7995 = CARTESIAN_POINT ( 'NONE',  ( 808.3070685750230950, -234.9982390220561683, 361.1904061080339261 ) ) ;
#7996 = CARTESIAN_POINT ( 'NONE',  ( 799.4546378042377910, -177.0783235625961538, 356.1575198192848006 ) ) ;
#7999 = CARTESIAN_POINT ( 'NONE',  ( 803.8556311672234642, -393.6237781080500326, 365.6418435158340117 ) ) ;
#7998 = DIRECTION ( 'NONE',  ( 1.000000000000000000, -0.000000000000000000, -0.000000000000000000 ) ) ;
#7997 = DIRECTION ( 'NONE',  ( -1.337618101958019798E-16, 1.000000000000000000, -1.672022627447524747E-16 ) ) ;
#8000 = ORIENTED_EDGE ( 'NONE', *, *, #13409, .T. ) ;
#8001 = CARTESIAN_POINT ( 'NONE',  ( 787.5531968255692163, -405.8272453906067199, -316.1348686366205811 ) ) ;
#8002 = DIRECTION ( 'NONE',  ( -0.000000000000000000, 1.000000000000000000, -0.000000000000000000 ) ) ;
#8003 = CARTESIAN_POINT ( 'NONE',  ( 744.6391490659812007, -206.7363362996982801, -338.7502325331110455 ) ) ;
#8004 = CARTESIAN_POINT ( 'NONE',  ( 764.1737431748507561, -82.37269993606227558, 371.6461892240376415 ) ) ;
#8006 = DIRECTION ( 'NONE',  ( -1.000000000000000000, 0.000000000000000000, 0.000000000000000000 ) ) ;
#8005 = CARTESIAN_POINT ( 'NONE',  ( 914.9999999999992042, 74.99999999999984368, -350.0000000000000000 ) ) ;
#8007 = CARTESIAN_POINT ( 'NONE',  ( 754.9735926884551418, -330.3510508353229511, -340.5236548041000333 ) ) ;
#8008 = LINE ( 'NONE', #12366, #5522 ) ;
#8009 = CARTESIAN_POINT ( 'NONE',  ( 755.8990559732751535, -179.4636090269710849, -365.9055244015606831 ) ) ;
#8010 = LINE ( 'NONE', #21849, #37035 ) ;
#8011 = FACE_BOUND ( 'NONE', #12913, .T. ) ;
#8012 = CARTESIAN_POINT ( 'NONE',  ( 805.0032342141413437, -229.5436935675107009, -314.9967657858572352 ) ) ;
#8013 = FACE_OUTER_BOUND ( 'NONE', #10547, .T. ) ;
#8014 = CARTESIAN_POINT ( 'NONE',  ( 768.0187753319979720, -8.634602658420517329, -318.0580252608186242 ) ) ;
#8015 = CARTESIAN_POINT ( 'NONE',  ( 802.2119215644370342, -174.0090635724256742, 367.5423716828165084 ) ) ;
#8016 = CARTESIAN_POINT ( 'NONE',  ( 812.6845335610512393, -103.9874144716873161, -353.5525998758768651 ) ) ;
#8017 = CARTESIAN_POINT ( 'NONE',  ( 745.7998596910086917, -125.3618753856928834, 332.5602148656461168 ) ) ;
#8018 = CARTESIAN_POINT ( 'NONE',  ( 763.0537975583475827, -360.4527844766010958, -371.0346526505627480 ) ) ;
#8019 = CARTESIAN_POINT ( 'NONE',  ( -78.83651009197140525, 260.0000000000000568, -197.2499999999937756 ) ) ;
#8020 = PLANE ( 'NONE',  #45644 ) ;
#8021 = CARTESIAN_POINT ( 'NONE',  ( 804.4286716492782716, -209.3618753856926276, 345.3141322388244703 ) ) ;
#8022 = CARTESIAN_POINT ( 'NONE',  ( 813.5763878283155464, -459.8272453906066062, 351.1614460488615350 ) ) ;
#8023 = CARTESIAN_POINT ( 'NONE',  ( 758.0141637701419768, -423.0783235625953580, -367.2620300519063790 ) ) ;
#8024 = AXIS2_PLACEMENT_3D ( 'NONE', #38580, #39271, #35106 ) ;
#8025 = CARTESIAN_POINT ( 'NONE',  ( 786.2694204179717872, 2.718209154846545683, -305.1769319972829067 ) ) ;
#8026 = DIRECTION ( 'NONE',  ( 1.000000000000000000, 0.000000000000000000, 0.000000000000000000 ) ) ;
#8027 = CARTESIAN_POINT ( 'NONE',  ( 748.3538107759620743, -16.71468719896031985, 355.8262568251490165 ) ) ;
#8028 = ORIENTED_EDGE ( 'NONE', *, *, #38258, .T. ) ;
#8029 = EDGE_CURVE ( 'NONE', #28334, #23746, #19187, .T. ) ;
#8030 = CARTESIAN_POINT ( 'NONE',  ( 755.0488828828309806, -185.8055962898689302, -344.1219089521771934 ) ) ;
#8031 = CARTESIAN_POINT ( 'NONE',  ( 797.8594530101008786, -13.54369356751140785, 322.1405469898980982 ) ) ;
#8032 = CARTESIAN_POINT ( 'NONE',  ( 786.2056067578752163, -203.8055962898688449, -374.4686193811670023 ) ) ;
#8033 = CARTESIAN_POINT ( 'NONE',  ( 999.9999999999992042, 249.5857864376267798, 359.5857864376268935 ) ) ;
#8034 = CARTESIAN_POINT ( 'NONE',  ( 752.4576283171824116, -333.0783235625956991, 317.7880784355627952 ) ) ;
#8035 = CARTESIAN_POINT ( 'NONE',  ( 764.8639956371174549, -152.0891481129655460, 319.7806653035542581 ) ) ;
#8036 = ORIENTED_EDGE ( 'NONE', *, *, #9964, .F. ) ;
#8037 = CARTESIAN_POINT ( 'NONE',  ( 776.2433038121456548, -420.8965053807772279, 374.8207195650711014 ) ) ;
#8038 = CARTESIAN_POINT ( 'NONE',  ( 795.1360043628807261, -140.0891481129654892, -360.2193346964456282 ) ) ;
#8039 = CARTESIAN_POINT ( 'NONE',  ( 778.1981804954714335, -346.2709662947830793, 314.8072714833589885 ) ) ;
#8040 = EDGE_CURVE ( 'NONE', #22842, #5612, #22403, .T. ) ;
#8041 = CARTESIAN_POINT ( 'NONE',  ( 751.6929314249748586, -54.99823902205672255, -318.8095938919659034 ) ) ;
#8042 = VERTEX_POINT ( 'NONE', #33945 ) ;
#8043 = CARTESIAN_POINT ( 'NONE',  ( 804.1009440267234822, -455.4636090269701754, -314.0944755984392600 ) ) ;
#8044 = ORIENTED_EDGE ( 'NONE', *, *, #41026, .T. ) ;
#8045 = CARTESIAN_POINT ( 'NONE',  ( 760.7433823573367135, -324.0090635724251911, -355.9930595647440441 ) ) ;
#8046 = CONTEXT_DEPENDENT_SHAPE_REPRESENTATION ( #10173, #24786 ) ;
#8048 = CARTESIAN_POINT ( 'NONE',  ( 761.4292242960306112, -353.4636090269705733, 323.2154366446414429 ) ) ;
#8047 = CARTESIAN_POINT ( 'NONE',  ( 791.9812246680005501, -44.63460265842040542, 361.9419747391813189 ) ) ;
#8049 = CARTESIAN_POINT ( 'NONE',  ( 804.4286716492782716, -305.3618753856922581, -345.3141322388244703 ) ) ;
#8051 = CARTESIAN_POINT ( 'NONE',  ( 761.9338519418445230, -278.5328690171412518, 370.4231160770881957 ) ) ;
#8050 = CARTESIAN_POINT ( 'NONE',  ( 772.4837098697145166, -407.3618753856920307, 374.5518280994205611 ) ) ;
#8052 = CARTESIAN_POINT ( 'NONE',  ( 804.4086373105744769, -289.6454272087889308, -333.3843516231986541 ) ) ;
#8053 = CARTESIAN_POINT ( 'NONE',  ( 767.8955696845333705, -288.4527844766014937, -362.1676090361162323 ) ) ;
#8054 = CYLINDRICAL_SURFACE ( 'NONE', #11775, 2.749999999999863665 ) ;
#8055 = CARTESIAN_POINT ( 'NONE',  ( 797.6776695296629214, -163.5436935675109567, -357.6776695296636603 ) ) ;
#8056 = EDGE_CURVE ( 'NONE', #15471, #14977, #5310, .T. ) ;
#8057 = CARTESIAN_POINT ( 'NONE',  ( -265.7583438952258916, -600.0000000000000000, -320.0000000000000000 ) ) ;
#8058 = ORIENTED_EDGE ( 'NONE', *, *, #16308, .T. ) ;
#8059 = AXIS2_PLACEMENT_3D ( 'NONE', #3048, #10428, #24747 ) ;
#8060 = CARTESIAN_POINT ( 'NONE',  ( 782.4968714119720516, -418.8164208402374129, 305.0891759886411023 ) ) ;
#8062 = CARTESIAN_POINT ( 'NONE',  ( 779.9999999999992042, 16.45630643248849267, -370.0000000000000568 ) ) ;
#8061 = CARTESIAN_POINT ( 'NONE',  ( 999.9999999999992042, -599.5857864376268935, 359.5857864376268935 ) ) ;
#8063 = EDGE_CURVE ( 'NONE', #17707, #2736, #38007, .T. ) ;
#8064 = CARTESIAN_POINT ( 'NONE',  ( 786.2694204179717872, -93.28179084515315367, -305.1769319972829067 ) ) ;
#8065 = FACE_OUTER_BOUND ( 'NONE', #29938, .T. ) ;
#8066 = DIRECTION ( 'NONE',  ( 1.000000000000000000, -0.000000000000000000, -0.000000000000000000 ) ) ;
#8067 = CARTESIAN_POINT ( 'NONE',  ( 776.9254006560222479, -284.1908817542434917, 314.8983024940802125 ) ) ;
#8068 = CARTESIAN_POINT ( 'NONE',  ( 767.8955696845333705, -144.4527844766018632, 362.1676090361162323 ) ) ;
#8069 = ORIENTED_EDGE ( 'NONE', *, *, #17979, .F. ) ;
#8070 = CARTESIAN_POINT ( 'NONE',  ( 805.0032342141413437, -109.5436935675110988, -314.9967657858572352 ) ) ;
#8071 = CARTESIAN_POINT ( 'NONE',  ( 756.7813123517142913, -331.9874144716865203, 329.9779781133712504 ) ) ;
#8072 = LINE ( 'NONE', #22134, #38911 ) ;
#8073 = CARTESIAN_POINT ( 'NONE',  ( 795.8262568251477660, -46.37269993606239638, 308.3538107759623585 ) ) ;
#8074 = CARTESIAN_POINT ( 'NONE',  ( 763.2262854647970016, -248.6346026584197659, -309.2812353651462445 ) ) ;
#8075 = CARTESIAN_POINT ( 'NONE',  ( 787.5162901302840055, -203.3618753856925991, 305.4481719005792684 ) ) ;
#8076 = CARTESIAN_POINT ( 'NONE',  ( 762.3223304703356007, -127.5436935675110561, 322.3223304703362828 ) ) ;
#8077 = CARTESIAN_POINT ( 'NONE',  ( 454.7528517110262101, 239.9999999999999716, -122.7905160835442615 ) ) ;
#8078 = CARTESIAN_POINT ( 'NONE',  ( 788.7631598425961101, -313.4419599262320730, -305.7194118038759143 ) ) ;
#8079 = EDGE_CURVE ( 'NONE', #9510, #36235, #3355, .T. ) ;
#8080 = CARTESIAN_POINT ( 'NONE',  ( 784.1219089521767955, -21.28179084515337749, 315.0488828828318333 ) ) ;
#8081 = CARTESIAN_POINT ( 'NONE',  ( 800.9747183278959710, -324.9982390220559409, -311.9810565676471583 ) ) ;
#8082 = LINE ( 'NONE', #11980, #37938 ) ;
#8083 = CARTESIAN_POINT ( 'NONE',  ( 789.9200121543843807, -385.9874144716864066, 317.0176451133914384 ) ) ;
#8084 = ORIENTED_EDGE ( 'NONE', *, *, #42226, .T. ) ;
#8085 = CARTESIAN_POINT ( 'NONE',  ( 785.3141322388236176, -429.7255117493282910, -364.4286716492789537 ) ) ;
#8086 = EDGE_CURVE ( 'NONE', #10075, #27381, #16168, .T. ) ;
#8087 = CARTESIAN_POINT ( 'NONE',  ( 791.9812246680005501, -212.6346026584198796, -361.9419747391813189 ) ) ;
#8088 = CARTESIAN_POINT ( 'NONE',  ( 798.0661480581538854, -74.53286901714196233, -309.5768839229118043 ) ) ;
#8089 = CARTESIAN_POINT ( 'NONE',  ( 799.9999999999993179, 205.0000000000000568, -255.0000000000000000 ) ) ;
#8090 = CARTESIAN_POINT ( 'NONE',  ( 783.7566961878529810, -240.8965053807777963, 305.1792804349288417 ) ) ;
#8091 = CARTESIAN_POINT ( 'NONE',  ( 788.7366044899766848, -59.90732993114762905, 316.5762568750059813 ) ) ;
#8092 = AXIS2_PLACEMENT_3D ( 'NONE', #39555, #40221, #21980 ) ;
#8093 = CARTESIAN_POINT ( 'NONE',  ( 766.7756240680305382, -230.5328690171415076, -361.5560724626415663 ) ) ;
#8094 = EDGE_CURVE ( 'NONE', #27562, #41260, #4087, .T. ) ;
#8095 = CARTESIAN_POINT ( 'NONE',  ( 785.3687786644884454, -227.3618753856925707, 315.3201227861279676 ) ) ;
#8096 = ADVANCED_FACE ( 'NONE', ( #16395 ), #11810, .F. ) ;
#8097 = CARTESIAN_POINT ( 'NONE',  ( 814.8230680027162407, -77.80559628986920018, -333.7305795820267917 ) ) ;
#8098 = DIRECTION ( 'NONE',  ( 1.000000000000000000, -0.000000000000000000, -0.000000000000000000 ) ) ;
#8099 = ORIENTED_EDGE ( 'NONE', *, *, #42697, .T. ) ;
#8100 = CARTESIAN_POINT ( 'NONE',  ( 813.5763878283155464, -339.8272453906069472, -351.1614460488615350 ) ) ;
#8101 = CARTESIAN_POINT ( 'NONE',  ( 777.5031285880264704, -286.8164208402378677, 374.9108240113588408 ) ) ;
#8102 = CARTESIAN_POINT ( 'NONE',  ( 800.1688906516307043, 13.83076734649413098, 369.0717654672308186 ) ) ;
#8103 = APPLICATION_CONTEXT ( 'automotive_design' ) ;
#8104 = CARTESIAN_POINT ( 'NONE',  ( 761.4292242960306112, -185.4636090269710280, -323.2154366446414429 ) ) ;
#8105 = CARTESIAN_POINT ( 'NONE',  ( 797.8594530101008786, -181.5436935675108145, -322.1405469898980982 ) ) ;
#8106 = CARTESIAN_POINT ( 'NONE',  ( 788.8264449731201466, -381.1800572038739006, -363.6646147819170665 ) ) ;
#8107 = EDGE_LOOP ( 'NONE', ( #36094, #15933 ) ) ;
#8108 = ORIENTED_EDGE ( 'NONE', *, *, #11198, .T. ) ;
#8109 = CARTESIAN_POINT ( 'NONE',  ( 767.7687537140311633, -335.9073299311468190, 372.7932403749916830 ) ) ;
#8110 = CARTESIAN_POINT ( 'NONE',  ( -78.83651009197140525, 260.0000000000000568, -193.8809999999935769 ) ) ;
#8111 = CARTESIAN_POINT ( 'NONE',  ( 761.4292242960306112, -209.4636090269709996, 323.2154366446414429 ) ) ;
#8112 = CARTESIAN_POINT ( 'NONE',  ( 789.9200121543843807, -361.9874144716864635, 317.0176451133914384 ) ) ;
#8113 = FACE_OUTER_BOUND ( 'NONE', #9283, .T. ) ;
#8114 = CARTESIAN_POINT ( 'NONE',  ( 769.9779781133707957, -163.0999726633347677, 316.7813123517150871 ) ) ;
#8115 = CARTESIAN_POINT ( 'NONE',  ( 785.3687786644884454, -59.36187538569306810, 315.3201227861279676 ) ) ;
#8116 = VERTEX_POINT ( 'NONE', #24230 ) ;
#8117 = CARTESIAN_POINT ( 'NONE',  ( 814.8207195650702488, -410.1908817542430370, -336.2433038121456548 ) ) ;
#8118 = CARTESIAN_POINT ( 'NONE',  ( 808.3070685750232087, 5.001760977943074948, -361.1904061080339829 ) ) ;
#8119 = CARTESIAN_POINT ( 'NONE',  ( 766.4474001241216001, -259.0999726633343698, 307.3154664389482491 ) ) ;
#8120 = CARTESIAN_POINT ( 'NONE',  ( 760.5453621957607311, -237.0783235625960117, 323.8424801807151425 ) ) ;
#8121 = CARTESIAN_POINT ( 'NONE',  ( 804.6798772138708955, -375.7255117493283478, -334.6312213355107019 ) ) ;
#8122 = CARTESIAN_POINT ( 'NONE',  ( 441.1634899080286232, 259.9999999999999432, -197.2499999999973852 ) ) ;
#8123 = CARTESIAN_POINT ( 'NONE',  ( 758.0580252608178853, -6.452784476602343666, 328.0187753319985404 ) ) ;
#8124 = CARTESIAN_POINT ( 'NONE',  ( -786.4999999999993179, -513.1383975375929367, -369.9999999999999432 ) ) ;
#8125 = CARTESIAN_POINT ( 'NONE',  ( 772.4468031744293057, -249.8272453906072315, -363.8651313633793620 ) ) ;
#8126 = CARTESIAN_POINT ( 'NONE',  ( 804.7487373415286811, -43.54369356751131903, 364.7487373415288516 ) ) ;
#8127 = CARTESIAN_POINT ( 'NONE',  ( 754.9967657858570647, -97.54369356751112718, 365.0032342141425374 ) ) ;
#8128 = CARTESIAN_POINT ( 'NONE',  ( 454.7528517110262101, 230.0000000000002274, 339.9999999999999432 ) ) ;
#8129 = DIRECTION ( 'NONE',  ( 0.000000000000000000, 0.7517448203044204691, 0.6594541114781790059 ) ) ;
#8130 = CARTESIAN_POINT ( 'NONE',  ( 745.5313806188320314, -399.2817908451522726, 333.7943932421247268 ) ) ;
#8131 = EDGE_CURVE ( 'NONE', #16382, #12764, #34405, .T. ) ;
#8132 = FACE_OUTER_BOUND ( 'NONE', #13568, .T. ) ;
#8133 = CARTESIAN_POINT ( 'NONE',  ( 805.0032342141412300, -349.5436935675102745, 314.9967657858571783 ) ) ;
#8134 = CARTESIAN_POINT ( 'NONE',  ( 804.4286716492782716, -305.3618753856922581, -345.3141322388244703 ) ) ;
#8135 = CARTESIAN_POINT ( 'NONE',  ( 778.2165204200184689, -430.8164208402374129, 364.9363028652563230 ) ) ;
#8136 = CARTESIAN_POINT ( 'NONE',  ( 783.0745993439762742, -200.1908817542436907, 365.1016975059196739 ) ) ;
#8137 = CARTESIAN_POINT ( 'NONE',  ( 757.7880784355613741, -66.00906357242595845, -312.4576283171834916 ) ) ;
#8138 = CARTESIAN_POINT ( 'NONE',  ( 759.2295555964440155, -136.1692326535053894, -353.9708237608231229 ) ) ;
#8139 = CARTESIAN_POINT ( 'NONE',  ( 778.7502325331095108, -96.35105083532370429, 304.6391490659818828 ) ) ;
#8140 = CARTESIAN_POINT ( 'NONE',  ( 781.7834795799800531, -442.8164208402372992, 315.0636971347436202 ) ) ;
#8141 = CARTESIAN_POINT ( 'NONE',  ( 808.7758568127978833, -172.1692326535052757, 320.0363995740631822 ) ) ;
#8142 = CARTESIAN_POINT ( 'NONE',  ( 785.3141322388236176, -45.72551174932949181, -364.4286716492789537 ) ) ;
#8143 = CARTESIAN_POINT ( 'NONE',  ( 763.2154366446407039, -117.6237781080509279, -321.4292242960311228 ) ) ;
#8144 = CARTESIAN_POINT ( 'NONE',  ( 792.1044303154645831, -84.45278447660206211, -317.8323909638837677 ) ) ;
#8145 = CARTESIAN_POINT ( 'NONE',  ( 800.7704444035546203, -436.1692326535044231, -326.0291762391768771 ) ) ;
#8147 = CARTESIAN_POINT ( 'NONE',  ( 774.6312213355098493, -263.3618753856924286, 364.6798772138717482 ) ) ;
#8146 = CARTESIAN_POINT ( 'NONE',  ( 756.3353852180819104, -269.9073299311468190, 331.1735550268788302 ) ) ;
#8148 = LINE ( 'NONE', #35611, #28622 ) ;
#8149 = VERTEX_POINT ( 'NONE', #41345 ) ;
#8150 = CARTESIAN_POINT ( 'NONE',  ( 796.7845633553578182, 14.37622189194867417, 358.5707757039688204 ) ) ;
#8151 = EDGE_LOOP ( 'NONE', ( #43349, #34026, #29103, #8255 ) ) ;
#8152 = CARTESIAN_POINT ( 'NONE',  ( 763.2262854647970016, -176.6346026584199933, 309.2812353651462445 ) ) ;
#8153 = CARTESIAN_POINT ( 'NONE',  ( 772.4468031744293057, -273.8272453906071746, 363.8651313633793620 ) ) ;
#8154 = VERTEX_POINT ( 'NONE', #9919 ) ;
#8155 = CARTESIAN_POINT ( 'NONE',  ( 766.9102291470427417, -66.55451811788050520, -318.6633372737382501 ) ) ;
#8156 = CARTESIAN_POINT ( 'NONE',  ( 813.9316612368132837, -223.4419599262323857, 348.6739635108323228 ) ) ;
#8157 = CARTESIAN_POINT ( 'NONE',  ( 804.4286716492782716, -281.3618753856923718, -345.3141322388244703 ) ) ;
#8158 = EDGE_LOOP ( 'NONE', ( #11451, #39576, #33005, #25466 ) ) ;
#8159 = CARTESIAN_POINT ( 'NONE',  ( 759.9864689768902508, -386.0891481129647786, -354.9819416627836404 ) ) ;
#8160 = CARTESIAN_POINT ( 'NONE',  ( 802.1676090361156639, -62.63460265842031305, -327.8955696845344505 ) ) ;
#8161 = CARTESIAN_POINT ( 'NONE',  ( 770.0799878456142551, -253.9874144716868329, 362.9823548866085616 ) ) ;
#8162 = DIRECTION ( 'NONE',  ( 0.000000000000000000, 0.000000000000000000, -1.000000000000000000 ) ) ;
#8163 = DIRECTION ( 'NONE',  ( 1.000000000000000000, -0.000000000000000000, -0.000000000000000000 ) ) ;
#8164 = CARTESIAN_POINT ( 'NONE',  ( 773.7305795820266212, -9.281790845153418346, -374.8230680027170365 ) ) ;
#8165 = DIRECTION ( 'NONE',  ( -0.000000000000000000, -0.000000000000000000, 1.000000000000000000 ) ) ;
#8166 = ORIENTED_EDGE ( 'NONE', *, *, #28958, .F. ) ;
#8167 = CARTESIAN_POINT ( 'NONE',  ( 748.6759233522253680, -304.3726999360615082, -324.3348316497537098 ) ) ;
#8168 = CARTESIAN_POINT ( 'NONE',  ( 814.8207195650702488, -170.1908817542438328, 336.2433038121456548 ) ) ;
#8170 = CARTESIAN_POINT ( 'NONE',  ( 754.8072714833581358, -244.8164208402378961, -338.1981804954720587 ) ) ;
#8169 = CARTESIAN_POINT ( 'NONE',  ( 441.1634899080286232, 229.9999999999999716, -199.9999999999972431 ) ) ;
#8171 = LINE ( 'NONE', #43485, #6080 ) ;
#8172 = CARTESIAN_POINT ( 'NONE',  ( 804.6971507214547046, -147.2817908451529547, -344.0799538623459739 ) ) ;
#8173 = CARTESIAN_POINT ( 'NONE',  ( 759.9999999999992042, 205.0000000000000568, -339.9999999999999432 ) ) ;
#8174 = CARTESIAN_POINT ( 'NONE',  ( 745.4481719005789273, -363.7255117493284615, -347.5162901302853697 ) ) ;
#8175 = CARTESIAN_POINT ( 'NONE',  ( -728.8365100919714905, 260.0000000000001705, -202.7499999999889440 ) ) ;
#8176 = CARTESIAN_POINT ( 'NONE',  ( 771.2633955100217236, 0.09267006885218045942, 363.4237431249939618 ) ) ;
#8177 = CARTESIAN_POINT ( 'NONE',  ( 768.9521613784389729, -273.8272453906071746, 373.2346286133773106 ) ) ;
#8178 = CARTESIAN_POINT ( 'NONE',  ( 751.2241431872005251, -232.1692326535051620, -359.9636004259367610 ) ) ;
#8179 = CARTESIAN_POINT ( 'NONE',  ( 751.6929314249748586, -246.9982390220560546, 318.8095938919659034 ) ) ;
#8180 = CARTESIAN_POINT ( 'NONE',  ( 813.1304606946830518, 6.092670068852159559, -352.3570229623690580 ) ) ;
#8181 = FACE_BOUND ( 'NONE', #37850, .T. ) ;
#8182 = EDGE_LOOP ( 'NONE', ( #43776, #31496, #4562, #45449 ) ) ;
#8183 = CARTESIAN_POINT ( 'NONE',  ( 759.9864689768902508, -338.0891481129649492, 354.9819416627836404 ) ) ;
#8184 = CARTESIAN_POINT ( 'NONE',  ( 787.5531968255692163, -69.82724539060775726, 316.1348686366205811 ) ) ;
#8185 = CARTESIAN_POINT ( 'NONE',  ( 784.0799538623451781, -11.80559628986942577, -364.6971507214555572 ) ) ;
#8186 = FACE_OUTER_BOUND ( 'NONE', #17296, .T. ) ;
#8187 = DIRECTION ( 'NONE',  ( 0.000000000000000000, 1.000000000000000000, 0.000000000000000000 ) ) ;
#8189 = CARTESIAN_POINT ( 'NONE',  ( 797.6776695296629214, -355.5436935675103882, 357.6776695296636603 ) ) ;
#8188 = CARTESIAN_POINT ( 'NONE',  ( 779.4709603349208464, -168.3510508353234911, 314.7162404726379918 ) ) ;
#8190 = ORIENTED_EDGE ( 'NONE', *, *, #44419, .F. ) ;
#8191 = CARTESIAN_POINT ( 'NONE',  ( 803.2186876482843445, -295.9874144716866908, -350.0220218866286928 ) ) ;
#8192 = CARTESIAN_POINT ( 'NONE',  ( 759.9864689768902508, -146.0891481129655176, 354.9819416627836404 ) ) ;
#8193 = CARTESIAN_POINT ( 'NONE',  ( 766.5853460496234675, -325.9874144716865771, -372.3518521366060554 ) ) ;
#8194 = CARTESIAN_POINT ( 'NONE',  ( -773.4999999999993179, -365.3551492539851893, -18.13243251470705886 ) ) ;
#8195 = CARTESIAN_POINT ( 'NONE',  ( 805.0032342141412300, 10.45630643248850866, 314.9967657858571783 ) ) ;
#8196 = VERTEX_POINT ( 'NONE', #37872 ) ;
#8197 = CARTESIAN_POINT ( 'NONE',  ( 759.9864689768902508, -314.0891481129650629, 354.9819416627836404 ) ) ;
#8198 = CARTESIAN_POINT ( 'NONE',  ( 765.8855110935204493, -70.16923265350563099, -319.0159684113471599 ) ) ;
#8199 = ORIENTED_EDGE ( 'NONE', *, *, #38844, .T. ) ;
#8200 = CARTESIAN_POINT ( 'NONE',  ( 781.8018195045266339, -430.2709662947827383, 365.1927285166406705 ) ) ;
#8201 = CARTESIAN_POINT ( 'NONE',  ( 805.0032342141412300, -181.5436935675108145, -314.9967657858571783 ) ) ;
#8202 = VERTEX_POINT ( 'NONE', #13397 ) ;
#8203 = CARTESIAN_POINT ( 'NONE',  ( 774.6312213355098493, -143.3618753856927697, -364.6798772138717482 ) ) ;
#8204 = VERTEX_POINT ( 'NONE', #38113 ) ;
#8205 = CARTESIAN_POINT ( 'NONE',  ( 758.4439275373578084, -420.5545181178793541, -353.2243759319684386 ) ) ;
#8206 = CARTESIAN_POINT ( 'NONE',  ( 755.5713283507202505, -5.361875385693257279, 334.6858677611754729 ) ) ;
#8207 = CARTESIAN_POINT ( 'NONE',  ( 787.5162901302840055, -227.3618753856925707, 305.4481719005792684 ) ) ;
#8208 = CARTESIAN_POINT ( 'NONE',  ( 754.8983024940795303, -162.8965053807780521, 336.9254006560228163 ) ) ;
#8210 = DIRECTION ( 'NONE',  ( 0.000000000000000000, 0.000000000000000000, -1.000000000000000000 ) ) ;
#8209 = DIRECTION ( 'NONE',  ( 0.000000000000000000, -1.000000000000000000, 0.000000000000000000 ) ) ;
#8211 = ORIENTED_EDGE ( 'NONE', *, *, #32386, .F. ) ;
#8212 = CARTESIAN_POINT ( 'NONE',  ( 804.8461984189677878, -410.1908817542430370, -336.9566956441385628 ) ) ;
#8213 = LINE ( 'NONE', #11004, #31434 ) ;
#8214 = CARTESIAN_POINT ( 'NONE',  ( 791.0478386215596629, -213.8272453906073167, -306.7653713866226326 ) ) ;
#8215 = CARTESIAN_POINT ( 'NONE',  ( 748.6759233522253680, -64.37269993606231822, 324.3348316497537098 ) ) ;
#8217 = DIRECTION ( 'NONE',  ( -0.000000000000000000, 1.000000000000000000, -0.000000000000000000 ) ) ;
#8216 = CARTESIAN_POINT ( 'NONE',  ( 928.0249999999991815, 154.9999999999998863, -360.0000000000000000 ) ) ;
#8218 = CARTESIAN_POINT ( 'NONE',  ( 789.9200121543843807, -337.9874144716865771, -317.0176451133914384 ) ) ;
#8219 = DIRECTION ( 'NONE',  ( 0.000000000000000000, 0.000000000000000000, -1.000000000000000000 ) ) ;
#8220 = CARTESIAN_POINT ( 'NONE',  ( 760.0363995740630116, -178.9181544815165239, -368.7758568127991907 ) ) ;
#8221 = CARTESIAN_POINT ( 'NONE',  ( 767.9999999999992042, 240.0000000000000853, -320.0000000000000000 ) ) ;
#8222 = CARTESIAN_POINT ( 'NONE',  ( 773.4999999999993179, -544.8427095258973623, -350.0000000000000000 ) ) ;
#8223 = CARTESIAN_POINT ( 'NONE',  ( 760.7433823573367135, -396.0090635724249637, 355.9930595647440441 ) ) ;
#8224 = CARTESIAN_POINT ( 'NONE',  ( 812.7932403749906598, -255.1800572038742700, -327.7687537140311633 ) ) ;
#8225 = CARTESIAN_POINT ( 'NONE',  ( 793.9708237608222134, -238.9181544815163534, 319.2295555964448681 ) ) ;
#8226 = CARTESIAN_POINT ( 'NONE',  ( 879.9999999999992042, 240.0000000000000568, -244.9999999999999716 ) ) ;
#8227 = CARTESIAN_POINT ( 'NONE',  ( 788.7366044899766848, -11.90732993114778182, -316.5762568750059813 ) ) ;
#8228 = CARTESIAN_POINT ( 'NONE',  ( 786.2694204179717872, -189.2817908451528979, 305.1769319972829067 ) ) ;
#8229 = CARTESIAN_POINT ( 'NONE',  ( 793.4146539503750546, -145.9874144716871740, -307.6481478633938877 ) ) ;
#8230 = CARTESIAN_POINT ( 'NONE',  ( 767.6429770376289525, -129.1800572038746111, 306.8695393053162093 ) ) ;
#8231 = CARTESIAN_POINT ( 'NONE',  ( 744.7301800767019131, -364.8164208402374697, -337.4774526936615757 ) ) ;
#8232 = LINE ( 'NONE', #25988, #31317 ) ;
#8233 = FACE_BOUND ( 'NONE', #23348, .T. ) ;
#8234 = CARTESIAN_POINT ( 'NONE',  ( 801.9419747391806368, -234.4527844766016358, 351.9812246680014027 ) ) ;
#8235 = CARTESIAN_POINT ( 'NONE',  ( 786.5483106153019435, -31.64542720878970883, 364.1601925771022366 ) ) ;
#8236 = CARTESIAN_POINT ( 'NONE',  ( 800.2193346964447755, -378.9982390220555999, -355.1360043628815788 ) ) ;
#8237 = CARTESIAN_POINT ( 'NONE',  ( 787.5162901302840055, -443.3618753856917465, -305.4481719005792684 ) ) ;
#8238 = DIRECTION ( 'NONE',  ( 0.000000000000000000, 0.9238795325112891810, -0.3826834323650838421 ) ) ;
#8239 = CARTESIAN_POINT ( 'NONE',  ( 813.2346286133761168, -29.26014174441482751, 328.9521613784389160 ) ) ;
#8240 = ORIENTED_EDGE ( 'NONE', *, *, #21048, .T. ) ;
#8241 = CARTESIAN_POINT ( 'NONE',  ( 780.5290396650775619, -204.3510508353233774, -365.2837595273619513 ) ) ;
#8242 = CARTESIAN_POINT ( 'NONE',  ( 778.1981804954714335, -34.27096629478407408, 314.8072714833589885 ) ) ;
#8243 = VECTOR ( 'NONE', #36501, 1000.000000000000227 ) ;
#8244 = CARTESIAN_POINT ( 'NONE',  ( 793.4146539503750546, -241.9874144716869182, -307.6481478633938877 ) ) ;
#8245 =( NAMED_UNIT ( * ) SI_UNIT ( $, .STERADIAN. ) SOLID_ANGLE_UNIT ( ) );
#8246 = CARTESIAN_POINT ( 'NONE',  ( 748.3538107759620743, -352.7146871989593251, 355.8262568251490165 ) ) ;
#8247 = VERTEX_POINT ( 'NONE', #20543 ) ;
#8248 = CARTESIAN_POINT ( 'NONE',  ( 800.1688906516307043, -418.1692326535044799, 369.0717654672308186 ) ) ;
#8249 = CARTESIAN_POINT ( 'NONE',  ( 755.5713283507202505, -149.3618753856928265, -334.6858677611754729 ) ) ;
#8250 = CARTESIAN_POINT ( 'NONE',  ( 788.8264449731200330, -333.1800572038740142, 363.6646147819171233 ) ) ;
#8251 = CARTESIAN_POINT ( 'NONE',  ( 813.1304606946830518, -65.90732993114758642, -352.3570229623690580 ) ) ;
#8252 = EDGE_CURVE ( 'NONE', #8116, #21264, #13620, .T. ) ;
#8253 = ORIENTED_EDGE ( 'NONE', *, *, #31216, .F. ) ;
#8254 = CARTESIAN_POINT ( 'NONE',  ( 799.2566176426618085, -0.009063572426172561425, -324.0069404352559559 ) ) ;
#8255 = ORIENTED_EDGE ( 'NONE', *, *, #45596, .F. ) ;
#8256 = CARTESIAN_POINT ( 'NONE',  ( 757.0176451133909268, -325.0999726633342561, -349.9200121543848354 ) ) ;
#8258 = CARTESIAN_POINT ( 'NONE',  ( 790.9844846989617508, -358.3726999360613945, 317.2208543904092721 ) ) ;
#8257 = CARTESIAN_POINT ( 'NONE',  ( 795.1360043628807261, -44.08914811296584446, 360.2193346964456282 ) ) ;
#8259 = CARTESIAN_POINT ( 'NONE',  ( 803.4237431249931660, -279.1800572038741848, -331.2633955100225194 ) ) ;
#8261 = CARTESIAN_POINT ( 'NONE',  ( 751.2241431872005251, -328.1692326535048210, 359.9636004259367610 ) ) ;
#8260 = CARTESIAN_POINT ( 'NONE',  ( 777.5031285880264704, -382.8164208402374697, 374.9108240113588408 ) ) ;
#8262 = CARTESIAN_POINT ( 'NONE',  ( 808.7758568127978833, -100.1692326535055315, 320.0363995740631822 ) ) ;
#8263 = CARTESIAN_POINT ( 'NONE',  ( 766.9102291470427417, -282.5545181178798657, -318.6633372737382501 ) ) ;
#8264 = CARTESIAN_POINT ( 'NONE',  ( 774.6312213355099630, -287.3618753856923718, -364.6798772138717482 ) ) ;
#8265 = DIRECTION ( 'NONE',  ( -1.000000000000000000, 0.000000000000000000, 0.000000000000000000 ) ) ;
#8266 = CARTESIAN_POINT ( 'NONE',  ( 788.8264449731200330, -141.1800572038746395, -363.6646147819171233 ) ) ;
#8267 = DIRECTION ( 'NONE',  ( 1.892425610156518354E-16, 1.000000000000000000, -0.000000000000000000 ) ) ;
#8268 = CARTESIAN_POINT ( 'NONE',  ( 751.6929314249748586, -414.9982390220555430, 318.8095938919659034 ) ) ;
#8270 = CARTESIAN_POINT ( 'NONE',  ( 786.4999999999993179, 26.27639943461401018, 900.0000000000001137 ) ) ;
#8269 = PLANE ( 'NONE',  #2707 ) ;
#8271 = CARTESIAN_POINT ( 'NONE',  ( 771.3260364891663130, -67.64542720878958448, -306.0683387631859773 ) ) ;
#8272 = CARTESIAN_POINT ( 'NONE',  ( 759.9999999999992042, -462.9681489794448339, -362.3606797749978909 ) ) ;
#8273 = CARTESIAN_POINT ( 'NONE',  ( -208.8365100919714052, 260.0000000000001137, -199.9999999999926956 ) ) ;
#8274 = EDGE_CURVE ( 'NONE', #31293, #5389, #6467, .T. ) ;
#8275 = CARTESIAN_POINT ( 'NONE',  ( 787.5531968255692163, -309.8272453906070041, 316.1348686366205811 ) ) ;
#8276 = CARTESIAN_POINT ( 'NONE',  ( 762.1405469898971887, -145.5436935675109851, 357.8594530101015607 ) ) ;
#8277 = ORIENTED_EDGE ( 'NONE', *, *, #10242, .T. ) ;
#8278 = VECTOR ( 'NONE', #32707, 1000.000000000000114 ) ;
#8279 = CARTESIAN_POINT ( 'NONE',  ( 796.9462024416508257, -132.4527844766019200, -308.9653473494370246 ) ) ;
#8280 = CARTESIAN_POINT ( 'NONE',  ( 754.9735926884551418, -330.3510508353229511, 340.5236548041000333 ) ) ;
#8281 = LINE ( 'NONE', #39936, #34463 ) ;
#8282 = CARTESIAN_POINT ( 'NONE',  ( 752.7379699480933368, -60.00906357242598688, 361.9858362298580232 ) ) ;
#8283 = CARTESIAN_POINT ( 'NONE',  ( 757.8323909638827445, -194.6346026584198796, 352.1044303154654358 ) ) ;
#8284 = CARTESIAN_POINT ( 'NONE',  ( 744.7301800767019131, -268.8164208402378108, -337.4774526936615757 ) ) ;
#8285 = EDGE_CURVE ( 'NONE', #28471, #35075, #20083, .T. ) ;
#8286 = CARTESIAN_POINT ( 'NONE',  ( 813.1304606946830518, -209.9073299311470748, 352.3570229623690580 ) ) ;
#8287 = CARTESIAN_POINT ( 'NONE',  ( 803.6646147819161570, -113.9073299311474301, 348.8264449731210561 ) ) ;
#8288 = ORIENTED_EDGE ( 'NONE', *, *, #43103, .T. ) ;
#8289 = CARTESIAN_POINT ( 'NONE',  ( 773.7943932421234194, -311.8055962898685038, -305.5313806188329409 ) ) ;
#8290 = CARTESIAN_POINT ( 'NONE',  ( 779.4763451958990572, -8.736336299698871599, 365.0264073115438919 ) ) ;
#8291 = CARTESIAN_POINT ( 'NONE',  ( 748.9653473494363425, -362.6346026584194533, -356.9462024416521331 ) ) ;
#8292 = LINE ( 'NONE', #18010, #15810 ) ;
#8293 = CARTESIAN_POINT ( 'NONE',  ( 783.0433043558608688, -384.8965053807772847, 315.1538015810313027 ) ) ;
#8294 = ORIENTED_EDGE ( 'NONE', *, *, #21009, .T. ) ;
#8295 = CARTESIAN_POINT ( 'NONE',  ( 792.1044303154645831, -420.4527844766009252, -317.8323909638837677 ) ) ;
#8296 = CARTESIAN_POINT ( 'NONE',  ( 752.4576283171824116, -117.0783235625963528, -317.7880784355627952 ) ) ;
#8298 = EDGE_CURVE ( 'NONE', #21010, #41897, #21777, .T. ) ;
#8297 = DIRECTION ( 'NONE',  ( -0.000000000000000000, 1.000000000000000000, -0.000000000000000000 ) ) ;
#8299 = CARTESIAN_POINT ( 'NONE',  ( 803.8556311672234642, -249.6237781080505158, 365.6418435158340117 ) ) ;
#8300 = CARTESIAN_POINT ( 'NONE',  ( 804.6798772138710092, -63.72551174932941365, 334.6312213355106451 ) ) ;
#8301 = EDGE_CURVE ( 'NONE', #4399, #40848, #44577, .T. ) ;
#8302 = CARTESIAN_POINT ( 'NONE',  ( 795.9930595647434757, -219.0783235625960401, -320.7433823573372820 ) ) ;
#8303 = CARTESIAN_POINT ( 'NONE',  ( 756.5762568750052424, -243.1800572038743269, 348.7366044899774238 ) ) ;
#8304 = CARTESIAN_POINT ( 'NONE',  ( 800.1688906516307043, -58.16923265350564520, -369.0717654672308186 ) ) ;
#8305 = VECTOR ( 'NONE', #31507, 1000.000000000000000 ) ;
#8306 = CARTESIAN_POINT ( 'NONE',  ( 809.4284809582966318, -452.9681489794448339, -335.2276976236387895 ) ) ;
#8307 = VERTEX_POINT ( 'NONE', #10154 ) ;
#8308 = ORIENTED_EDGE ( 'NONE', *, *, #20723, .F. ) ;
#8309 = CARTESIAN_POINT ( 'NONE',  ( 762.1177392798416577, -354.5545181178796383, -309.8865473780659272 ) ) ;
#8310 = CARTESIAN_POINT ( 'NONE',  ( 792.2312462859673587, -299.9073299311468759, 307.2067596250082602 ) ) ;
#8311 = CARTESIAN_POINT ( 'NONE',  ( 751.2241431872005251, -40.16923265350570915, 359.9636004259367610 ) ) ;
#8312 = CARTESIAN_POINT ( 'NONE',  ( 784.1219089521767955, -189.2817908451528979, -315.0488828828318333 ) ) ;
#8313 = CARTESIAN_POINT ( 'NONE',  ( 755.5713283507202505, -197.3618753856926560, -334.6858677611754729 ) ) ;
#8314 = CARTESIAN_POINT ( 'NONE',  ( 791.9812246680005501, -380.6346026584192828, -361.9419747391813189 ) ) ;
#8315 = ORIENTED_EDGE ( 'NONE', *, *, #4666, .T. ) ;
#8316 = CARTESIAN_POINT ( 'NONE',  ( 804.9511171171677688, 18.19440371013048008, -335.8780910478229202 ) ) ;
#8317 = VERTEX_POINT ( 'NONE', #23759 ) ;
#8318 = CARTESIAN_POINT ( 'NONE',  ( 759.0252816721024374, -312.9982390220559409, 368.0189434323527280 ) ) ;
#8319 = EDGE_CURVE ( 'NONE', #3612, #41109, #45393, .T. ) ;
#8320 = CARTESIAN_POINT ( 'NONE',  ( 784.4999999999993179, -563.3203001761231690, -342.3463313526983143 ) ) ;
#8321 = CARTESIAN_POINT ( 'NONE',  ( 772.3691319403857278, -359.2601417444137724, 315.8894580844506663 ) ) ;
#8322 = FACE_OUTER_BOUND ( 'NONE', #3835, .T. ) ;
#8323 = EDGE_CURVE ( 'NONE', #12356, #8307, #16866, .T. ) ;
#8324 = CARTESIAN_POINT ( 'NONE',  ( 755.3028492785439312, -183.2817908451528695, 335.9200461376539693 ) ) ;
#8325 = CARTESIAN_POINT ( 'NONE',  ( 762.3223304703356007, -31.54369356751135456, 322.3223304703362828 ) ) ;
#8326 = VERTEX_POINT ( 'NONE', #27468 ) ;
#8327 = CARTESIAN_POINT ( 'NONE',  ( 766.4474001241216001, -427.0999726633338582, -307.3154664389482491 ) ) ;
#8328 = VECTOR ( 'NONE', #17490, 1000.000000000000000 ) ;
#8329 = CARTESIAN_POINT ( 'NONE',  ( 787.4397851343537695, -45.72551174932949181, -374.2001403089903988 ) ) ;
#8330 = CARTESIAN_POINT ( 'NONE',  ( 775.9200461376533440, -215.8055962898687881, 315.3028492785443291 ) ) ;
#8331 = CARTESIAN_POINT ( 'NONE',  ( 755.0636971347428243, -388.2709662947829656, -341.7834795799807353 ) ) ;
#8332 = CARTESIAN_POINT ( 'NONE',  ( 778.2165204200184689, 1.183579159761269040, -364.9363028652563230 ) ) ;
#8333 = CARTESIAN_POINT ( 'NONE',  ( 754.9967657858570647, -433.5436935675099903, 365.0032342141425374 ) ) ;
#8334 = CARTESIAN_POINT ( 'NONE',  ( -728.8365100919714905, 256.5000000000001705, -193.8809999999890863 ) ) ;
#8335 = CARTESIAN_POINT ( 'NONE',  ( 804.8461984189677878, -242.1908817542435770, -336.9566956441385628 ) ) ;
#8336 = CARTESIAN_POINT ( 'NONE',  ( 796.9462024416508257, -180.4527844766017211, -308.9653473494370246 ) ) ;
#8337 = EDGE_CURVE ( 'NONE', #17262, #7179, #30947, .T. ) ;
#8338 = CARTESIAN_POINT ( 'NONE',  ( 815.2698199232961542, -64.81642084023852135, 342.5225473063383106 ) ) ;
#8339 = CARTESIAN_POINT ( 'NONE',  ( 751.6929314249748586, -102.9982390220565520, 318.8095938919659034 ) ) ;
#8340 = CARTESIAN_POINT ( 'NONE',  ( 792.4730984305310812, 16.45630643248850333, -314.5980907654948169 ) ) ;
#8341 = CARTESIAN_POINT ( 'NONE',  ( 757.7880784355613741, -402.0090635724250205, 312.4576283171834916 ) ) ;
#8342 = CARTESIAN_POINT ( 'NONE',  ( 744.6391490659812007, -398.7363362996976548, 338.7502325331110455 ) ) ;
#8343 = DIRECTION ( 'NONE',  ( 0.000000000000000000, 0.000000000000000000, 1.000000000000000000 ) ) ;
#8344 = CARTESIAN_POINT ( 'NONE',  ( 787.4397851343537695, -357.7255117493285184, 374.2001403089903988 ) ) ;
#8345 = CARTESIAN_POINT ( 'NONE',  ( 774.6312213355099630, -311.3618753856922581, -364.6798772138717482 ) ) ;
#8346 = CARTESIAN_POINT ( 'NONE',  ( 800.7704444035546203, 19.83076734649410966, 326.0291762391768771 ) ) ;
#8347 = CARTESIAN_POINT ( 'NONE',  ( 752.7379699480933368, -60.00906357242598688, -361.9858362298580232 ) ) ;
#8348 = CARTESIAN_POINT ( 'NONE',  ( 799.4546378042377910, -105.0783235625964096, -356.1575198192848006 ) ) ;
#8349 = CARTESIAN_POINT ( 'NONE',  ( 745.1769319972822814, -137.8055962898690154, 346.2694204179732083 ) ) ;
#8350 = CARTESIAN_POINT ( 'NONE',  ( 756.5762568750052424, -435.1800572038737869, 348.7366044899774238 ) ) ;
#8351 = ADVANCED_FACE ( 'NONE', ( #2529 ), #13173, .F. ) ;
#8352 = CARTESIAN_POINT ( 'NONE',  ( 744.9990715423526808, -162.3510508353235196, 341.2370466360926002 ) ) ;
#8353 = CARTESIAN_POINT ( 'NONE',  ( 755.5713283507202505, -29.36187538569318178, -334.6858677611754729 ) ) ;
#8354 = CARTESIAN_POINT ( 'NONE',  ( 803.8651313633788504, -125.2601417444145255, -332.4468031744301015 ) ) ;
#8355 = CARTESIAN_POINT ( 'NONE',  ( 778.2165204200184689, -142.8164208402382656, -364.9363028652563230 ) ) ;
#8356 = CARTESIAN_POINT ( 'NONE',  ( 811.6461892240364477, 19.28531280103956647, -324.1737431748509835 ) ) ;
#8358 = CARTESIAN_POINT ( 'NONE',  ( 771.2633955100217236, -263.9073299311469327, 363.4237431249939618 ) ) ;
#8357 = CARTESIAN_POINT ( 'NONE',  ( 758.0580252608178853, -270.4527844766014937, 328.0187753319985404 ) ) ;
#8359 = AXIS2_PLACEMENT_3D ( 'NONE', #27637, #24392, #13562 ) ;
#8360 = DIRECTION ( 'NONE',  ( -1.000000000000000000, -0.000000000000000000, -0.000000000000000000 ) ) ;
#8361 = ORIENTED_EDGE ( 'NONE', *, *, #11177, .F. ) ;
#8362 = CARTESIAN_POINT ( 'NONE',  ( 790.8050863131179540, -452.8379544210779954, 362.5841948692291226 ) ) ;
#8363 = CARTESIAN_POINT ( 'NONE',  ( 784.0799538623451781, -371.8055962898682765, 364.6971507214555572 ) ) ;
#8364 = EDGE_LOOP ( 'NONE', ( #32742, #8997, #18827, #23046 ) ) ;
#8365 = CARTESIAN_POINT ( 'NONE',  ( 808.3070685750232087, -186.9982390220563104, 361.1904061080339829 ) ) ;
#8366 = CARTESIAN_POINT ( 'NONE',  ( 755.8894580844503253, -279.8272453906071746, 332.3691319403863531 ) ) ;
#8367 = CARTESIAN_POINT ( 'NONE',  ( 804.1601925771018387, -415.4419599262318457, 346.5483106153029098 ) ) ;
#8368 = ORIENTED_EDGE ( 'NONE', *, *, #26992, .F. ) ;
#8369 = CARTESIAN_POINT ( 'NONE',  ( 799.2566176426618085, -96.00906357242585898, -324.0069404352559559 ) ) ;
#8370 = CARTESIAN_POINT ( 'NONE',  ( 803.8556311672234642, -201.6237781080506863, 365.6418435158340117 ) ) ;
#8371 = CARTESIAN_POINT ( 'NONE',  ( 756.5762568750052424, -291.1800572038741848, -348.7366044899774238 ) ) ;
#8372 = ORIENTED_EDGE ( 'NONE', *, *, #15989, .F. ) ;
#8373 = CARTESIAN_POINT ( 'NONE',  ( 781.7834795799800531, -394.8164208402374697, -315.0636971347436202 ) ) ;
#8374 = CARTESIAN_POINT ( 'NONE',  ( 801.9419747391806368, -42.45278447660223264, -351.9812246680014027 ) ) ;
#8375 = AXIS2_PLACEMENT_3D ( 'NONE', #18878, #40110, #8473 ) ;
#8376 = EDGE_CURVE ( 'NONE', #8202, #17032, #41807, .T. ) ;
#8377 = CARTESIAN_POINT ( 'NONE',  ( 795.9930595647434757, -267.0783235625958696, 320.7433823573372820 ) ) ;
#8378 = LINE ( 'NONE', #12070, #36619 ) ;
#8379 = CARTESIAN_POINT ( 'NONE',  ( -775.4999999999993179, -512.9681489794448908, -327.9999999999999432 ) ) ;
#8380 = EDGE_CURVE ( 'NONE', #11197, #20161, #34853, .T. ) ;
#8381 = CARTESIAN_POINT ( 'NONE',  ( 778.7629533639073998, -8.736336299698871599, -375.0009284576466371 ) ) ;
#8382 = DIRECTION ( 'NONE',  ( 1.000000000000000000, 0.000000000000000000, 0.000000000000000000 ) ) ;
#8383 = VERTEX_POINT ( 'NONE', #27024 ) ;
#8384 = CARTESIAN_POINT ( 'NONE',  ( 764.1737431748507561, -322.3726999360615082, -371.6461892240376415 ) ) ;
#8385 = CARTESIAN_POINT ( 'NONE',  ( 747.6481478633932056, -181.0999726633347109, 353.4146539503763620 ) ) ;
#8387 = CARTESIAN_POINT ( 'NONE',  ( 803.6646147819161570, -305.9073299311467622, -348.8264449731210561 ) ) ;
#8386 = CARTESIAN_POINT ( 'NONE',  ( 989.9999999999992042, 50.81038600091411439, -193.6948738798775764 ) ) ;
#8388 = CARTESIAN_POINT ( 'NONE',  ( -858.8365100919713768, 230.0000000000001990, -199.9999999999881481 ) ) ;
#8389 = CARTESIAN_POINT ( 'NONE',  ( 761.4292242960306112, -137.4636090269711985, -323.2154366446414429 ) ) ;
#8390 = CARTESIAN_POINT ( 'NONE',  ( 801.1904061080336987, -20.08914811296592973, 368.3070685750235498 ) ) ;
#8391 = AXIS2_PLACEMENT_3D ( 'NONE', #19288, #44456, #16059 ) ;
#8392 = LINE ( 'NONE', #32654, #32058 ) ;
#8393 = CARTESIAN_POINT ( 'NONE',  ( 749.2812353651451076, -342.4527844766013231, -323.2262854647983090 ) ) ;
#8394 = DIRECTION ( 'NONE',  ( 0.000000000000000000, 0.000000000000000000, -1.000000000000000000 ) ) ;
#8395 = CARTESIAN_POINT ( 'NONE',  ( 794.9819416627830151, -36.99823902205679360, 319.9864689768909898 ) ) ;
#8396 = CIRCLE ( 'NONE', #31234, 10.00000000000006395 ) ;
#8397 = CARTESIAN_POINT ( 'NONE',  ( 750.9282345327678740, -280.9181544815162965, 319.8311093483690115 ) ) ;
#8398 = CARTESIAN_POINT ( 'NONE',  ( 781.2497674668890113, -252.3510508353232353, -375.3608509340180603 ) ) ;
#8399 = CARTESIAN_POINT ( 'NONE',  ( 814.2001403089898304, -257.3618753856924286, 347.4397851343538264 ) ) ;
#8400 = CARTESIAN_POINT ( 'NONE',  ( 812.6845335610512393, -439.9874144716862929, -353.5525998758768651 ) ) ;
#8401 = DIRECTION ( 'NONE',  ( 1.000000000000000000, -1.880165489482579047E-16, 0.000000000000000000 ) ) ;
#8402 = ORIENTED_EDGE ( 'NONE', *, *, #9997, .T. ) ;
#8403 = CARTESIAN_POINT ( 'NONE',  ( 765.0180583372156207, -360.9982390220557704, 360.0135310231089534 ) ) ;
#8404 = CARTESIAN_POINT ( 'NONE',  ( 760.7433823573367135, -84.00906357242590161, 355.9930595647440441 ) ) ;
#8405 = CARTESIAN_POINT ( 'NONE',  ( 793.2243759319678702, -2.532869017142183932, -318.4439275373583200 ) ) ;
#8406 = CARTESIAN_POINT ( 'NONE',  ( 794.9999999999993179, 205.0000000000000568, 255.0000000000000000 ) ) ;
#8407 = VECTOR ( 'NONE', #11396, 1000.000000000000000 ) ;
#8408 = LINE ( 'NONE', #40950, #10018 ) ;
#8409 = CARTESIAN_POINT ( 'NONE',  ( 815.0009284576459549, -126.3510508353236048, 338.7629533639073429 ) ) ;
#8410 = CARTESIAN_POINT ( 'NONE',  ( 805.1927285166397041, -400.8164208402373561, 341.8018195045277707 ) ) ;
#8411 = VERTEX_POINT ( 'NONE', #41123 ) ;
#8412 = CARTESIAN_POINT ( 'NONE',  ( 803.6646147819161570, -41.90732993114767169, -348.8264449731210561 ) ) ;
#8413 = CARTESIAN_POINT ( 'NONE',  ( 801.3366627262608972, -320.5328690171411949, -353.0897708529566899 ) ) ;
#8414 = CARTESIAN_POINT ( 'NONE',  ( 767.8955696845333705, -144.4527844766018632, 362.1676090361162323 ) ) ;
#8415 = CARTESIAN_POINT ( 'NONE',  ( 773.7943932421234194, -335.8055962898683902, -305.5313806188329409 ) ) ;
#8416 = DIRECTION ( 'NONE',  ( -0.000000000000000000, -0.000000000000000000, 1.000000000000000000 ) ) ;
#8417 = CARTESIAN_POINT ( 'NONE',  ( 813.9316612368132837, -439.4419599262316751, 348.6739635108323228 ) ) ;
#8418 = ORIENTED_EDGE ( 'NONE', *, *, #38068, .T. ) ;
#8419 = CARTESIAN_POINT ( 'NONE',  ( 804.4286716492782716, -353.3618753856922012, 345.3141322388244703 ) ) ;
#8420 = CARTESIAN_POINT ( 'NONE',  ( 804.9511171171677688, -77.80559628986920018, -335.8780910478229202 ) ) ;
#8421 = VERTEX_POINT ( 'NONE', #9476 ) ;
#8422 = CARTESIAN_POINT ( 'NONE',  ( 788.8264449731200330, -429.1800572038737869, 363.6646147819171233 ) ) ;
#8423 = CARTESIAN_POINT ( 'NONE',  ( 792.2312462859673587, -179.9073299311472454, -307.2067596250082602 ) ) ;
#8424 = ORIENTED_EDGE ( 'NONE', *, *, #20739, .T. ) ;
#8425 = AXIS2_PLACEMENT_3D ( 'NONE', #1264, #11884, #22492 ) ;
#8426 = CARTESIAN_POINT ( 'NONE',  ( 781.7834795799800531, -178.8164208402381519, -315.0636971347436202 ) ) ;
#8427 = VECTOR ( 'NONE', #39142, 1000.000000000000000 ) ;
#8428 = ORIENTED_EDGE ( 'NONE', *, *, #34615, .F. ) ;
#8429 = CARTESIAN_POINT ( 'NONE',  ( 786.5483106153019435, -439.6454272087884760, -364.1601925771022366 ) ) ;
#8430 = CARTESIAN_POINT ( 'NONE',  ( 804.4086373105744769, -457.6454272087884760, 333.3843516231986541 ) ) ;
#8431 = CARTESIAN_POINT ( 'NONE',  ( 792.2312462859673587, -227.9073299311471033, 307.2067596250082602 ) ) ;
#8432 = CARTESIAN_POINT ( 'NONE',  ( 799.4546378042377910, -153.0783235625962675, 356.1575198192848006 ) ) ;
#8434 = LINE ( 'NONE', #13487, #21842 ) ;
#8433 = CYLINDRICAL_SURFACE ( 'NONE', #15915, 2.749999999999863665 ) ;
#8435 = EDGE_LOOP ( 'NONE', ( #7509, #5329, #24034, #10191 ) ) ;
#8436 = CARTESIAN_POINT ( 'NONE',  ( 790.9844846989617508, -430.3726999360611671, -317.2208543904092721 ) ) ;
#8437 = CARTESIAN_POINT ( 'NONE',  ( 181.1634899080285948, 256.5000000000000000, -199.9999999999953957 ) ) ;
#8438 = CARTESIAN_POINT ( 'NONE',  ( 762.1177392798416577, -186.5545181178801215, -309.8865473780659272 ) ) ;
#8439 = CARTESIAN_POINT ( 'NONE',  ( 783.7953271457878373, -80.19088175424411702, 375.1787889125761239 ) ) ;
#8441 = CARTESIAN_POINT ( 'NONE',  ( 774.6858677611749044, -201.7255117493290015, -315.5713283507209894 ) ) ;
#8440 = LINE ( 'NONE', #22510, #40123 ) ;
#8442 = CARTESIAN_POINT ( 'NONE',  ( 804.9511171171677688, -317.8055962898684470, -335.8780910478229202 ) ) ;
#8443 = DIRECTION ( 'NONE',  ( -1.000000000000000000, -0.000000000000000000, -0.000000000000000000 ) ) ;
#8444 = CARTESIAN_POINT ( 'NONE',  ( 791.0478386215596629, -237.8272453906072599, -306.7653713866226326 ) ) ;
#8445 = DIRECTION ( 'NONE',  ( -0.000000000000000000, 1.000000000000000000, -0.000000000000000000 ) ) ;
#8446 = FACE_BOUND ( 'NONE', #28078, .T. ) ;
#8447 = CARTESIAN_POINT ( 'NONE',  ( 784.1219089521767955, -45.28179084515329578, -315.0488828828318333 ) ) ;
#8448 = CARTESIAN_POINT ( 'NONE',  ( 800.9840315886518738, -388.9181544815158986, 354.1144889064786412 ) ) ;
#8449 = AXIS2_PLACEMENT_3D ( 'NONE', #31791, #18190, #14725 ) ;
#8450 = CARTESIAN_POINT ( 'NONE',  ( 792.3570229623691148, -237.1800572038742985, -373.1304606946836770 ) ) ;
#8451 = LINE ( 'NONE', #5889, #44550 ) ;
#8452 = CARTESIAN_POINT ( 'NONE',  ( 800.2193346964447755, -18.99823902205683979, -355.1360043628815788 ) ) ;
#8453 = CARTESIAN_POINT ( 'NONE',  ( 748.6759233522253680, -184.3726999360619629, 324.3348316497537098 ) ) ;
#8454 = CARTESIAN_POINT ( 'NONE',  ( 781.2497674668890113, -132.3510508353235764, -375.3608509340180603 ) ) ;
#8455 = CARTESIAN_POINT ( 'NONE',  ( 796.7737145352015204, -140.6346026584201070, 370.7187646348536987 ) ) ;
#8456 = CARTESIAN_POINT ( 'NONE',  ( 800.9747183278959710, -372.9982390220557704, -311.9810565676471583 ) ) ;
#8457 = LINE ( 'NONE', #22761, #43829 ) ;
#8458 = DIRECTION ( 'NONE',  ( 1.000000000000000000, 0.000000000000000000, 0.000000000000000000 ) ) ;
#8459 = CIRCLE ( 'NONE', #34244, 10.00000000000006395 ) ;
#8460 = CARTESIAN_POINT ( 'NONE',  ( 792.1044303154645831, -228.4527844766015789, 317.8323909638837677 ) ) ;
#8461 = CIRCLE ( 'NONE', #1771, 10.00000000000000888 ) ;
#8462 = CARTESIAN_POINT ( 'NONE',  ( 755.1538015810308480, -14.19088175424431242, 343.0433043558613804 ) ) ;
#8463 = CARTESIAN_POINT ( 'NONE',  ( 803.6646147819161570, -401.9073299311463643, -348.8264449731210561 ) ) ;
#8464 = VECTOR ( 'NONE', #10258, 1000.000000000000000 ) ;
#8465 = CARTESIAN_POINT ( 'NONE',  ( 802.2119215644370342, -6.009063572426154742, -367.5423716828165084 ) ) ;
#8466 = LINE ( 'NONE', #12603, #26916 ) ;
#8467 = CARTESIAN_POINT ( 'NONE',  ( 803.8556311672234642, -33.62377810805116951, 365.6418435158340117 ) ) ;
#8468 = CARTESIAN_POINT ( 'NONE',  ( 803.4237431249931660, -303.1800572038740711, 331.2633955100225194 ) ) ;
#8469 = ORIENTED_EDGE ( 'NONE', *, *, #42688, .F. ) ;
#8470 = CARTESIAN_POINT ( 'NONE',  ( 786.6156483768007774, -241.4419599262322720, -315.5913626894246136 ) ) ;
#8471 = CARTESIAN_POINT ( 'NONE',  ( 778.1981804954714335, -10.27096629478414691, 314.8072714833589885 ) ) ;
#8472 = CARTESIAN_POINT ( 'NONE',  ( 788.7631598425961101, -217.4419599262324141, -305.7194118038759143 ) ) ;
#8473 = DIRECTION ( 'NONE',  ( 1.000000000000000000, 0.000000000000000000, 0.000000000000000000 ) ) ;
#8474 = CARTESIAN_POINT ( 'NONE',  ( 783.7566961878529810, -360.8965053807773984, 305.1792804349288417 ) ) ;
#8475 = CARTESIAN_POINT ( 'NONE',  ( 764.8639956371174549, -80.08914811296574499, -319.7806653035542013 ) ) ;
#8476 = VERTEX_POINT ( 'NONE', #33204 ) ;
#8477 = CIRCLE ( 'NONE', #20263, 9.999999999999982236 ) ;
#8478 = CARTESIAN_POINT ( 'NONE',  ( 793.4146539503750546, -433.9874144716862361, 307.6481478633938877 ) ) ;
#8479 = CARTESIAN_POINT ( 'NONE',  ( 792.1044303154645831, -348.4527844766012663, 317.8323909638837677 ) ) ;
#8480 = AXIS2_PLACEMENT_3D ( 'NONE', #5426, #19300, #15612 ) ;
#8481 = CARTESIAN_POINT ( 'NONE',  ( 763.0537975583475827, -72.45278447660213317, -371.0346526505627480 ) ) ;
#8482 = CARTESIAN_POINT ( 'NONE',  ( 781.8018195045267476, -70.27096629478397460, -365.1927285166407273 ) ) ;
#8483 = ORIENTED_EDGE ( 'NONE', *, *, #44416, .T. ) ;
#8484 = CARTESIAN_POINT ( 'NONE',  ( 766.9102291470427417, 5.445481882119263872, -318.6633372737382501 ) ) ;
#8485 = EDGE_LOOP ( 'NONE', ( #43181, #42102 ) ) ;
#8486 = CARTESIAN_POINT ( 'NONE',  ( 755.8894580844503253, -327.8272453906069472, -332.3691319403863531 ) ) ;
#8488 = CARTESIAN_POINT ( 'NONE',  ( 763.8424801807145741, -378.0090635724250774, 320.5453621957614700 ) ) ;
#8487 = CARTESIAN_POINT ( 'NONE',  ( 785.3687786644884454, -59.36187538569306810, 315.3201227861279676 ) ) ;
#8489 = CARTESIAN_POINT ( 'NONE',  ( 785.3141322388236176, -309.7255117493287457, -364.4286716492789537 ) ) ;
#8492 = CARTESIAN_POINT ( 'NONE',  ( 749.8865473780648472, -332.5328690171411381, 322.1177392798429082 ) ) ;
#8491 = CARTESIAN_POINT ( 'NONE',  ( 200.7583438952259485, 394.6698570112193920, -244.9999999999999716 ) ) ;
#8490 = CARTESIAN_POINT ( 'NONE',  ( 763.2262854647970016, -440.6346026584191122, 309.2812353651462445 ) ) ;
#8493 = VECTOR ( 'NONE', #20143, 999.9999999999998863 ) ;
#8494 = CARTESIAN_POINT ( 'NONE',  ( 800.9840315886518738, -316.9181544815160692, -354.1144889064786412 ) ) ;
#8495 = CARTESIAN_POINT ( 'NONE',  ( 756.3353852180819104, -293.9073299311468759, -331.1735550268788302 ) ) ;
#8496 = CARTESIAN_POINT ( 'NONE',  ( 755.0636971347428243, -148.2709662947837330, -341.7834795799807353 ) ) ;
#8497 = EDGE_CURVE ( 'NONE', #5810, #24407, #30400, .T. ) ;
#8498 = CIRCLE ( 'NONE', #26184, 6.118999999999985562 ) ;
#8499 = FACE_OUTER_BOUND ( 'NONE', #23837, .T. ) ;
#8500 = CARTESIAN_POINT ( 'NONE',  ( 763.0537975583475827, -432.4527844766008684, 371.0346526505627480 ) ) ;
#8501 = AXIS2_PLACEMENT_3D ( 'NONE', #29131, #4431, #42984 ) ;
#8503 = CARTESIAN_POINT ( 'NONE',  ( 265.7583438952258916, -600.0000000000000000, -244.9999999999999716 ) ) ;
#8502 = LINE ( 'NONE', #660, #14523 ) ;
#8504 = CARTESIAN_POINT ( 'NONE',  ( 807.2620300519052989, -72.00906357242594424, -318.0141637701419768 ) ) ;
#8505 = DIRECTION ( 'NONE',  ( 0.000000000000000000, 0.000000000000000000, 1.000000000000000000 ) ) ;
#8506 = DIRECTION ( 'NONE',  ( 0.000000000000000000, 0.000000000000000000, 1.000000000000000000 ) ) ;
#8507 = CARTESIAN_POINT ( 'NONE',  ( 757.4527132478984868, -280.3726999360616787, 329.1273215169538844 ) ) ;
#8508 = CARTESIAN_POINT ( 'NONE',  ( 756.3353852180819104, -173.9073299311472169, 331.1735550268788302 ) ) ;
#8509 = VERTEX_POINT ( 'NONE', #44494 ) ;
#8510 = CIRCLE ( 'NONE', #24705, 10.00000000000006395 ) ;
#8511 = CARTESIAN_POINT ( 'NONE',  ( 751.9810565676468741, -122.0891481129656171, -360.9747183278973921 ) ) ;
#8512 = CARTESIAN_POINT ( 'NONE',  ( 760.5453621957607311, -333.0783235625956991, 323.8424801807151425 ) ) ;
#8513 = AXIS2_PLACEMENT_3D ( 'NONE', #33182, #37310, #23440 ) ;
#8514 = CARTESIAN_POINT ( 'NONE',  ( 747.6481478633932056, -85.09997266333499510, 353.4146539503763620 ) ) ;
#8515 = CARTESIAN_POINT ( 'NONE',  ( 749.2812353651451076, -270.4527844766014937, -323.2262854647983090 ) ) ;
#8516 = AXIS2_PLACEMENT_3D ( 'NONE', #36131, #25731, #28267 ) ;
#8517 = PLANE ( 'NONE',  #21757 ) ;
#8518 = CARTESIAN_POINT ( 'NONE',  ( 767.8955696845333705, -120.4527844766019484, 362.1676090361162323 ) ) ;
#8519 = EDGE_LOOP ( 'NONE', ( #8649, #23157, #36994, #27053 ) ) ;
#8520 = CARTESIAN_POINT ( 'NONE',  ( 811.6461892240364477, -340.7146871989592114, -324.1737431748509835 ) ) ;
#8521 = CARTESIAN_POINT ( 'NONE',  ( 792.2312462859673587, -83.90732993114754379, -307.2067596250082602 ) ) ;
#8522 = CARTESIAN_POINT ( 'NONE',  ( 787.5531968255692163, -21.82724539060792424, 316.1348686366205811 ) ) ;
#8523 = CARTESIAN_POINT ( 'NONE',  ( 745.0891759886404770, -340.2709662947831362, -342.4968714119734159 ) ) ;
#8524 = CYLINDRICAL_SURFACE ( 'NONE', #24641, 2.749999999999863665 ) ;
#8525 = CARTESIAN_POINT ( 'NONE',  ( 772.3691319403857278, -407.2601417444137155, 315.8894580844506663 ) ) ;
#8526 = VERTEX_POINT ( 'NONE', #34086 ) ;
#8527 = CARTESIAN_POINT ( 'NONE',  ( 765.0180583372156207, -432.9982390220555999, -360.0135310231089534 ) ) ;
#8528 = CARTESIAN_POINT ( 'NONE',  ( 758.0580252608178853, -222.4527844766016642, -328.0187753319985404 ) ) ;
#8529 = CIRCLE ( 'NONE', #38040, 8.024999999999948841 ) ;
#8530 = CARTESIAN_POINT ( 'NONE',  ( 810.1134526219336749, -104.5328690171418913, -357.8822607201570349 ) ) ;
#8531 = CARTESIAN_POINT ( 'NONE',  ( 454.7528517110261532, -8.550106180308601742E-14, 339.9999999999999432 ) ) ;
#8532 = CARTESIAN_POINT ( 'NONE',  ( 744.8212110874229666, -234.8965053807777963, 336.2046728542121627 ) ) ;
#8533 = CARTESIAN_POINT ( 'NONE',  ( 788.7366044899766848, -35.90732993114770011, 316.5762568750059813 ) ) ;
#8534 = CARTESIAN_POINT ( 'NONE',  ( 803.2186876482843445, -247.9874144716867761, -350.0220218866286928 ) ) ;
#8535 = CARTESIAN_POINT ( 'NONE',  ( 764.8639956371174549, -224.0891481129653187, 319.7806653035542013 ) ) ;
#8536 = CARTESIAN_POINT ( 'NONE',  ( 787.5162901302840055, 12.63812461430668321, -305.4481719005792684 ) ) ;
#8537 = CARTESIAN_POINT ( 'NONE',  ( 778.7502325331095108, -72.35105083532378956, -304.6391490659818828 ) ) ;
#8538 = CYLINDRICAL_SURFACE ( 'NONE', #43823, 20.00000000000004974 ) ;
#8539 = ORIENTED_EDGE ( 'NONE', *, *, #35945, .T. ) ;
#8540 = ORIENTED_EDGE ( 'NONE', *, *, #1014, .F. ) ;
#8541 = CARTESIAN_POINT ( 'NONE',  ( 805.6418435158337843, -389.4636090269704027, -363.8556311672236916 ) ) ;
#8542 = COLOUR_RGB ( '',0.7921568627450980005, 0.8196078431372548767, 0.9333333333333333481 ) ;
#8543 = CARTESIAN_POINT ( 'NONE',  ( 802.1676090361156639, -230.6346026584197659, -327.8955696845344505 ) ) ;
#8544 = ADVANCED_FACE ( 'NONE', ( #26017 ), #2452, .F. ) ;
#8545 = VECTOR ( 'NONE', #33355, 1000.000000000000000 ) ;
#8546 = CARTESIAN_POINT ( 'NONE',  ( 767.7687537140311633, -335.9073299311468190, 372.7932403749916830 ) ) ;
#8547 = CARTESIAN_POINT ( 'NONE',  ( 754.0944755984390895, -39.62377810805116951, 364.1009440267246760 ) ) ;
#8548 = CARTESIAN_POINT ( 'NONE',  ( 755.1538015810308480, -206.1908817542437191, -343.0433043558613804 ) ) ;
#8549 = CARTESIAN_POINT ( 'NONE',  ( 756.5762568750052424, -195.1800572038744974, -348.7366044899774238 ) ) ;
#8551 = AXIS2_PLACEMENT_3D ( 'NONE', #31338, #30662, #24178 ) ;
#8550 = CARTESIAN_POINT ( 'NONE',  ( 755.3201227861273992, -387.7255117493284047, -345.3687786644892981 ) ) ;
#8552 = ORIENTED_EDGE ( 'NONE', *, *, #13735, .F. ) ;
#8553 = CARTESIAN_POINT ( 'NONE',  ( 771.1735550268778070, -225.1800572038743269, 316.3353852180827630 ) ) ;
#8554 = CARTESIAN_POINT ( 'NONE',  ( 800.7704444035546203, 19.83076734649410966, -326.0291762391768771 ) ) ;
#8555 = ORIENTED_EDGE ( 'NONE', *, *, #18304, .F. ) ;
#8556 = CARTESIAN_POINT ( 'NONE',  ( 792.3570229623688874, -333.1800572038740142, 373.1304606946836202 ) ) ;
#8557 = CARTESIAN_POINT ( 'NONE',  ( 1820.038553321469863, 240.0000000000001990, -201.9999999999999716 ) ) ;
#8558 = CARTESIAN_POINT ( 'NONE',  ( 914.9999999999992042, 74.99999999999984368, 350.0000000000000000 ) ) ;
#8559 = FACE_OUTER_BOUND ( 'NONE', #13422, .T. ) ;
#8560 = CARTESIAN_POINT ( 'NONE',  ( 772.4468031744293057, -201.8272453906073451, 363.8651313633793620 ) ) ;
#8561 = CARTESIAN_POINT ( 'NONE',  ( 785.3141322388236176, -45.72551174932949181, 364.4286716492789537 ) ) ;
#8562 = EDGE_LOOP ( 'NONE', ( #27846, #24077, #27537, #18545 ) ) ;
#8563 = CARTESIAN_POINT ( 'NONE',  ( 810.4231160770870019, -408.5545181178794110, -321.9338519418446936 ) ) ;
#8564 = CARTESIAN_POINT ( 'NONE',  ( 782.4968714119720516, -34.81642084023861372, -305.0891759886411023 ) ) ;
#8565 = CARTESIAN_POINT ( 'NONE',  ( 775.9200461376533440, -239.8055962898687028, 315.3028492785443291 ) ) ;
#8566 = VECTOR ( 'NONE', #27340, 1000.000000000000000 ) ;
#8567 = CARTESIAN_POINT ( 'NONE',  ( 774.6312213355099630, -383.3618753856921444, -364.6798772138717482 ) ) ;
#8568 = CARTESIAN_POINT ( 'NONE',  ( 804.4286716492782716, -17.36187538569322086, -345.3141322388244703 ) ) ;
#8569 = CARTESIAN_POINT ( 'NONE',  ( 767.6429770376289525, -417.1800572038736163, 306.8695393053162093 ) ) ;
#8570 = DIRECTION ( 'NONE',  ( -1.880165489482579047E-16, -1.000000000000000000, -0.000000000000000000 ) ) ;
#8571 = CIRCLE ( 'NONE', #15834, 9.999999999999982236 ) ;
#8572 = CARTESIAN_POINT ( 'NONE',  ( 780.5236548040995785, -260.7363362996981095, -314.9735926884559944 ) ) ;
#8574 = AXIS2_PLACEMENT_3D ( 'NONE', #11453, #25536, #42643 ) ;
#8573 = CARTESIAN_POINT ( 'NONE',  ( 792.3570229623688874, -165.1800572038745258, -373.1304606946836202 ) ) ;
#8575 = CARTESIAN_POINT ( 'NONE',  ( 751.6929314249748586, -54.99823902205672255, 318.8095938919659034 ) ) ;
#8576 = CARTESIAN_POINT ( 'NONE',  ( 810.7187646348534145, -114.4527844766020053, 356.7737145352016341 ) ) ;
#8577 = DIRECTION ( 'NONE',  ( -1.000000000000000000, 0.000000000000000000, 0.000000000000000000 ) ) ;
#8578 = CARTESIAN_POINT ( 'NONE',  ( 181.1634899080285948, 256.5000000000000000, -199.9999999999953957 ) ) ;
#8579=STYLED_ITEM('',(#45758),#32652);
#8580 = CARTESIAN_POINT ( 'NONE',  ( -786.4999999999993179, -513.1383975375929367, -349.9999999999999432 ) ) ;
#8581 = CARTESIAN_POINT ( 'NONE',  ( 745.7998596910086917, -365.3618753856920875, 332.5602148656461168 ) ) ;
#8582 = CARTESIAN_POINT ( 'NONE',  ( 805.1927285166397041, -328.8164208402375834, -341.8018195045277707 ) ) ;
#8583 = AXIS2_PLACEMENT_3D ( 'NONE', #44558, #33473, #26541 ) ;
#8584 = CARTESIAN_POINT ( 'NONE',  ( 786.6156483768007774, 22.55804007376682918, 315.5913626894246136 ) ) ;
#8585 = CARTESIAN_POINT ( 'NONE',  ( 771.3260364891663130, -91.64542720878951343, -306.0683387631859773 ) ) ;
#8586 = CARTESIAN_POINT ( 'NONE',  ( 779.4709603349208464, -120.3510508353236048, -314.7162404726379918 ) ) ;
#8587 = CARTESIAN_POINT ( 'NONE',  ( 744.9990715423526808, -138.3510508353236048, 341.2370466360926002 ) ) ;
#8588 = CARTESIAN_POINT ( 'NONE',  ( 771.2633955100217236, -431.9073299311464211, 363.4237431249939618 ) ) ;
#8589 = CARTESIAN_POINT ( 'NONE',  ( 757.8323909638827445, -26.63460265842045871, -352.1044303154654358 ) ) ;
#8590 = CARTESIAN_POINT ( 'NONE',  ( 754.8983024940795303, -138.8965053807781374, -336.9254006560228163 ) ) ;
#8591 = CARTESIAN_POINT ( 'NONE',  ( 785.3687786644884454, -131.3618753856928834, -315.3201227861279676 ) ) ;
#8592 = CARTESIAN_POINT ( 'NONE',  ( 801.9419747391806368, -114.4527844766020053, 351.9812246680014027 ) ) ;
#8593 = EDGE_CURVE ( 'NONE', #27904, #34950, #23464, .T. ) ;
#8594 = CARTESIAN_POINT ( 'NONE',  ( 766.7756240680305382, -422.5328690171408539, -361.5560724626415663 ) ) ;
#8596 = CARTESIAN_POINT ( 'NONE',  ( 778.2165204200184689, -262.8164208402379245, 364.9363028652563230 ) ) ;
#8595 = CARTESIAN_POINT ( 'NONE',  ( 778.1981804954714335, -250.2709662947832783, 314.8072714833589885 ) ) ;
#8597 = CARTESIAN_POINT ( 'NONE',  ( 1007.605605532488426, -434.0043448692482002, 397.6917108626901154 ) ) ;
#8598 = EDGE_LOOP ( 'NONE', ( #42155, #35681, #19053, #21427 ) ) ;
#8599 = CARTESIAN_POINT ( 'NONE',  ( 764.0069404352550464, 8.921676437403235127, 359.2566176426627180 ) ) ;
#8600 = CARTESIAN_POINT ( 'NONE',  ( 802.2119215644370342, -270.0090635724253048, -367.5423716828165084 ) ) ;
#8601 = ORIENTED_EDGE ( 'NONE', *, *, #23000, .T. ) ;
#8602 =( NAMED_UNIT ( * ) PLANE_ANGLE_UNIT ( ) SI_UNIT ( $, .RADIAN. ) );
#8603 = AXIS2_PLACEMENT_3D ( 'NONE', #22949, #33821, #30575 ) ;
#8604 = EDGE_CURVE ( 'NONE', #17065, #23212, #29206, .T. ) ;
#8605 = CARTESIAN_POINT ( 'NONE',  ( 782.4968714119720516, -202.8164208402380950, 305.0891759886411023 ) ) ;
#8606 = CARTESIAN_POINT ( 'NONE',  ( 786.5483106153019435, -295.6454272087888739, 364.1601925771022366 ) ) ;
#8607 = CARTESIAN_POINT ( 'NONE',  ( 765.8855110935204493, -406.1692326535045368, 319.0159684113471599 ) ) ;
#8608 = VERTEX_POINT ( 'NONE', #44736 ) ;
#8609 = CARTESIAN_POINT ( 'NONE',  ( 769.0155153010367712, -82.37269993606227558, -362.7791456095907279 ) ) ;
#8610 = CARTESIAN_POINT ( 'NONE',  ( 765.0180583372156207, -288.9982390220559978, -360.0135310231089534 ) ) ;
#8611 = ORIENTED_EDGE ( 'NONE', *, *, #36003, .F. ) ;
#8612 = CARTESIAN_POINT ( 'NONE',  ( 795.1360043628807261, -380.0891481129646650, -360.2193346964456282 ) ) ;
#8613 = CARTESIAN_POINT ( 'NONE',  ( 794.9819416627830151, -36.99823902205679360, -319.9864689768909898 ) ) ;
#8614 = CARTESIAN_POINT ( 'NONE',  ( 761.2382568024794409, -255.6237781080504874, 356.9571628226838129 ) ) ;
#8615 = CYLINDRICAL_SURFACE ( 'NONE', #43985, 6.118999999999985562 ) ;
#8616 = DIRECTION ( 'NONE',  ( -0.000000000000000000, 1.000000000000000000, -0.000000000000000000 ) ) ;
#8617 = VECTOR ( 'NONE', #42914, 1000.000000000000000 ) ;
#8618 = CARTESIAN_POINT ( 'NONE',  ( 812.3518521366052028, -25.09997266333519050, -326.5853460496235243 ) ) ;
#8619 = CARTESIAN_POINT ( 'NONE',  ( -829.9999999999992042, -600.0000000000000000, -244.9999999999995168 ) ) ;
#8620 = ORIENTED_EDGE ( 'NONE', *, *, #2576, .T. ) ;
#8621 = CARTESIAN_POINT ( 'NONE',  ( 749.5768839229115201, -324.5545181178796952, -358.0661480581553064 ) ) ;
#8622 = EDGE_CURVE ( 'NONE', #30100, #16583, #5920, .T. ) ;
#8623 = CARTESIAN_POINT ( 'NONE',  ( 752.7379699480933368, -180.0090635724255890, 361.9858362298580232 ) ) ;
#8625 = CARTESIAN_POINT ( 'NONE',  ( 797.8594530101008786, -277.5436935675105019, -322.1405469898980982 ) ) ;
#8624 = PLANE ( 'NONE',  #26813 ) ;
#8626 = EDGE_CURVE ( 'NONE', #28228, #42107, #22562, .T. ) ;
#8627 = DIRECTION ( 'NONE',  ( -1.880165489482579047E-16, -1.000000000000000000, -0.000000000000000000 ) ) ;
#8628 = CARTESIAN_POINT ( 'NONE',  ( 790.9844846989617508, -166.3726999360620198, -317.2208543904092721 ) ) ;
#8629 = CARTESIAN_POINT ( 'NONE',  ( 751.6929314249748586, -6.998239022056885972, 318.8095938919659034 ) ) ;
#8630 = LINE ( 'NONE', #19232, #4047 ) ;
#8631 = CARTESIAN_POINT ( 'NONE',  ( 796.7737145352015204, -332.6346026584195101, -370.7187646348536987 ) ) ;
#8632 = CYLINDRICAL_SURFACE ( 'NONE', #6231, 10.00000000000000888 ) ;
#8633 = CARTESIAN_POINT ( 'NONE',  ( 803.6646147819161570, -41.90732993114767169, 348.8264449731210561 ) ) ;
#8634 = CARTESIAN_POINT ( 'NONE',  ( 783.7953271457878373, -296.1908817542434917, 375.1787889125761239 ) ) ;
#8635 = CARTESIAN_POINT ( 'NONE',  ( 767.6429770376289525, -273.1800572038742985, 306.8695393053162093 ) ) ;
#8636 = CARTESIAN_POINT ( 'NONE',  ( 814.8230680027162407, -437.8055962898679923, -333.7305795820267917 ) ) ;
#8637 = CIRCLE ( 'NONE', #38879, 8.025000000000003908 ) ;
#8638 = FACE_BOUND ( 'NONE', #21534, .T. ) ;
#8639 = ORIENTED_EDGE ( 'NONE', *, *, #32957, .T. ) ;
#8640 = CARTESIAN_POINT ( 'NONE',  ( 764.8639956371174549, -344.0891481129647786, 319.7806653035542013 ) ) ;
#8641 = CONICAL_SURFACE ( 'NONE', #19593, 8.025000000000003908, 0.7853981633974482790 ) ;
#8642 = CARTESIAN_POINT ( 'NONE',  ( 755.1538015810308480, -110.1908817542440033, 343.0433043558613804 ) ) ;
#8643 = CARTESIAN_POINT ( 'NONE',  ( 803.2186876482843445, -7.987414471687621642, -350.0220218866286928 ) ) ;
#8644 = AXIS2_PLACEMENT_3D ( 'NONE', #7476, #35628, #32182 ) ;
#8645 = DIRECTION ( 'NONE',  ( 1.000000000000000000, 0.000000000000000000, 0.000000000000000000 ) ) ;
#8646 = EDGE_CURVE ( 'NONE', #16202, #3030, #26934, .T. ) ;
#8647 = CARTESIAN_POINT ( 'NONE',  ( -728.8365100919714905, 260.0000000000001705, -199.9999999999890861 ) ) ;
#8648 = CARTESIAN_POINT ( 'NONE',  ( 755.0636971347428243, -388.2709662947829656, 341.7834795799807353 ) ) ;
#8649 = ORIENTED_EDGE ( 'NONE', *, *, #6020, .F. ) ;
#8650 = ADVANCED_FACE ( 'NONE', ( #37563 ), #19548, .F. ) ;
#8651 = CARTESIAN_POINT ( 'NONE',  ( 758.6633372737375112, -332.5328690171411381, -326.9102291470432533 ) ) ;
#8652 = CARTESIAN_POINT ( 'NONE',  ( 797.8594530101008786, -157.5436935675108998, 322.1405469898980982 ) ) ;
#8653 = CARTESIAN_POINT ( 'NONE',  ( 795.6651683502461765, -322.7146871989593819, -371.3240766477733814 ) ) ;
#8654 = CARTESIAN_POINT ( 'NONE',  ( -26.63011601220122060, -512.9681489794448908, -329.9999999999999432 ) ) ;
#8655 = ORIENTED_EDGE ( 'NONE', *, *, #8659, .T. ) ;
#8656 = CARTESIAN_POINT ( 'NONE',  ( 785.3141322388236176, -357.7255117493285184, 364.4286716492789537 ) ) ;
#8657 = ORIENTED_EDGE ( 'NONE', *, *, #42213, .T. ) ;
#8658 = CARTESIAN_POINT ( 'NONE',  ( 771.1735550268778070, -441.1800572038735027, 316.3353852180827630 ) ) ;
#8659 = EDGE_CURVE ( 'NONE', #7675, #10891, #20010, .T. ) ;
#8660 = EDGE_CURVE ( 'NONE', #1029, #5066, #44036, .T. ) ;
#8661 = CARTESIAN_POINT ( 'NONE',  ( 815.2698199232961542, -184.8164208402380950, -342.5225473063383106 ) ) ;
#8662 = CARTESIAN_POINT ( 'NONE',  ( 787.5162901302840055, -83.36187538569299704, 305.4481719005793252 ) ) ;
#8663 = EDGE_LOOP ( 'NONE', ( #22933, #43468, #1007, #24998 ) ) ;
#8664 = CARTESIAN_POINT ( 'NONE',  ( 765.0180583372156207, -168.9982390220563673, -360.0135310231089534 ) ) ;
#8665 = ORIENTED_EDGE ( 'NONE', *, *, #17723, .T. ) ;
#8666 = VECTOR ( 'NONE', #20195, 1000.000000000000000 ) ;
#8667 = CARTESIAN_POINT ( 'NONE',  ( 779.4763451958990572, -416.7363362996975980, -365.0264073115438919 ) ) ;
#8668 = CARTESIAN_POINT ( 'NONE',  ( 785.3141322388236176, 2.274488250670355871, 364.4286716492789537 ) ) ;
#8669 = CARTESIAN_POINT ( 'NONE',  ( 801.1904061080336987, -260.0891481129650060, 368.3070685750235498 ) ) ;
#8670 = CARTESIAN_POINT ( 'NONE',  ( 794.1144889064781864, -154.1692326535053894, 360.9840315886528401 ) ) ;
#8672 = DIRECTION ( 'NONE',  ( 0.000000000000000000, 0.000000000000000000, 1.000000000000000000 ) ) ;
#8671 = CARTESIAN_POINT ( 'NONE',  ( 779.9999999999992042, -462.9681489794448339, -339.9999999999999432 ) ) ;
#8673 = ORIENTED_EDGE ( 'NONE', *, *, #42479, .F. ) ;
#8674 = CARTESIAN_POINT ( 'NONE',  ( 776.9254006560222479, -428.1908817542430938, -314.8983024940802125 ) ) ;
#8675 = CYLINDRICAL_SURFACE ( 'NONE', #29984, 7.999999999999896083 ) ;
#8676 = CARTESIAN_POINT ( 'NONE',  ( 754.3581564841646241, -209.4636090269709996, -316.1443688327762516 ) ) ;
#8677 = CARTESIAN_POINT ( 'NONE',  ( 768.9521613784389729, -57.82724539060780700, 373.2346286133773106 ) ) ;
#8678 = CIRCLE ( 'NONE', #24148, 2.749999999999863665 ) ;
#8680 = CARTESIAN_POINT ( 'NONE',  ( 804.6798772138708955, -183.7255117493290015, -334.6312213355107019 ) ) ;
#8679 = LINE ( 'NONE', #22743, #12814 ) ;
#8681 = CARTESIAN_POINT ( 'NONE',  ( 804.1601925771018387, -343.4419599262320162, -346.5483106153029098 ) ) ;
#8682 = DIRECTION ( 'NONE',  ( -1.000000000000000000, -0.000000000000000000, -0.000000000000000000 ) ) ;
#8683 = CARTESIAN_POINT ( 'NONE',  ( 766.4474001241216001, -235.0999726633344835, -307.3154664389482491 ) ) ;
#8684 = LINE ( 'NONE', #26884, #6811 ) ;
#8685 = CARTESIAN_POINT ( 'NONE',  ( 180.7583438952258348, 394.6698570112193920, -224.9999999999999716 ) ) ;
#8686 = CARTESIAN_POINT ( 'NONE',  ( 775.8780910478218402, -57.28179084515326736, -364.9511171171680530 ) ) ;
#8687 = CARTESIAN_POINT ( 'NONE',  ( 804.1105419155481968, -387.8272453906067767, 347.6308680596136469 ) ) ;
#8688 = CARTESIAN_POINT ( 'NONE',  ( 787.4397851343537695, -237.7255117493289163, -374.2001403089903988 ) ) ;
#8689 = CARTESIAN_POINT ( 'NONE',  ( 796.9571628226829034, -239.4636090269709143, 321.2382568024804641 ) ) ;
#8690 = DIRECTION ( 'NONE',  ( 0.000000000000000000, -0.6755902076156505842, -0.7372773368101327440 ) ) ;
#8691 = CARTESIAN_POINT ( 'NONE',  ( 791.9812246680005501, -20.63460265842048003, -361.9419747391813189 ) ) ;
#8692 = CARTESIAN_POINT ( 'NONE',  ( 791.0478386215596629, -189.8272453906073736, 306.7653713866226326 ) ) ;
#8693 = CARTESIAN_POINT ( 'NONE',  ( 759.8311093483677041, -142.1692326535054178, -310.9282345327691814 ) ) ;
#8694 = CARTESIAN_POINT ( 'NONE',  ( 772.5602148656447525, -153.7255117493291721, 305.7998596910095443 ) ) ;
#8695 = CARTESIAN_POINT ( 'NONE',  ( 744.7301800767019131, -388.8164208402374129, -337.4774526936615757 ) ) ;
#8696 = CARTESIAN_POINT ( 'NONE',  ( 799.9999999999993179, 205.0000000000000568, 245.0000000000000284 ) ) ;
#8697 = DIRECTION ( 'NONE',  ( 1.000000000000000000, -0.000000000000000000, -0.000000000000000000 ) ) ;
#8698 = CARTESIAN_POINT ( 'NONE',  ( 804.6798772138708955, -255.7255117493287742, 334.6312213355107019 ) ) ;
#8699 = CARTESIAN_POINT ( 'NONE',  ( 780.5236548040995785, -20.73633629969883430, 314.9735926884559944 ) ) ;
#8700 = CARTESIAN_POINT ( 'NONE',  ( 804.9363028652555840, -376.2709662947829656, -338.2165204200192079 ) ) ;
#8701 = CARTESIAN_POINT ( 'NONE',  ( 939.9999999999992042, 240.0000000000000568, 201.9999999999999716 ) ) ;
#8702 = CARTESIAN_POINT ( 'NONE',  ( 808.0189434323515343, -446.0891481129646081, -319.0252816721025511 ) ) ;
#8703 = CARTESIAN_POINT ( 'NONE',  ( 1238.921997096861332, 240.0000000000000853, -360.0000000000000000 ) ) ;
#8704 = CARTESIAN_POINT ( 'NONE',  ( 799.4546378042377910, -81.07832356259649487, 356.1575198192848006 ) ) ;
#8705 = ORIENTED_EDGE ( 'NONE', *, *, #27181, .F. ) ;
#8706 = CARTESIAN_POINT ( 'NONE',  ( 756.1348686366196716, -209.2601417444142839, -347.5531968255698416 ) ) ;
#8707 = CARTESIAN_POINT ( 'NONE',  ( 804.6798772138708955, -63.72551174932939233, 334.6312213355107019 ) ) ;
#8708 = CARTESIAN_POINT ( 'NONE',  ( 768.8385539511368734, -215.2601417444141987, -306.4236121716840557 ) ) ;
#8709 = PLANE ( 'NONE',  #33452 ) ;
#8710 = CARTESIAN_POINT ( 'NONE',  ( 746.0683387631852383, -355.4419599262319593, 331.3260364891676204 ) ) ;
#8711 = ORIENTED_EDGE ( 'NONE', *, *, #28285, .F. ) ;
#8712 = CONICAL_SURFACE ( 'NONE', #18316, 8.025000000000003908, 0.7853981633974482790 ) ;
#8713 = CARTESIAN_POINT ( 'NONE',  ( 745.1769319972822814, -425.8055962898680491, 346.2694204179732083 ) ) ;
#8714 = CARTESIAN_POINT ( 'NONE',  ( 759.9864689768902508, -146.0891481129655176, -354.9819416627836404 ) ) ;
#8715 = CARTESIAN_POINT ( 'NONE',  ( 802.1676090361156639, -326.6346026584193396, 327.8955696845344505 ) ) ;
#8716 = CARTESIAN_POINT ( 'NONE',  ( 772.5602148656447525, -81.72551174932937101, -305.7998596910095443 ) ) ;
#8717 = CARTESIAN_POINT ( 'NONE',  ( 800.0135310231082713, -62.08914811296580183, -325.0180583372163028 ) ) ;
#8718 = ORIENTED_EDGE ( 'NONE', *, *, #30332, .F. ) ;
#8719 = CARTESIAN_POINT ( 'NONE',  ( 804.6971507214547046, -27.28179084515336328, -344.0799538623459739 ) ) ;
#8720 = ORIENTED_EDGE ( 'NONE', *, *, #7243, .F. ) ;
#8721 = CARTESIAN_POINT ( 'NONE',  ( 798.5707757039680246, -317.4636090269706301, -356.7845633553585003 ) ) ;
#8722 = CONTEXT_DEPENDENT_SHAPE_REPRESENTATION ( #6042, #45062 ) ;
#8724 = CARTESIAN_POINT ( 'NONE',  ( 759.0159684113467620, -376.9181544815159555, 325.8855110935213020 ) ) ;
#8723 = CARTESIAN_POINT ( 'NONE',  ( 762.3223304703356007, -79.54369356751119824, 322.3223304703362828 ) ) ;
#8727 = CARTESIAN_POINT ( 'NONE',  ( 800.1688906516307043, -322.1692326535048210, 369.0717654672308186 ) ) ;
#8726 = DIRECTION ( 'NONE',  ( 0.000000000000000000, -0.3826834323650835645, -0.9238795325112892920 ) ) ;
#8725 = CARTESIAN_POINT ( 'NONE',  ( 787.5162901302840055, -419.3618753856918602, 305.4481719005793252 ) ) ;
#8728 = CARTESIAN_POINT ( 'NONE',  ( 778.7502325331095108, -96.35105083532370429, 304.6391490659818828 ) ) ;
#8729 = CARTESIAN_POINT ( 'NONE',  ( 773.4516893846965786, -307.6454272087888171, -315.8398074228977066 ) ) ;
#8730 = CARTESIAN_POINT ( 'NONE',  ( 792.1044303154645831, -324.4527844766013231, -317.8323909638837677 ) ) ;
#8731 = CARTESIAN_POINT ( 'NONE',  ( 804.4286716492782716, -137.3618753856928265, -345.3141322388244703 ) ) ;
#8732 = CARTESIAN_POINT ( 'NONE',  ( 759.0252816721024374, -432.9982390220555999, 368.0189434323527280 ) ) ;
#8734 = LINE ( 'NONE', #16326, #27061 ) ;
#8733 = FACE_OUTER_BOUND ( 'NONE', #10414, .T. ) ;
#8735 = CARTESIAN_POINT ( 'NONE',  ( 757.7880784355613741, -114.0090635724258163, -312.4576283171834916 ) ) ;
#8736 = LINE ( 'NONE', #14764, #5687 ) ;
#8737 = CARTESIAN_POINT ( 'NONE',  ( 759.9999999999992042, -512.9681489794448908, 339.9999999999999432 ) ) ;
#8738 = CARTESIAN_POINT ( 'NONE',  ( 804.6971507214547046, -291.2817908451525000, 344.0799538623459739 ) ) ;
#8739 = CARTESIAN_POINT ( 'NONE',  ( 804.6798772138708955, -183.7255117493290015, 334.6312213355107019 ) ) ;
#8740 = VERTEX_POINT ( 'NONE', #16554 ) ;
#8741 = CARTESIAN_POINT ( 'NONE',  ( 787.4397851343537695, -141.7255117493291721, -374.2001403089903988 ) ) ;
#8742 = CYLINDRICAL_SURFACE ( 'NONE', #18710, 10.00000000000000888 ) ;
#8743 = CARTESIAN_POINT ( 'NONE',  ( 755.8990559732751535, -83.46360902697136908, 365.9055244015606831 ) ) ;
#8744 = CARTESIAN_POINT ( 'NONE',  ( 782.5225473063381969, -286.2709662947833635, -375.2698199232970637 ) ) ;
#8745 = CARTESIAN_POINT ( 'NONE',  ( 815.2698199232962679, -448.8164208402372424, -342.5225473063383674 ) ) ;
#8746 = CARTESIAN_POINT ( 'NONE',  ( 785.3141322388236176, -141.7255117493291721, 364.4286716492789537 ) ) ;
#8747 = VERTEX_POINT ( 'NONE', #40128 ) ;
#8748 = CARTESIAN_POINT ( 'NONE',  ( 744.9990715423526808, -330.3510508353229511, -341.2370466360926002 ) ) ;
#8749 = CARTESIAN_POINT ( 'NONE',  ( 782.4968714119720516, -82.81642084023846451, -305.0891759886411023 ) ) ;
#8750 = CARTESIAN_POINT ( 'NONE',  ( 796.1575198192839480, -6.009063572426154742, 359.4546378042384163 ) ) ;
#8751 = CARTESIAN_POINT ( 'NONE',  ( 777.5031285880264704, -334.8164208402376403, -374.9108240113588408 ) ) ;
#8752 = PLANE ( 'NONE',  #29858 ) ;
#8753 = CARTESIAN_POINT ( 'NONE',  ( 763.2154366446407039, -381.6237781080500326, 321.4292242960311228 ) ) ;
#8754 = VERTEX_POINT ( 'NONE', #8491 ) ;
#8755 = CARTESIAN_POINT ( 'NONE',  ( 811.6461892240364477, -124.7146871989599930, -324.1737431748509835 ) ) ;
#8756 = DIRECTION ( 'NONE',  ( 1.000000000000000000, -4.147566128926370535E-16, 0.000000000000000000 ) ) ;
#8757 = CARTESIAN_POINT ( 'NONE',  ( 813.2346286133761168, -245.2601417444141987, 328.9521613784389160 ) ) ;
#8758 = CARTESIAN_POINT ( 'NONE',  ( 802.1676090361155502, -38.63460265842041963, 327.8955696845344505 ) ) ;
#8759 = ORIENTED_EDGE ( 'NONE', *, *, #41330, .T. ) ;
#8760 = CARTESIAN_POINT ( 'NONE',  ( 759.2295555964440155, -232.1692326535051620, -353.9708237608231229 ) ) ;
#8761 = CARTESIAN_POINT ( 'NONE',  ( 768.0187753319979720, -224.6346026584198228, 318.0580252608186242 ) ) ;
#8762 = CARTESIAN_POINT ( 'NONE',  ( 810.1134526219336749, -440.5328690171407970, -357.8822607201570349 ) ) ;
#8763 = CARTESIAN_POINT ( 'NONE',  ( 759.8311093483677041, -70.16923265350563099, -310.9282345327691814 ) ) ;
#8764 = DIRECTION ( 'NONE',  ( 0.000000000000000000, 0.000000000000000000, -1.000000000000000000 ) ) ;
#8765 = ORIENTED_EDGE ( 'NONE', *, *, #20717, .F. ) ;
#8766 = CARTESIAN_POINT ( 'NONE',  ( 805.6418435158337843, -365.4636090269705164, -363.8556311672236916 ) ) ;
#8767 = VECTOR ( 'NONE', #11813, 1000.000000000000000 ) ;
#8768 = CARTESIAN_POINT ( 'NONE',  ( 800.0135310231082713, -230.0891481129652618, -325.0180583372163028 ) ) ;
#8769 = CARTESIAN_POINT ( 'NONE',  ( 759.0252816721024374, -336.9982390220558273, 368.0189434323527280 ) ) ;
#8770 = CARTESIAN_POINT ( 'NONE',  ( 746.0683387631852383, -43.44195992623296831, 331.3260364891676204 ) ) ;
#8771 = CARTESIAN_POINT ( 'NONE',  ( 776.9254006560222479, -236.1908817542436338, -314.8983024940802125 ) ) ;
#8772 = CARTESIAN_POINT ( 'NONE',  ( 755.0636971347428243, -220.2709662947834772, -341.7834795799807353 ) ) ;
#8773 = CARTESIAN_POINT ( 'NONE',  ( 785.3141322388236176, -381.7255117493284615, -364.4286716492789537 ) ) ;
#8774 = VERTEX_POINT ( 'NONE', #33871 ) ;
#8775 = CARTESIAN_POINT ( 'NONE',  ( 800.2193346964447755, -210.9982390220561967, 355.1360043628815788 ) ) ;
#8776 = CARTESIAN_POINT ( 'NONE',  ( 797.6776695296629214, -91.54369356751116982, -357.6776695296636603 ) ) ;
#8777 = ORIENTED_EDGE ( 'NONE', *, *, #33179, .F. ) ;
#8778 = CARTESIAN_POINT ( 'NONE',  ( 751.6929314249748586, -318.9982390220557704, 318.8095938919659034 ) ) ;
#8779 = CARTESIAN_POINT ( 'NONE',  ( 782.7696130847263021, 18.14353250567099707, -310.1281195208451322 ) ) ;
#8780 = LINE ( 'NONE', #3779, #4191 ) ;
#8781 = CARTESIAN_POINT ( 'NONE',  ( 701.1634899080286232, 239.9999999999999432, -202.7499999999988916 ) ) ;
#8782 = CARTESIAN_POINT ( 'NONE',  ( 775.8780910478218402, -177.2817908451528695, 364.9511171171680530 ) ) ;
#8783 = CARTESIAN_POINT ( 'NONE',  ( 754.8072714833581358, -100.8164208402383792, 338.1981804954720587 ) ) ;
#8784 = ORIENTED_EDGE ( 'NONE', *, *, #26936, .T. ) ;
#8785 = CARTESIAN_POINT ( 'NONE',  ( 773.7305795820266212, -441.2817908451521021, -374.8230680027170365 ) ) ;
#8786 = CARTESIAN_POINT ( 'NONE',  ( 745.0891759886404770, -52.27096629478401724, -342.4968714119734159 ) ) ;
#8787 = CARTESIAN_POINT ( 'NONE',  ( 780.5290396650775619, -252.3510508353232353, 365.2837595273619513 ) ) ;
#8788 = CARTESIAN_POINT ( 'NONE',  ( 778.2165204200184689, -382.8164208402374697, -364.9363028652563230 ) ) ;
#8789 = CARTESIAN_POINT ( 'NONE',  ( 797.6776695296629214, 4.456306432488530866, -357.6776695296636603 ) ) ;
#8790 = CARTESIAN_POINT ( 'NONE',  ( 745.0891759886404770, -436.2709662947827951, 342.4968714119734159 ) ) ;
#8791 = DIRECTION ( 'NONE',  ( -0.000000000000000000, 1.000000000000000000, -0.000000000000000000 ) ) ;
#8792 = CARTESIAN_POINT ( 'NONE',  ( 804.6971507214547046, -267.2817908451526137, -344.0799538623459739 ) ) ;
#8793 = CARTESIAN_POINT ( 'NONE',  ( 805.0032342141412300, -181.5436935675108145, -314.9967657858571783 ) ) ;
#8794 = CARTESIAN_POINT ( 'NONE',  ( 808.0189434323515343, -62.08914811296580183, 319.0252816721025511 ) ) ;
#8795 = CARTESIAN_POINT ( 'NONE',  ( 814.9108240113580450, -136.2709662947837330, 337.5031285880265273 ) ) ;
#8796 = CARTESIAN_POINT ( 'NONE',  ( 778.5401871010416244, 16.45630643248848912, -314.2029270906900251 ) ) ;
#8797 =( NAMED_UNIT ( * ) SI_UNIT ( $, .STERADIAN. ) SOLID_ANGLE_UNIT ( ) );
#8798 = VECTOR ( 'NONE', #43446, 1000.000000000000000 ) ;
#8799 = CARTESIAN_POINT ( 'NONE',  ( 999.9999999999992042, -599.0000000000001137, -359.0000000000000000 ) ) ;
#8800 = CARTESIAN_POINT ( 'NONE',  ( 787.5162901302840055, -347.3618753856922012, 305.4481719005792684 ) ) ;
#8801 = ADVANCED_FACE ( 'NONE', ( #26262 ), #36666, .F. ) ;
#8802 = CARTESIAN_POINT ( 'NONE',  ( 755.3201227861273992, -315.7255117493286320, -345.3687786644892981 ) ) ;
#8803 = CARTESIAN_POINT ( 'NONE',  ( 756.1348686366196716, 6.739858255585061464, 347.5531968255698416 ) ) ;
#8804 = CARTESIAN_POINT ( 'NONE',  ( 805.6418435158337843, -101.4636090269713264, -363.8556311672236916 ) ) ;
#8805 = CARTESIAN_POINT ( 'NONE',  ( 776.9566956441375396, -132.8965053807781374, -364.8461984189686405 ) ) ;
#8806 = CARTESIAN_POINT ( 'NONE',  ( 768.8385539511368734, -143.2601417444144829, 306.4236121716840557 ) ) ;
#8807 = DIRECTION ( 'NONE',  ( 0.000000000000000000, 0.000000000000000000, 1.000000000000000000 ) ) ;
#8808 = CARTESIAN_POINT ( 'NONE',  ( 788.7366044899766848, -11.90732993114778182, -316.5762568750059813 ) ) ;
#8809 = CARTESIAN_POINT ( 'NONE',  ( 763.2154366446407039, -141.6237781080508569, -321.4292242960311228 ) ) ;
#8810 = CARTESIAN_POINT ( 'NONE',  ( 804.9363028652555840, -136.2709662947837330, -338.2165204200192079 ) ) ;
#8811 = CARTESIAN_POINT ( 'NONE',  ( 791.9812246680005501, -140.6346026584201070, 361.9419747391813189 ) ) ;
#8812 = CARTESIAN_POINT ( 'NONE',  ( 757.2208543904082489, -424.7146871989589840, -350.9844846989624330 ) ) ;
#8814 = CARTESIAN_POINT ( 'NONE',  ( 778.1981804954715471, -250.2709662947833351, 314.8072714833591021 ) ) ;
#8813 = CARTESIAN_POINT ( 'NONE',  ( 788.7366044899766848, -275.9073299311469896, 316.5762568750059813 ) ) ;
#8815 = CARTESIAN_POINT ( 'NONE',  ( -809.9999999999993179, -512.9681489794448908, -329.9999999999999432 ) ) ;
#8816 = ORIENTED_EDGE ( 'NONE', *, *, #3017, .T. ) ;
#8817 = CARTESIAN_POINT ( 'NONE',  ( 756.7813123517142913, 4.012585528312341054, 329.9779781133712504 ) ) ;
#8818 = CARTESIAN_POINT ( 'NONE',  ( 814.2805881961230625, -289.6454272087889308, -331.2368401574024119 ) ) ;
#8819 = EDGE_LOOP ( 'NONE', ( #15795, #438, #15741, #30393 ) ) ;
#8820 = CARTESIAN_POINT ( 'NONE',  ( 0.000000000000000000, 0.000000000000000000, 0.000000000000000000 ) ) ;
#8821 = CARTESIAN_POINT ( 'NONE',  ( 812.7932403749906598, -207.1800572038744406, 327.7687537140311633 ) ) ;
#8822 = CARTESIAN_POINT ( 'NONE',  ( 780.5236548040995785, -308.7363362996979390, 314.9735926884559944 ) ) ;
#8823 = CARTESIAN_POINT ( 'NONE',  ( 780.5290396650775619, -396.3510508353228374, 365.2837595273619513 ) ) ;
#8824 = ORIENTED_EDGE ( 'NONE', *, *, #6060, .T. ) ;
#8825 = CARTESIAN_POINT ( 'NONE',  ( 800.9840315886518738, -100.9181544815167513, -354.1144889064786412 ) ) ;
#8826 = CARTESIAN_POINT ( 'NONE',  ( 791.9812246680005501, -284.6346026584196807, -361.9419747391813189 ) ) ;
#8827 = VERTEX_POINT ( 'NONE', #15637 ) ;
#8828 = CONICAL_SURFACE ( 'NONE', #13252, 8.025000000000003908, 0.7853981633974410625 ) ;
#8829 = CARTESIAN_POINT ( 'NONE',  ( 762.3223304703356007, -415.5436935675102177, -322.3223304703362828 ) ) ;
#8830 = CARTESIAN_POINT ( 'NONE',  ( 754.8072714833581358, -100.8164208402383792, -338.1981804954720587 ) ) ;
#8831 = CARTESIAN_POINT ( 'NONE',  ( 759.2295555964440155, -280.1692326535049347, 353.9708237608231229 ) ) ;
#8832 = DIRECTION ( 'NONE',  ( 1.892425610156518354E-16, 1.000000000000000000, -0.000000000000000000 ) ) ;
#8833 = PLANE ( 'NONE',  #4939 ) ;
#8834 = CARTESIAN_POINT ( 'NONE',  ( 792.1044303154645831, 11.54721552339760038, 317.8323909638837677 ) ) ;
#8835 = VERTEX_POINT ( 'NONE', #44268 ) ;
#8836 = CARTESIAN_POINT ( 'NONE',  ( 766.4474001241216001, -355.0999726633341993, -307.3154664389482491 ) ) ;
#8837 = CARTESIAN_POINT ( 'NONE',  ( 791.0478386215596629, -213.8272453906073167, 306.7653713866226326 ) ) ;
#8839 = CARTESIAN_POINT ( 'NONE',  ( 797.6776695296629214, -283.5436935675105019, -357.6776695296636603 ) ) ;
#8838 = CARTESIAN_POINT ( 'NONE',  ( 998.9999999999992042, -600.0000000000001137, -360.0000000000000000 ) ) ;
#8840 = DIRECTION ( 'NONE',  ( 1.000000000000000000, 0.000000000000000000, 0.000000000000000000 ) ) ;
#8841 = CARTESIAN_POINT ( 'NONE',  ( 796.1575198192839480, -150.0090635724257027, -359.4546378042384163 ) ) ;
#8842 = EDGE_CURVE ( 'NONE', #8317, #16303, #16093, .T. ) ;
#8843 = CARTESIAN_POINT ( 'NONE',  ( 748.9653473494363425, -50.63460265842036989, 356.9462024416521331 ) ) ;
#8844 = DIRECTION ( 'NONE',  ( 1.000000000000000000, -0.000000000000000000, -0.000000000000000000 ) ) ;
#8845 = CARTESIAN_POINT ( 'NONE',  ( 801.1904061080338124, -332.0891481129649492, -368.3070685750236066 ) ) ;
#8846 = DIRECTION ( 'NONE',  ( -0.000000000000000000, 1.000000000000000000, -0.000000000000000000 ) ) ;
#8847 = CARTESIAN_POINT ( 'NONE',  ( 800.0135310231082713, -38.08914811296587999, 325.0180583372163028 ) ) ;
#8848 = CARTESIAN_POINT ( 'NONE',  ( 747.6481478633932056, -277.0999726633344267, 353.4146539503763620 ) ) ;
#8849 = CARTESIAN_POINT ( 'NONE',  ( 751.9810565676468741, -266.0891481129651197, 360.9747183278973921 ) ) ;
#8850 = CARTESIAN_POINT ( 'NONE',  ( 777.5031285880264704, 1.183579159761269040, -374.9108240113588408 ) ) ;
#8851 = ADVANCED_FACE ( 'NONE', ( #29720 ), #43798, .F. ) ;
#8852 = CARTESIAN_POINT ( 'NONE',  ( 959.5497976682736407, 229.9999999999998579, -2132.806278688367456 ) ) ;
#8853 = DIRECTION ( 'NONE',  ( -0.000000000000000000, 1.000000000000000000, -0.000000000000000000 ) ) ;
#8854 = CARTESIAN_POINT ( 'NONE',  ( 797.8594530101008786, -349.5436935675102745, 322.1405469898980982 ) ) ;
#8855 = CARTESIAN_POINT ( 'NONE',  ( 804.1105419155481968, -123.8272453906076009, 347.6308680596136469 ) ) ;
#8856 = CARTESIAN_POINT ( 'NONE',  ( 760.5453621957607311, -21.07832356259667250, -323.8424801807151425 ) ) ;
#8857 = FACE_OUTER_BOUND ( 'NONE', #25285, .T. ) ;
#8858 = CARTESIAN_POINT ( 'NONE',  ( 919.9999999999993179, 219.9999999999998863, -360.0000000000000000 ) ) ;
#8859 = CARTESIAN_POINT ( 'NONE',  ( 795.1360043628807261, -404.0891481129646081, 360.2193346964456282 ) ) ;
#8860 = ORIENTED_EDGE ( 'NONE', *, *, #2576, .F. ) ;
#8861 = CARTESIAN_POINT ( 'NONE',  ( 779.4709603349208464, -312.3510508353230080, -314.7162404726379918 ) ) ;
#8863 = CARTESIAN_POINT ( 'NONE',  ( 755.3201227861273992, -171.7255117493290868, 345.3687786644892981 ) ) ;
#8862 = CARTESIAN_POINT ( 'NONE',  ( 767.8955696845333705, -168.4527844766018347, 362.1676090361162323 ) ) ;
#8864 = PRODUCT_DEFINITION_CONTEXT ( 'detailed design', #17542, 'design' ) ;
#8865 = CARTESIAN_POINT ( 'NONE',  ( 783.7566961878529810, -336.8965053807774552, -305.1792804349288417 ) ) ;
#8866 = DIRECTION ( 'NONE',  ( -1.000000000000000000, -0.000000000000000000, -0.000000000000000000 ) ) ;
#8867 = ADVANCED_FACE ( 'NONE', ( #22791 ), #5454, .F. ) ;
#8868 = ORIENTED_EDGE ( 'NONE', *, *, #12822, .F. ) ;
#8869 = CARTESIAN_POINT ( 'NONE',  ( 755.0636971347428243, -364.2709662947830793, 341.7834795799807353 ) ) ;
#8870 = EDGE_CURVE ( 'NONE', #1685, #6874, #37338, .T. ) ;
#8871 = ORIENTED_EDGE ( 'NONE', *, *, #15402, .F. ) ;
#8872 = CARTESIAN_POINT ( 'NONE',  ( 751.9810565676468741, -170.0891481129654608, -360.9747183278973921 ) ) ;
#8873 = CARTESIAN_POINT ( 'NONE',  ( 767.7687537140311633, -119.9073299311474443, 372.7932403749916830 ) ) ;
#8874 = EDGE_LOOP ( 'NONE', ( #8288, #10398, #44837, #35620 ) ) ;
#8875 = CARTESIAN_POINT ( 'NONE',  ( 774.6312213355098493, -191.3618753856926276, -364.6798772138717482 ) ) ;
#8876 = ORIENTED_EDGE ( 'NONE', *, *, #34864, .T. ) ;
#8877 = CARTESIAN_POINT ( 'NONE',  ( 754.7162404726377645, -446.7363362996975980, -339.4709603349214717 ) ) ;
#8878 = CARTESIAN_POINT ( 'NONE',  ( 814.9108240113580450, -256.2709662947834204, 337.5031285880265273 ) ) ;
#8879 = CARTESIAN_POINT ( 'NONE',  ( 805.0264073115434940, -174.3510508353234627, 339.4763451958999099 ) ) ;
#8881 = DIRECTION ( 'NONE',  ( 1.000000000000000000, 0.000000000000000000, 0.000000000000000000 ) ) ;
#8880 = DIRECTION ( 'NONE',  ( 0.000000000000000000, 0.000000000000000000, 1.000000000000000000 ) ) ;
#8882 = EDGE_LOOP ( 'NONE', ( #2728, #11684, #41023, #35664 ) ) ;
#8883 = CARTESIAN_POINT ( 'NONE',  ( 757.0176451133909268, -421.0999726633340288, -349.9200121543848354 ) ) ;
#8884 = CARTESIAN_POINT ( 'NONE',  ( 1820.038553321469863, -589.9999999999998863, 201.9999999999998579 ) ) ;
#8885 = CARTESIAN_POINT ( 'NONE',  ( 747.6481478633932056, -205.0999726633346256, -353.4146539503763620 ) ) ;
#8886 = CARTESIAN_POINT ( 'NONE',  ( 746.4236121716829757, -111.8272453906076151, 328.8385539511384650 ) ) ;
#8888 = CARTESIAN_POINT ( 'NONE',  ( 803.4237431249931660, -183.1800572038744974, -331.2633955100225194 ) ) ;
#8887 = DIRECTION ( 'NONE',  ( 0.000000000000000000, 1.000000000000000000, -0.000000000000000000 ) ) ;
#8889 = EDGE_CURVE ( 'NONE', #38409, #20274, #36550, .T. ) ;
#8890 = CARTESIAN_POINT ( 'NONE',  ( 775.9200461376533440, -359.8055962898683333, -315.3028492785443291 ) ) ;
#8891 = CARTESIAN_POINT ( 'NONE',  ( -78.83651009197140525, 260.0000000000000568, -199.9999999999936051 ) ) ;
#8892 = CARTESIAN_POINT ( 'NONE',  ( 802.2119215644370342, -222.0090635724254184, -367.5423716828165084 ) ) ;
#8893 = DIRECTION ( 'NONE',  ( 0.000000000000000000, 0.000000000000000000, -1.000000000000000000 ) ) ;
#8894 = LINE ( 'NONE', #6101, #17187 ) ;
#8895 = CARTESIAN_POINT ( 'NONE',  ( 804.6971507214547046, -51.28179084515328867, -344.0799538623459739 ) ) ;
#8896 = CARTESIAN_POINT ( 'NONE',  ( 766.0291762391763086, -394.9181544815158418, 360.7704444035551319 ) ) ;
#8897 = ADVANCED_FACE ( 'NONE', ( #44963 ), #41490, .F. ) ;
#8898 = CARTESIAN_POINT ( 'NONE',  ( 810.7187646348534145, -234.4527844766016358, -356.7737145352016341 ) ) ;
#8899 = DIRECTION ( 'NONE',  ( 0.000000000000000000, 0.000000000000000000, 1.000000000000000000 ) ) ;
#8900 = FACE_OUTER_BOUND ( 'NONE', #2396, .T. ) ;
#8901 = CARTESIAN_POINT ( 'NONE',  ( 755.0636971347428243, -52.27096629478401724, -341.7834795799807353 ) ) ;
#8902 = CARTESIAN_POINT ( 'NONE',  ( 809.0717654672305343, -196.9181544815164386, 360.1688906516309885 ) ) ;
#8903 = CARTESIAN_POINT ( 'NONE',  ( 764.3348316497523456, -118.7146871989600072, -308.6759233522265617 ) ) ;
#8904 = CARTESIAN_POINT ( 'NONE',  ( 814.2001403089898304, -137.3618753856928265, 347.4397851343538264 ) ) ;
#8905 = CARTESIAN_POINT ( 'NONE',  ( 792.3570229623688874, -357.1800572038739006, -373.1304606946836202 ) ) ;
#8906 = EDGE_CURVE ( 'NONE', #34191, #16721, #13320, .T. ) ;
#8907 = LINE ( 'NONE', #26899, #1056 ) ;
#8908 = CARTESIAN_POINT ( 'NONE',  ( 767.8955696845333705, -240.4527844766015221, 362.1676090361162323 ) ) ;
#8909 = CARTESIAN_POINT ( 'NONE',  ( 763.0428371773158460, -35.46360902697151829, 358.7617431975195359 ) ) ;
#8910 = CARTESIAN_POINT ( 'NONE',  ( 792.1044303154645831, -396.4527844766010389, -317.8323909638837677 ) ) ;
#8911 = LINE ( 'NONE', #44242, #366 ) ;
#8912 = CARTESIAN_POINT ( 'NONE',  ( 809.0717654672305343, -4.918154481517067467, -360.1688906516309885 ) ) ;
#8913 = DIRECTION ( 'NONE',  ( 0.000000000000000000, 1.000000000000000000, 0.000000000000000000 ) ) ;
#8914 = CARTESIAN_POINT ( 'NONE',  ( 754.8983024940795303, -90.89650538077827946, 336.9254006560228163 ) ) ;
#8915 = VERTEX_POINT ( 'NONE', #23913 ) ;
#8916 = CARTESIAN_POINT ( 'NONE',  ( 779.4709603349208464, -240.3510508353232069, -314.7162404726379918 ) ) ;
#8917 = CARTESIAN_POINT ( 'NONE',  ( 756.5762568750052424, -75.18005720387485269, 348.7366044899774238 ) ) ;
#8918 = CARTESIAN_POINT ( 'NONE',  ( 744.8212110874229666, -234.8965053807777963, -336.2046728542121627 ) ) ;
#8919 = CARTESIAN_POINT ( 'NONE',  ( 754.0944755984390895, -351.6237781080502032, 364.1009440267246760 ) ) ;
#8920 = EDGE_LOOP ( 'NONE', ( #921, #1748, #23517, #35732 ) ) ;
#8921 = CARTESIAN_POINT ( 'NONE',  ( 814.8230680027162407, -437.8055962898679923, 333.7305795820267917 ) ) ;
#8922 = ADVANCED_FACE ( 'NONE', ( #13784 ), #16789, .F. ) ;
#8923 = CARTESIAN_POINT ( 'NONE',  ( 764.8639956371174549, -368.0891481129647786, 319.7806653035542013 ) ) ;
#8924 = CARTESIAN_POINT ( 'NONE',  ( 772.4837098697144029, -71.36187538569302546, -374.5518280994205611 ) ) ;
#8925 = CARTESIAN_POINT ( 'NONE',  ( 803.4237431249931660, -87.18005720387481006, -331.2633955100225194 ) ) ;
#8926 = EDGE_LOOP ( 'NONE', ( #5902, #20512, #35977, #20567, #33801, #30215 ) ) ;
#8927 = CARTESIAN_POINT ( 'NONE',  ( 755.3028492785439312, -15.28179084515340058, -335.9200461376539693 ) ) ;
#8928 = ORIENTED_EDGE ( 'NONE', *, *, #17368, .T. ) ;
#8929 = CARTESIAN_POINT ( 'NONE',  ( 773.4516893846965786, -307.6454272087888171, -315.8398074228977066 ) ) ;
#8931 = CARTESIAN_POINT ( 'NONE',  ( 758.4439275373578084, -420.5545181178793541, 353.2243759319684386 ) ) ;
#8930 = CARTESIAN_POINT ( 'NONE',  ( 756.5762568750052424, -99.18005720387478164, 348.7366044899774238 ) ) ;
#8934 = CARTESIAN_POINT ( 'NONE',  ( 756.1443688327750579, -333.6237781080502600, 314.3581564841659315 ) ) ;
#8933 = DIRECTION ( 'NONE',  ( 1.000000000000000000, -0.000000000000000000, -0.000000000000000000 ) ) ;
#8932 = CARTESIAN_POINT ( 'NONE',  ( 749.2812353651451076, -414.4527844766010389, 323.2262854647983090 ) ) ;
#8935 = CARTESIAN_POINT ( 'NONE',  ( 754.0944755984390895, -111.6237781080509279, 364.1009440267246760 ) ) ;
#8936 = CARTESIAN_POINT ( 'NONE',  ( 802.9823548866075953, -313.0999726633342561, -330.0799878456151077 ) ) ;
#8937 = CARTESIAN_POINT ( 'NONE',  ( 800.2193346964447755, -306.9982390220558273, -355.1360043628815788 ) ) ;
#8938 = CARTESIAN_POINT ( 'NONE',  ( 800.2193346964447755, -162.9982390220563673, -355.1360043628815788 ) ) ;
#8939 = ADVANCED_BREP_SHAPE_REPRESENTATION ( '', ( #16696, #26858 ), #23892 ) ;
#8940 = CARTESIAN_POINT ( 'NONE',  ( 758.8095938919642549, -440.0891481129644944, 311.6929314249763365 ) ) ;
#8942 = DIRECTION ( 'NONE',  ( -1.000000000000000000, 0.000000000000000000, 0.000000000000000000 ) ) ;
#8941 = LINE ( 'NONE', #23470, #18218 ) ;
#8943 = ADVANCED_FACE ( 'NONE', ( #3617 ), #27863, .F. ) ;
#8944 = CARTESIAN_POINT ( 'NONE',  ( 800.7704444035546203, -268.1692326535049347, -326.0291762391768771 ) ) ;
#8945 = CARTESIAN_POINT ( 'NONE',  ( 749.5768839229115201, -108.5545181178803915, -358.0661480581553064 ) ) ;
#8946 = DIRECTION ( 'NONE',  ( 0.000000000000000000, 0.000000000000000000, -1.000000000000000000 ) ) ;
#8947 = CARTESIAN_POINT ( 'NONE',  ( 879.9999999999992042, 469.9999999999998863, 210.0000000000000000 ) ) ;
#8948 = CARTESIAN_POINT ( 'NONE',  ( 783.0745993439762742, -296.1908817542434917, 365.1016975059196739 ) ) ;
#8949 = EDGE_CURVE ( 'NONE', #44204, #45600, #28075, .T. ) ;
#8950 = CARTESIAN_POINT ( 'NONE',  ( 800.0135310231082713, -182.0891481129654323, 325.0180583372163028 ) ) ;
#8951 = ORIENTED_EDGE ( 'NONE', *, *, #22178, .F. ) ;
#8952 = CARTESIAN_POINT ( 'NONE',  ( 814.4686193811664907, -267.2817908451526137, 346.2056067578752732 ) ) ;
#8953 = CARTESIAN_POINT ( 'NONE',  ( 755.2512626584698410, -151.5436935675109851, -315.2512626584710915 ) ) ;
#8954 = CARTESIAN_POINT ( 'NONE',  ( -39.63011601220123481, -494.6608068873671300, -357.6536686473015720 ) ) ;
#8955 = CARTESIAN_POINT ( 'NONE',  ( 776.2046728542105711, -92.19088175424406018, 304.8212110874238761 ) ) ;
#8956 = CARTESIAN_POINT ( 'NONE',  ( 763.0537975583475827, -264.4527844766016074, -371.0346526505627480 ) ) ;
#8957 = DIRECTION ( 'NONE',  ( 1.000000000000000000, -0.000000000000000000, -0.000000000000000000 ) ) ;
#8958 = CARTESIAN_POINT ( 'NONE',  ( 797.6776695296629214, -163.5436935675109567, 357.6776695296636603 ) ) ;
#8959 = VERTEX_POINT ( 'NONE', #2693 ) ;
#8960 = CARTESIAN_POINT ( 'NONE',  ( 771.2368401574024119, -349.4419599262320162, -374.2805881961240857 ) ) ;
#8961 = CARTESIAN_POINT ( 'NONE',  ( 810.7187646348534145, -90.45278447660209054, -356.7737145352016341 ) ) ;
#8962 = CARTESIAN_POINT ( 'NONE',  ( 790.0220218866281812, -31.09997266333516919, 363.2186876482849129 ) ) ;
#8963 = CARTESIAN_POINT ( 'NONE',  ( 792.3570229623688874, -357.1800572038739006, -373.1304606946836202 ) ) ;
#8964 = CARTESIAN_POINT ( 'NONE',  ( 989.9999999999992042, -184.9457194955396631, 62.92409052808250891 ) ) ;
#8965 = CARTESIAN_POINT ( 'NONE',  ( 789.9200121543843807, -433.9874144716862361, 317.0176451133914384 ) ) ;
#8966 = ORIENTED_EDGE ( 'NONE', *, *, #29262, .F. ) ;
#8967 = CARTESIAN_POINT ( 'NONE',  ( 754.8072714833581358, -220.8164208402379529, -338.1981804954720587 ) ) ;
#8968 = CARTESIAN_POINT ( 'NONE',  ( 751.2241431872005251, -136.1692326535053894, -359.9636004259367610 ) ) ;
#8969 = CARTESIAN_POINT ( 'NONE',  ( 786.4999999999993179, -513.1383975375929367, -369.9999999999999432 ) ) ;
#8970 = CARTESIAN_POINT ( 'NONE',  ( 791.1614460488616487, -227.2601417444141987, 373.5763878283158874 ) ) ;
#8971 = CARTESIAN_POINT ( 'NONE',  ( 805.1927285166399315, -88.81642084023843609, 341.8018195045277707 ) ) ;
#8972 = ORIENTED_EDGE ( 'NONE', *, *, #19296, .F. ) ;
#8973 = CARTESIAN_POINT ( 'NONE',  ( 754.9735926884551418, 5.648949164675971524, -340.5236548041000333 ) ) ;
#8974 = CARTESIAN_POINT ( 'NONE',  ( 754.8072714833581358, -268.8164208402378108, 338.1981804954720587 ) ) ;
#8975 = CARTESIAN_POINT ( 'NONE',  ( 795.6651683502461765, -418.7146871989590409, -371.3240766477733814 ) ) ;
#8976 = DIRECTION ( 'NONE',  ( -1.000000000000000000, -0.000000000000000000, 0.000000000000000000 ) ) ;
#8977 = ORIENTED_EDGE ( 'NONE', *, *, #34012, .F. ) ;
#8978 = EDGE_LOOP ( 'NONE', ( #30270, #26130, #5585, #32312 ) ) ;
#8979 = CARTESIAN_POINT ( 'NONE',  ( 768.9521613784389729, -393.8272453906067199, -373.2346286133773106 ) ) ;
#8980 = CARTESIAN_POINT ( 'NONE',  ( 762.1405469898971887, -241.5436935675106156, -357.8594530101015607 ) ) ;
#8981 = CARTESIAN_POINT ( 'NONE',  ( 800.9747183278959710, -324.9982390220559409, 311.9810565676471583 ) ) ;
#8982 = CARTESIAN_POINT ( 'NONE',  ( 764.3348316497523456, -22.71468719896029853, 308.6759233522265617 ) ) ;
#8983 = CARTESIAN_POINT ( 'NONE',  ( 804.4086373105744769, -217.6454272087891582, -333.3843516231986541 ) ) ;
#8984 = CARTESIAN_POINT ( 'NONE',  ( 797.8594530101008786, -205.5436935675108430, -322.1405469898980982 ) ) ;
#8985 = AXIS2_PLACEMENT_3D ( 'NONE', #30769, #6274, #23587 ) ;
#8986 = CARTESIAN_POINT ( 'NONE',  ( 803.4237431249931660, -399.1800572038738437, -331.2633955100225194 ) ) ;
#8987 = EDGE_LOOP ( 'NONE', ( #2012, #36325, #4837, #24253, #26408, #12665, #37665, #4056 ) ) ;
#8988 = CARTESIAN_POINT ( 'NONE',  ( 792.1044303154645831, -204.4527844766016926, 317.8323909638837677 ) ) ;
#8989 = CARTESIAN_POINT ( 'NONE',  ( 778.2165204200184689, -94.81642084023843609, -364.9363028652563230 ) ) ;
#8990 = ORIENTED_EDGE ( 'NONE', *, *, #45289, .T. ) ;
#8991 = CARTESIAN_POINT ( 'NONE',  ( 745.4481719005789273, -315.7255117493286320, 347.5162901302853129 ) ) ;
#8992 = DIRECTION ( 'NONE',  ( -0.000000000000000000, 1.000000000000000000, -0.000000000000000000 ) ) ;
#8993 = DIRECTION ( 'NONE',  ( -0.000000000000000000, 1.000000000000000000, -0.000000000000000000 ) ) ;
#8994 = CYLINDRICAL_SURFACE ( 'NONE', #14301, 9.999999999999980460 ) ;
#8995 = CARTESIAN_POINT ( 'NONE',  ( 804.6971507214547046, -195.2817908451528410, 344.0799538623459739 ) ) ;
#8996 = CARTESIAN_POINT ( 'NONE',  ( 794.9819416627830151, -84.99823902205663728, 319.9864689768909898 ) ) ;
#8997 = ORIENTED_EDGE ( 'NONE', *, *, #17059, .T. ) ;
#8998 = CARTESIAN_POINT ( 'NONE',  ( 748.6759233522253680, -448.3726999360611103, -324.3348316497537098 ) ) ;
#8999 = CARTESIAN_POINT ( 'NONE',  ( 808.3070685750232087, -42.99823902205676518, -361.1904061080339829 ) ) ;
#9000 = CARTESIAN_POINT ( 'NONE',  ( 773.3843516231979720, -253.4419599262323572, 364.4086373105754433 ) ) ;
#9001 = CARTESIAN_POINT ( 'NONE',  ( 794.9819416627830151, -396.9982390220556567, -319.9864689768909898 ) ) ;
#9002 = CARTESIAN_POINT ( 'NONE',  ( 762.1405469898973024, -25.54369356751137232, -357.8594530101016176 ) ) ;
#9003 = CARTESIAN_POINT ( 'NONE',  ( 805.0032342141412300, -421.5436935675101040, 314.9967657858571783 ) ) ;
#9004 = CARTESIAN_POINT ( 'NONE',  ( -208.8365100919714052, 230.0000000000000853, -199.9999999999926956 ) ) ;
#9005 = CARTESIAN_POINT ( 'NONE',  ( 799.2566176426618085, -288.0090635724252479, -324.0069404352559559 ) ) ;
#9006 = CARTESIAN_POINT ( 'NONE',  ( 745.4481719005789273, -171.7255117493291152, -347.5162901302853129 ) ) ;
#9007 = CARTESIAN_POINT ( 'NONE',  ( 812.7932403749906598, -87.18005720387481006, 327.7687537140311633 ) ) ;
#9008 = CARTESIAN_POINT ( 'NONE',  ( 811.0346526505616112, -134.6346026584201070, 323.0537975583477532 ) ) ;
#9009 = CARTESIAN_POINT ( 'NONE',  ( 780.7518514355283514, 16.45630643248848912, -313.9393219192966740 ) ) ;
#9010 = CARTESIAN_POINT ( 'NONE',  ( 701.1634899080286232, 256.4999999999999432, -199.9999999999990337 ) ) ;
#9011 = DIRECTION ( 'NONE',  ( 0.000000000000000000, 0.7071067811865474617, 0.7071067811865474617 ) ) ;
#9012 = CARTESIAN_POINT ( 'NONE',  ( 800.9747183278959710, -348.9982390220558273, 311.9810565676471583 ) ) ;
#9013 = CARTESIAN_POINT ( 'NONE',  ( 797.8594530101008786, -349.5436935675102745, -322.1405469898980982 ) ) ;
#9014 = CARTESIAN_POINT ( 'NONE',  ( 803.8651313633788504, 18.73985825558501972, 332.4468031744301015 ) ) ;
#9015 = CIRCLE ( 'NONE', #9744, 2.749999999999835687 ) ;
#9016 = CARTESIAN_POINT ( 'NONE',  ( 783.7953271457878373, -104.1908817542440175, -375.1787889125761239 ) ) ;
#9017 = CARTESIAN_POINT ( 'NONE',  ( 755.0488828828309806, -161.8055962898689870, -344.1219089521771934 ) ) ;
#9018 = CARTESIAN_POINT ( 'NONE',  ( 756.1443688327750579, -141.6237781080508569, 314.3581564841659315 ) ) ;
#9019 = CARTESIAN_POINT ( 'NONE',  ( 801.9419747391806368, 5.547215523397618142, 351.9812246680014027 ) ) ;
#9020 = CARTESIAN_POINT ( 'NONE',  ( 805.1927285166397041, -40.81642084023859951, -341.8018195045277707 ) ) ;
#9021 = CARTESIAN_POINT ( 'NONE',  ( 765.8855110935204493, -166.1692326535053041, -319.0159684113471599 ) ) ;
#9022 = CARTESIAN_POINT ( 'NONE',  ( 800.2193346964447755, -138.9982390220563957, -355.1360043628815788 ) ) ;
#9023 = CARTESIAN_POINT ( 'NONE',  ( 774.6312213355099630, -119.3618753856928691, 364.6798772138717482 ) ) ;
#9024 = CARTESIAN_POINT ( 'NONE',  ( 779.4709603349208464, -432.3510508353226669, -314.7162404726379918 ) ) ;
#9026 = CARTESIAN_POINT ( 'NONE',  ( 785.3687786644885591, -275.3618753856924286, 315.3201227861280813 ) ) ;
#9025 = CARTESIAN_POINT ( 'NONE',  ( 788.8264449731200330, -285.1800572038740711, 363.6646147819171233 ) ) ;
#9027 = FACE_OUTER_BOUND ( 'NONE', #5128, .T. ) ;
#9028 = ORIENTED_EDGE ( 'NONE', *, *, #19257, .T. ) ;
#9029 = CARTESIAN_POINT ( 'NONE',  ( 804.1601925771018387, 16.55804007376685050, 346.5483106153029098 ) ) ;
#9030 = CARTESIAN_POINT ( 'NONE',  ( 755.8990559732751535, -275.4636090269708575, -365.9055244015606831 ) ) ;
#9031 = VERTEX_POINT ( 'NONE', #38034 ) ;
#9032 = CARTESIAN_POINT ( 'NONE',  ( 0.000000000000000000, 0.000000000000000000, 0.000000000000000000 ) ) ;
#9033 = CARTESIAN_POINT ( 'NONE',  ( 815.2698199232962679, -208.8164208402380666, 342.5225473063383674 ) ) ;
#9034 = CARTESIAN_POINT ( 'NONE',  ( 804.6971507214547046, -315.2817908451525000, 344.0799538623459739 ) ) ;
#9035 = CARTESIAN_POINT ( 'NONE',  ( 773.3843516231979720, -397.4419599262317320, 364.4086373105754433 ) ) ;
#9036 = ORIENTED_EDGE ( 'NONE', *, *, #16099, .F. ) ;
#9037 = CARTESIAN_POINT ( 'NONE',  ( 784.1219089521767955, -117.2817908451530684, -315.0488828828318333 ) ) ;
#9038 = CARTESIAN_POINT ( 'NONE',  ( 762.3223304703356007, -127.5436935675110561, -322.3223304703362828 ) ) ;
#9039 = CIRCLE ( 'NONE', #34852, 19.99999999999998934 ) ;
#9040 = CARTESIAN_POINT ( 'NONE',  ( 755.0636971347428243, -268.2709662947833067, -341.7834795799807353 ) ) ;
#9041 = ORIENTED_EDGE ( 'NONE', *, *, #42791, .F. ) ;
#9042 = CARTESIAN_POINT ( 'NONE',  ( 778.2165204200184689, -430.8164208402374129, -364.9363028652563230 ) ) ;
#9043 = CARTESIAN_POINT ( 'NONE',  ( 774.6312213355099630, -71.36187538569302546, -364.6798772138717482 ) ) ;
#9044 = CARTESIAN_POINT ( 'NONE',  ( 760.5453621957607311, -285.0783235625958127, 323.8424801807151425 ) ) ;
#9045 = CARTESIAN_POINT ( 'NONE',  ( 187.2824899080286229, 256.5000000000000000, -199.9999999999953957 ) ) ;
#9046 = DIRECTION ( 'NONE',  ( 0.000000000000000000, 0.000000000000000000, -1.000000000000000000 ) ) ;
#9047 = CARTESIAN_POINT ( 'NONE',  ( 794.9819416627830151, 11.00176097794305541, 319.9864689768909898 ) ) ;
#9048 = VERTEX_POINT ( 'NONE', #42171 ) ;
#9049 = CARTESIAN_POINT ( 'NONE',  ( 766.4474001241216001, -331.0999726633342561, -307.3154664389482491 ) ) ;
#9050 = MECHANICAL_DESIGN_GEOMETRIC_PRESENTATION_REPRESENTATION (  '', ( #9778 ), #44465 ) ;
#9051 = ADVANCED_FACE ( 'NONE', ( #31556 ), #27619, .F. ) ;
#9052 = CARTESIAN_POINT ( 'NONE',  ( 814.2805881961230625, -193.6454272087891582, 331.2368401574024119 ) ) ;
#9054 = CARTESIAN_POINT ( 'NONE',  ( 771.2633955100217236, -287.9073299311468759, -363.4237431249939618 ) ) ;
#9053 = DIRECTION ( 'NONE',  ( 1.000000000000000000, 0.000000000000000000, 0.000000000000000000 ) ) ;
#9055 = FACE_BOUND ( 'NONE', #27483, .T. ) ;
#9056 = CARTESIAN_POINT ( 'NONE',  ( 766.0291762391763086, -202.9181544815164386, -360.7704444035551319 ) ) ;
#9057 = CARTESIAN_POINT ( 'NONE',  ( 808.0189434323515343, -38.08914811296587999, 319.0252816721025511 ) ) ;
#9058 = CARTESIAN_POINT ( 'NONE',  ( -598.8365100919716042, 258.0940000000001646, -206.1189999999899385 ) ) ;
#9059 = CARTESIAN_POINT ( 'NONE',  ( 755.2512626584698410, -367.5436935675102745, -315.2512626584710915 ) ) ;
#9060 = DIRECTION ( 'NONE',  ( 0.000000000000000000, -0.3826834323650836756, -0.9238795325112892920 ) ) ;
#9061 = CARTESIAN_POINT ( 'NONE',  ( 788.8264449731200330, -45.18005720387493085, 363.6646147819171233 ) ) ;
#9062 = CARTESIAN_POINT ( 'NONE',  ( 797.8822607201568644, -318.5545181178796952, 370.1134526219340160 ) ) ;
#9063 = CARTESIAN_POINT ( 'NONE',  ( 744.7301800767019131, -244.8164208402378961, 337.4774526936615757 ) ) ;
#9064 = CARTESIAN_POINT ( 'NONE',  ( 808.0189434323515343, -14.08914811296595460, -319.0252816721025511 ) ) ;
#9065 = CARTESIAN_POINT ( 'NONE',  ( 803.4237431249931660, -231.1800572038743553, -331.2633955100225194 ) ) ;
#9066 = CARTESIAN_POINT ( 'NONE',  ( 187.1337867209877857, -434.4637272565419153, 347.3621835540870961 ) ) ;
#9067 = ADVANCED_FACE ( 'NONE', ( #6391 ), #31766, .F. ) ;
#9068 = CARTESIAN_POINT ( 'NONE',  ( 788.7366044899766848, -347.9073299311467053, 316.5762568750059813 ) ) ;
#9069 = CIRCLE ( 'NONE', #23793, 6.118999999999985562 ) ;
#9070 = CARTESIAN_POINT ( 'NONE',  ( 754.7162404726377645, -134.7363362996984790, 339.4709603349214717 ) ) ;
#9071 = CARTESIAN_POINT ( 'NONE',  ( 755.0488828828309806, -17.80559628986940979, -344.1219089521771934 ) ) ;
#9072 = CARTESIAN_POINT ( 'NONE',  ( 791.9812246680005501, -356.6346026584193964, 361.9419747391813189 ) ) ;
#9073 = PRODUCT_DEFINITION_FORMATION_WITH_SPECIFIED_SOURCE ( 'ANY', '', #31792, .NOT_KNOWN. ) ;
#9074 = LINE ( 'NONE', #26840, #5560 ) ;
#9075 = LINE ( 'NONE', #37246, #19600 ) ;
#9076 = CARTESIAN_POINT ( 'NONE',  ( 778.2165204200184689, -406.8164208402375266, 364.9363028652563230 ) ) ;
#9077 = ORIENTED_EDGE ( 'NONE', *, *, #7983, .F. ) ;
#9078 = CARTESIAN_POINT ( 'NONE',  ( 805.0264073115434940, -318.3510508353230080, -339.4763451958999099 ) ) ;
#9080 = CARTESIAN_POINT ( 'NONE',  ( 791.9812246680005501, -140.6346026584201070, 361.9419747391813189 ) ) ;
#9079 = CARTESIAN_POINT ( 'NONE',  ( 785.3687786644884454, -179.3618753856927128, 315.3201227861279676 ) ) ;
#9081 = CARTESIAN_POINT ( 'NONE',  ( 811.6461892240364477, -364.7146871989592114, -324.1737431748509835 ) ) ;
#9082 = DIRECTION ( 'NONE',  ( -0.000000000000000000, 1.000000000000000000, -0.000000000000000000 ) ) ;
#9083 = ORIENTED_EDGE ( 'NONE', *, *, #39102, .T. ) ;
#9084 = CARTESIAN_POINT ( 'NONE',  ( 755.3201227861273992, -363.7255117493284047, 345.3687786644892981 ) ) ;
#9085 = ORIENTED_EDGE ( 'NONE', *, *, #30846, .F. ) ;
#9086 =( NAMED_UNIT ( * ) SI_UNIT ( $, .STERADIAN. ) SOLID_ANGLE_UNIT ( ) );
#9087 = CARTESIAN_POINT ( 'NONE',  ( 772.4837098697144029, -167.3618753856927412, -374.5518280994205611 ) ) ;
#9088 = CARTESIAN_POINT ( 'NONE',  ( 808.0189434323515343, -110.0891481129656597, 319.0252816721025511 ) ) ;
#9089 = EDGE_LOOP ( 'NONE', ( #44420, #44433 ) ) ;
#9090 = CARTESIAN_POINT ( 'NONE',  ( 767.8955696845334842, -192.4527844766017211, -362.1676090361161755 ) ) ;
#9091 = EDGE_LOOP ( 'NONE', ( #35921, #977, #29837, #29456 ) ) ;
#9092 = CARTESIAN_POINT ( 'NONE',  ( 766.0291762391763086, -442.9181544815157849, -360.7704444035551319 ) ) ;
#9093 = CARTESIAN_POINT ( 'NONE',  ( 787.4397851343537695, -261.7255117493288026, 374.2001403089903988 ) ) ;
#9094 = CARTESIAN_POINT ( 'NONE',  ( 758.6633372737375112, -212.5328690171415076, 326.9102291470432533 ) ) ;
#9096 = FACE_OUTER_BOUND ( 'NONE', #30862, .T. ) ;
#9095 = DIRECTION ( 'NONE',  ( 0.000000000000000000, -1.000000000000000000, 0.000000000000000000 ) ) ;
#9097 = EDGE_CURVE ( 'NONE', #14962, #40161, #38263, .T. ) ;
#9098 = DIRECTION ( 'NONE',  ( -0.000000000000000000, 1.000000000000000000, -0.000000000000000000 ) ) ;
#9099 = VERTEX_POINT ( 'NONE', #24373 ) ;
#9100 = CARTESIAN_POINT ( 'NONE',  ( 802.5472867521000353, -436.3726999360612240, -350.8726784830461156 ) ) ;
#9101 = CARTESIAN_POINT ( 'NONE',  ( 989.9999999999992042, -590.0000000000001137, 201.9999999999998579 ) ) ;
#9102 = VECTOR ( 'NONE', #23422, 1000.000000000000000 ) ;
#9103 = ORIENTED_EDGE ( 'NONE', *, *, #4891, .F. ) ;
#9104 = CARTESIAN_POINT ( 'NONE',  ( 745.5313806188320314, -231.2817908451527558, -333.7943932421247268 ) ) ;
#9105 = AXIS2_PLACEMENT_3D ( 'NONE', #37162, #1387, #30013 ) ;
#9106 = CARTESIAN_POINT ( 'NONE',  ( 750.9282345327678740, -112.9181544815167229, 319.8311093483690115 ) ) ;
#9108 = CARTESIAN_POINT ( 'NONE',  ( 774.6312213355099630, -191.3618753856925991, -364.6798772138717482 ) ) ;
#9107 = CARTESIAN_POINT ( 'NONE',  ( 180.7583438952258916, 294.6698570112193920, -274.9999999999999432 ) ) ;
#9109 = CARTESIAN_POINT ( 'NONE',  ( 756.1348686366196716, -353.2601417444137724, -347.5531968255698416 ) ) ;
#9110 = FACE_OUTER_BOUND ( 'NONE', #12110, .T. ) ;
#9111 = CARTESIAN_POINT ( 'NONE',  ( 744.6391490659812007, -206.7363362996982801, -338.7502325331110455 ) ) ;
#9112 = LINE ( 'NONE', #29678, #11966 ) ;
#9113 = CARTESIAN_POINT ( 'NONE',  ( 999.9999999999992042, 248.9999999999998863, 200.9999999999999432 ) ) ;
#9114 = CARTESIAN_POINT ( 'NONE',  ( 804.8461984189677878, -98.19088175424404596, -336.9566956441385628 ) ) ;
#9115 = CARTESIAN_POINT ( 'NONE',  ( 776.9254006560222479, -452.1908817542428665, 314.8983024940802125 ) ) ;
#9116 = CARTESIAN_POINT ( 'NONE',  ( 807.2620300519052989, -360.0090635724250774, 318.0141637701419768 ) ) ;
#9117 = CARTESIAN_POINT ( 'NONE',  ( 773.4999999999993179, -512.9681489794448908, -339.9999999999999432 ) ) ;
#9118 = CARTESIAN_POINT ( 'NONE',  ( 773.3843516231979720, -421.4419599262317888, -364.4086373105754433 ) ) ;
#9119 = CARTESIAN_POINT ( 'NONE',  ( 749.2812353651451076, -294.4527844766013800, -323.2262854647983090 ) ) ;
#9120 = DIRECTION ( 'NONE',  ( -1.000000000000000000, -0.000000000000000000, -0.000000000000000000 ) ) ;
#9121 = CARTESIAN_POINT ( 'NONE',  ( -786.4999999999993179, -110.5936016518799221, 750.6326042729449455 ) ) ;
#9122 = CARTESIAN_POINT ( 'NONE',  ( 756.3353852180819104, -53.90732993114765037, -331.1735550268788302 ) ) ;
#9123 = AXIS2_PLACEMENT_3D ( 'NONE', #33107, #15329, #37224 ) ;
#9124 = CARTESIAN_POINT ( 'NONE',  ( 745.5313806188320314, -207.2817908451527842, 333.7943932421247268 ) ) ;
#9125 = CARTESIAN_POINT ( 'NONE',  ( 745.1769319972822814, -137.8055962898690154, -346.2694204179732083 ) ) ;
#9126 = CARTESIAN_POINT ( 'NONE',  ( 777.5031285880264704, -166.8164208402382087, 374.9108240113588408 ) ) ;
#9127 = CARTESIAN_POINT ( 'NONE',  ( 777.4774526936600978, -418.2709662947827383, -304.7301800767027657 ) ) ;
#9128 = CARTESIAN_POINT ( 'NONE',  ( 989.9999999999992042, -179.7356316342496712, 69.11609595480017276 ) ) ;
#9129 = CARTESIAN_POINT ( 'NONE',  ( 759.7806653035534055, -246.9982390220560546, 324.8639956371180801 ) ) ;
#9130 = CARTESIAN_POINT ( 'NONE',  ( 776.9254006560222479, -20.19088175424429110, 314.8983024940802125 ) ) ;
#9131 = CARTESIAN_POINT ( 'NONE',  ( 767.8955696845333705, -408.4527844766009252, -362.1676090361162323 ) ) ;
#9132 = DIRECTION ( 'NONE',  ( -0.000000000000000000, 1.000000000000000000, 0.000000000000000000 ) ) ;
#9133 = CARTESIAN_POINT ( 'NONE',  ( 802.2119215644370342, -30.00906357242607925, -367.5423716828165084 ) ) ;
#9134 = PLANE ( 'NONE',  #21787 ) ;
#9135 = CARTESIAN_POINT ( 'NONE',  ( 801.3366627262608972, -104.5328690171418913, 353.0897708529566899 ) ) ;
#9136 = EDGE_LOOP ( 'NONE', ( #44530, #32686, #26588, #20152, #28994, #40255, #11894, #45303, #1864, #16311, #5908, #22664, #25054, #38306 ) ) ;
#9137 = CARTESIAN_POINT ( 'NONE',  ( 756.7813123517142913, -235.9874144716868898, -329.9779781133712504 ) ) ;
#9138 = VECTOR ( 'NONE', #19978, 1000.000000000000000 ) ;
#9139 = CARTESIAN_POINT ( 'NONE',  ( 756.3353852180819104, -53.90732993114765037, 331.1735550268788302 ) ) ;
#9140 = AXIS2_PLACEMENT_3D ( 'NONE', #31515, #31049, #38922 ) ;
#9141 = CARTESIAN_POINT ( 'NONE',  ( 798.0661480581538854, -218.5328690171414792, -309.5768839229118043 ) ) ;
#9142 = CARTESIAN_POINT ( 'NONE',  ( -786.4999999999993179, -513.1383975375929367, -369.9999999999999432 ) ) ;
#9143 = CARTESIAN_POINT ( 'NONE',  ( 812.6845335610512393, -391.9874144716864066, 353.5525998758768651 ) ) ;
#9144 = ORIENTED_EDGE ( 'NONE', *, *, #22713, .T. ) ;
#9145 = CARTESIAN_POINT ( 'NONE',  ( 746.8695393053150156, -5.907329931147798696, 327.6429770376306010 ) ) ;
#9146 = EDGE_CURVE ( 'NONE', #3205, #27542, #3138, .T. ) ;
#9147 = CARTESIAN_POINT ( 'NONE',  ( 803.6646147819161570, -185.9073299311472454, -348.8264449731210561 ) ) ;
#9148 = CARTESIAN_POINT ( 'NONE',  ( 771.2633955100217236, -359.9073299311467053, 363.4237431249939618 ) ) ;
#9149 = ADVANCED_FACE ( 'NONE', ( #6829, #2919 ), #17008, .F. ) ;
#9150 = CARTESIAN_POINT ( 'NONE',  ( 814.5518280994195948, -87.72551174932937101, -332.4837098697145734 ) ) ;
#9151 = CARTESIAN_POINT ( 'NONE',  ( 804.6798772138710092, -63.72551174932941365, -334.6312213355106451 ) ) ;
#9152 = ORIENTED_EDGE ( 'NONE', *, *, #8029, .F. ) ;
#9153 = CARTESIAN_POINT ( 'NONE',  ( 763.8424801807145741, -18.00906357242611477, -320.5453621957614700 ) ) ;
#9154 = ORIENTED_EDGE ( 'NONE', *, *, #34274, .T. ) ;
#9155 = CARTESIAN_POINT ( 'NONE',  ( 796.1575198192839480, -342.0090635724251342, -359.4546378042384163 ) ) ;
#9157 = CARTESIAN_POINT ( 'NONE',  ( 763.8424801807145741, -402.0090635724250205, 320.5453621957614700 ) ) ;
#9156 = CARTESIAN_POINT ( 'NONE',  ( 795.1360043628807261, -92.08914811296568814, 360.2193346964456282 ) ) ;
#9160 = CARTESIAN_POINT ( 'NONE',  ( 805.9055244015594326, -315.6237781080503169, 315.8990559732753240 ) ) ;
#9159 = CARTESIAN_POINT ( 'NONE',  ( 786.4999999999993179, 26.27639943461401018, 900.0000000000001137 ) ) ;
#9158 = CARTESIAN_POINT ( 'NONE',  ( 763.2262854647970016, -416.6346026584192259, 309.2812353651462445 ) ) ;
#9161 = ADVANCED_FACE ( 'NONE', ( #41267 ), #3382, .F. ) ;
#9162 = CARTESIAN_POINT ( 'NONE',  ( 800.9840315886518738, -340.9181544815160123, -354.1144889064786412 ) ) ;
#9163 = CARTESIAN_POINT ( 'NONE',  ( 803.6646147819161570, -305.9073299311467622, -348.8264449731210561 ) ) ;
#9164 = CARTESIAN_POINT ( 'NONE',  ( 799.9636004259356241, -142.9181544815166376, -311.2241431872006956 ) ) ;
#9165 = CARTESIAN_POINT ( 'NONE',  ( 814.5518280994195948, -447.7255117493280636, 332.4837098697145734 ) ) ;
#9167 = CARTESIAN_POINT ( 'NONE',  ( 939.9999999999993179, -422.8782571739196214, -207.4246812887968758 ) ) ;
#9166 = CARTESIAN_POINT ( 'NONE',  ( 784.9999999999992042, 239.9999999999998863, -235.0000000000000000 ) ) ;
#9168 = CARTESIAN_POINT ( 'NONE',  ( 813.5763878283155464, -123.8272453906076009, -351.1614460488615350 ) ) ;
#9169 = CARTESIAN_POINT ( 'NONE',  ( 786.4999999999993179, -563.3203001761230553, -342.3463313526983143 ) ) ;
#9170 = CARTESIAN_POINT ( 'NONE',  ( 998.9999999999992042, -600.0000000000001137, 360.0000000000000000 ) ) ;
#9171 = CARTESIAN_POINT ( 'NONE',  ( 790.9844846989617508, -334.3726999360615082, 317.2208543904092721 ) ) ;
#9172 = AXIS2_PLACEMENT_3D ( 'NONE', #36324, #11391, #4685 ) ;
#9173 = CARTESIAN_POINT ( 'NONE',  ( 805.1927285166397041, -184.8164208402380950, 341.8018195045277707 ) ) ;
#9174 = ORIENTED_EDGE ( 'NONE', *, *, #40721, .F. ) ;
#9175 = CIRCLE ( 'NONE', #43112, 7.999999999999785061 ) ;
#9176 = CARTESIAN_POINT ( 'NONE',  ( 813.5763878283155464, -315.8272453906070609, 351.1614460488615350 ) ) ;
#9177 = AXIS2_PLACEMENT_3D ( 'NONE', #19234, #41859, #16916 ) ;
#9178 = CARTESIAN_POINT ( 'NONE',  ( 792.2312462859673587, -155.9073299311473306, -307.2067596250082602 ) ) ;
#9179 = ADVANCED_FACE ( 'NONE', ( #45656 ), #14006, .F. ) ;
#9180 = PLANE ( 'NONE',  #40076 ) ;
#9181 = CARTESIAN_POINT ( 'NONE',  ( 762.1177392798416577, -66.55451811788050520, 309.8865473780659272 ) ) ;
#9182 = EDGE_CURVE ( 'NONE', #44613, #25018, #20235, .T. ) ;
#9183 = CARTESIAN_POINT ( 'NONE',  ( 808.3070685750230950, -282.9982390220558841, -361.1904061080339261 ) ) ;
#9184 = CARTESIAN_POINT ( 'NONE',  ( 187.1337867209877857, 56.73212367640085318, -362.5753187112032379 ) ) ;
#9185 = CARTESIAN_POINT ( 'NONE',  ( 754.8072714833581358, -148.8164208402382656, 338.1981804954720587 ) ) ;
#9186 = ORIENTED_EDGE ( 'NONE', *, *, #19085, .T. ) ;
#9187 = CARTESIAN_POINT ( 'NONE',  ( 754.3581564841646241, -401.4636090269704027, 316.1443688327762516 ) ) ;
#9188 = CARTESIAN_POINT ( 'NONE',  ( 813.2346286133761168, -341.2601417444138292, -328.9521613784389160 ) ) ;
#9189 = CARTESIAN_POINT ( 'NONE',  ( 759.0252816721024374, -96.99823902205660886, -368.0189434323527280 ) ) ;
#9190 = VECTOR ( 'NONE', #41087, 1000.000000000000000 ) ;
#9191 = CARTESIAN_POINT ( 'NONE',  ( 773.4516893846965786, -67.64542720878958448, 315.8398074228977066 ) ) ;
#9192 = CARTESIAN_POINT ( 'NONE',  ( 787.5162901302840055, -347.3618753856922012, -305.4481719005792684 ) ) ;
#9193 = DIRECTION ( 'NONE',  ( -0.000000000000000000, -0.000000000000000000, 1.000000000000000000 ) ) ;
#9194 = CARTESIAN_POINT ( 'NONE',  ( 795.9930595647434757, -435.0783235625953580, 320.7433823573372820 ) ) ;
#9195 = VERTEX_POINT ( 'NONE', #7755 ) ;
#9196 = VECTOR ( 'NONE', #32491, 1000.000000000000227 ) ;
#9197 = EDGE_CURVE ( 'NONE', #42559, #16836, #6309, .T. ) ;
#9198 = CARTESIAN_POINT ( 'NONE',  ( 815.1787889125755555, -126.8965053807781516, -343.7953271457877804 ) ) ;
#9199 = DIRECTION ( 'NONE',  ( 0.000000000000000000, 0.000000000000000000, 1.000000000000000000 ) ) ;
#9200 = CARTESIAN_POINT ( 'NONE',  ( 801.9858362298568863, -267.0783235625958696, 312.7379699480935642 ) ) ;
#9201 = CARTESIAN_POINT ( 'NONE',  ( 791.9812246680005501, -92.63460265842026331, 361.9419747391813189 ) ) ;
#9202 = VERTEX_POINT ( 'NONE', #29236 ) ;
#9203 = EDGE_CURVE ( 'NONE', #20167, #14643, #43922, .T. ) ;
#9204 = CARTESIAN_POINT ( 'NONE',  ( 783.0433043558608688, -0.8965053807785533513, -315.1538015810313027 ) ) ;
#9205 = CARTESIAN_POINT ( 'NONE',  ( 778.2165204200184689, -262.8164208402379245, 364.9363028652563230 ) ) ;
#9206 = EDGE_CURVE ( 'NONE', #44135, #23261, #18163, .T. ) ;
#9207 = CARTESIAN_POINT ( 'NONE',  ( 814.8230680027162407, -437.8055962898679923, -333.7305795820267917 ) ) ;
#9208 = CARTESIAN_POINT ( 'NONE',  ( 9.202092513630264312E-14, 200.0000000000001421, 0.000000000000000000 ) ) ;
#9209 = VERTEX_POINT ( 'NONE', #39869 ) ;
#9210 = EDGE_LOOP ( 'NONE', ( #13305, #2147, #4895, #43480 ) ) ;
#9211 = CARTESIAN_POINT ( 'NONE',  ( 812.3518521366052028, -361.0999726633341425, -326.5853460496235243 ) ) ;
#9212 = CARTESIAN_POINT ( 'NONE',  ( 797.8594530101008786, -301.5436935675105588, 322.1405469898980982 ) ) ;
#9213 = CARTESIAN_POINT ( 'NONE',  ( 794.9819416627830151, -228.9982390220561683, -319.9864689768909898 ) ) ;
#9214 = EDGE_CURVE ( 'NONE', #38198, #16659, #39181, .T. ) ;
#9216 = CARTESIAN_POINT ( 'NONE',  ( 745.1769319972822814, -209.8055962898687881, 346.2694204179732083 ) ) ;
#9215 = CARTESIAN_POINT ( 'NONE',  ( 745.7998596910086917, -341.3618753856922012, 332.5602148656461168 ) ) ;
#9217 = CARTESIAN_POINT ( 'NONE',  ( 815.1787889125755555, -30.89650538077846065, 343.7953271457877804 ) ) ;
#9218 = CARTESIAN_POINT ( 'NONE',  ( 755.8894580844503253, -207.8272453906073451, -332.3691319403863531 ) ) ;
#9219 = CARTESIAN_POINT ( 'NONE',  ( 803.4237431249931660, -231.1800572038743553, -331.2633955100225194 ) ) ;
#9220 = CARTESIAN_POINT ( 'NONE',  ( 797.6776695296629214, -427.5436935675101040, -357.6776695296636603 ) ) ;
#9221 = ORIENTED_EDGE ( 'NONE', *, *, #29530, .F. ) ;
#9222 = CARTESIAN_POINT ( 'NONE',  ( 756.5762568750052424, -219.1800572038744122, 348.7366044899774238 ) ) ;
#9223 = CARTESIAN_POINT ( 'NONE',  ( 771.2633955100217236, -95.90732993114751537, -363.4237431249939618 ) ) ;
#9224 = ORIENTED_EDGE ( 'NONE', *, *, #19948, .F. ) ;
#9225 = CARTESIAN_POINT ( 'NONE',  ( 796.9462024416508257, -372.4527844766010958, 308.9653473494370246 ) ) ;
#9226 = VECTOR ( 'NONE', #14502, 1000.000000000000000 ) ;
#9227 = CARTESIAN_POINT ( 'NONE',  ( 181.1634899080285948, 256.5000000000000000, -199.9999999999953957 ) ) ;
#9228 = CARTESIAN_POINT ( 'NONE',  ( 768.1267186599862953, 16.45630643248851044, 317.8138973628999224 ) ) ;
#9229 = FACE_OUTER_BOUND ( 'NONE', #21653, .T. ) ;
#9230 = AXIS2_PLACEMENT_3D ( 'NONE', #22034, #4702, #19030 ) ;
#9231 = CARTESIAN_POINT ( 'NONE',  ( 793.9708237608222134, -238.9181544815163534, 319.2295555964448681 ) ) ;
#9232 = VECTOR ( 'NONE', #8957, 1000.000000000000000 ) ;
#9233 = CARTESIAN_POINT ( 'NONE',  ( 768.0187753319979720, -80.63460265842029173, 318.0580252608186242 ) ) ;
#9234 = ORIENTED_EDGE ( 'NONE', *, *, #29650, .T. ) ;
#9235 = CARTESIAN_POINT ( 'NONE',  ( 744.6391490659812007, -446.7363362996975980, -338.7502325331110455 ) ) ;
#9236 = CARTESIAN_POINT ( 'NONE',  ( 754.9967657858570647, -25.54369356751137232, -365.0032342141425943 ) ) ;
#9237 = CARTESIAN_POINT ( 'NONE',  ( 789.9200121543843807, -241.9874144716869182, 317.0176451133914384 ) ) ;
#9238 = CARTESIAN_POINT ( 'NONE',  ( 754.8072714833581358, -436.8164208402372992, -338.1981804954720587 ) ) ;
#9239 = CARTESIAN_POINT ( 'NONE',  ( 801.9419747391806368, 5.547215523397618142, -351.9812246680014027 ) ) ;
#9240 = CARTESIAN_POINT ( 'NONE',  ( 751.6929314249748586, -438.9982390220553157, 318.8095938919659034 ) ) ;
#9241 = CARTESIAN_POINT ( 'NONE',  ( 779.9999999999992042, -462.9681489794448339, -339.9999999999999432 ) ) ;
#9242 = CARTESIAN_POINT ( 'NONE',  ( 796.1575198192839480, -294.0090635724253048, -359.4546378042384163 ) ) ;
#9243 = CARTESIAN_POINT ( 'NONE',  ( 746.8695393053150156, -173.9073299311472169, -327.6429770376306010 ) ) ;
#9244 = VECTOR ( 'NONE', #30830, 1000.000000000000000 ) ;
#9245 = CARTESIAN_POINT ( 'NONE',  ( 772.4837098697144029, -95.36187538569294020, 374.5518280994205611 ) ) ;
#9246 = CARTESIAN_POINT ( 'NONE',  ( 792.2312462859673587, -155.9073299311473306, 307.2067596250082602 ) ) ;
#9247 = CARTESIAN_POINT ( 'NONE',  ( 794.4892657455289964, 16.45630643248850689, -314.6207049315058271 ) ) ;
#9248 = CIRCLE ( 'NONE', #15163, 2.749999999999891642 ) ;
#9249 = DIRECTION ( 'NONE',  ( 0.000000000000000000, 1.000000000000000000, 0.000000000000000000 ) ) ;
#9250 = CARTESIAN_POINT ( 'NONE',  ( 795.6651683502461765, -226.7146871989596661, -371.3240766477733814 ) ) ;
#9251 = AXIS2_PLACEMENT_3D ( 'NONE', #9159, #1755, #19116 ) ;
#9252 = CARTESIAN_POINT ( 'NONE',  ( 747.6481478633932056, -397.0999726633340288, 353.4146539503763620 ) ) ;
#9253 = LINE ( 'NONE', #12265, #37540 ) ;
#9254 = CARTESIAN_POINT ( 'NONE',  ( 812.7932403749906598, -399.1800572038738437, 327.7687537140311633 ) ) ;
#9255 = CARTESIAN_POINT ( 'NONE',  ( 745.0891759886404770, -28.27096629478409540, 342.4968714119734159 ) ) ;
#9256 = CARTESIAN_POINT ( 'NONE',  ( 771.1735550268778070, -369.1800572038739574, -316.3353852180827630 ) ) ;
#9257 = CARTESIAN_POINT ( 'NONE',  ( 798.7617431975189675, 20.37622189194865285, 323.0428371773161871 ) ) ;
#9258 = CIRCLE ( 'NONE', #1143, 8.024999999999948841 ) ;
#9259 = CARTESIAN_POINT ( 'NONE',  ( 746.4236121716829757, -87.82724539060770041, -328.8385539511384650 ) ) ;
#9260 = CARTESIAN_POINT ( 'NONE',  ( 755.8398074228967971, -163.4419599262325846, -333.4516893846970333 ) ) ;
#9261 = CARTESIAN_POINT ( 'NONE',  ( 808.7758568127978833, -172.1692326535052757, 320.0363995740631822 ) ) ;
#9262 = FACE_OUTER_BOUND ( 'NONE', #30378, .T. ) ;
#9263 = CARTESIAN_POINT ( 'NONE',  ( 797.8594530101008786, -61.54369356751124087, -322.1405469898980982 ) ) ;
#9264 = CARTESIAN_POINT ( 'NONE',  ( 769.1273215169530886, -166.7146871989598367, -317.4527132478988847 ) ) ;
#9265 = CARTESIAN_POINT ( 'NONE',  ( 794.9819416627830151, -156.9982390220564241, 319.9864689768909898 ) ) ;
#9266 = VECTOR ( 'NONE', #1677, 1000.000000000000000 ) ;
#9267 = PRODUCT ( 'MirrorTreadle Extension Return Springs', 'MirrorTreadle Extension Return Springs', '', ( #24889 ) ) ;
#9268 = CARTESIAN_POINT ( 'NONE',  ( 814.8230680027162407, -5.805596289869448867, -333.7305795820267917 ) ) ;
#9269 = CARTESIAN_POINT ( 'NONE',  ( 804.9363028652555840, -280.2709662947833067, 338.2165204200192079 ) ) ;
#9270 = AXIS2_PLACEMENT_3D ( 'NONE', #13806, #45446, #34798 ) ;
#9271 = DIRECTION ( 'NONE',  ( 0.000000000000000000, 0.000000000000000000, 1.000000000000000000 ) ) ;
#9272 = VERTEX_POINT ( 'NONE', #43083 ) ;
#9273 = CARTESIAN_POINT ( 'NONE',  ( 763.2154366446407039, -21.62377810805121570, 321.4292242960311228 ) ) ;
#9274 = CARTESIAN_POINT ( 'NONE',  ( 750.9282345327678740, -256.9181544815163534, -319.8311093483690115 ) ) ;
#9275 = ORIENTED_EDGE ( 'NONE', *, *, #14012, .F. ) ;
#9276 = CARTESIAN_POINT ( 'NONE',  ( 745.4481719005789273, -219.7255117493289447, 347.5162901302853697 ) ) ;
#9277 = CARTESIAN_POINT ( 'NONE',  ( 769.0155153010367712, -298.3726999360616787, 362.7791456095907279 ) ) ;
#9278 = CARTESIAN_POINT ( 'NONE',  ( 802.7791456095903868, -412.7146871989590409, 329.0155153010375102 ) ) ;
#9279 = VERTEX_POINT ( 'NONE', #31992 ) ;
#9280 = CARTESIAN_POINT ( 'NONE',  ( 763.0428371773158460, -107.4636090269713122, -358.7617431975195359 ) ) ;
#9281 = CARTESIAN_POINT ( 'NONE',  ( 800.2193346964447755, -114.9982390220565236, -355.1360043628815788 ) ) ;
#9282 = CARTESIAN_POINT ( 'NONE',  ( 805.1927285166399315, -304.8164208402376971, -341.8018195045277707 ) ) ;
#9283 = EDGE_LOOP ( 'NONE', ( #701, #22471, #1074, #6170 ) ) ;
#9284 = CARTESIAN_POINT ( 'NONE',  ( 788.8264449731200330, -429.1800572038737869, -363.6646147819171233 ) ) ;
#9285 = VECTOR ( 'NONE', #6609, 1000.000000000000000 ) ;
#9286 = CARTESIAN_POINT ( 'NONE',  ( 776.9566956441375396, -300.8965053807775689, 364.8461984189686405 ) ) ;
#9287 = LINE ( 'NONE', #6263, #43996 ) ;
#9288 = DIRECTION ( 'NONE',  ( -0.000000000000000000, 1.000000000000000000, -0.000000000000000000 ) ) ;
#9289 = DIRECTION ( 'NONE',  ( 0.000000000000000000, 0.000000000000000000, 1.000000000000000000 ) ) ;
#9290 = EDGE_LOOP ( 'NONE', ( #2276, #4456 ) ) ;
#9291 = CARTESIAN_POINT ( 'NONE',  ( 749.5768839229115201, -348.5545181178796383, -358.0661480581553064 ) ) ;
#9292 = CARTESIAN_POINT ( 'NONE',  ( 776.2046728542105711, -188.1908817542437760, 304.8212110874238761 ) ) ;
#9293 = VECTOR ( 'NONE', #30545, 1000.000000000000000 ) ;
#9294 = CARTESIAN_POINT ( 'NONE',  ( 804.4286716492782716, -305.3618753856922581, -345.3141322388244703 ) ) ;
#9295 = CARTESIAN_POINT ( 'NONE',  ( 799.9999999999993179, -462.9681489794448339, 309.9999999999998863 ) ) ;
#9296 = CARTESIAN_POINT ( 'NONE',  ( 793.0897708529556667, -174.5545181178801784, -361.3366627262616362 ) ) ;
#9297 = CARTESIAN_POINT ( 'NONE',  ( 746.8695393053150156, -53.90732993114765037, 327.6429770376306010 ) ) ;
#9298 = CARTESIAN_POINT ( 'NONE',  ( 779.9999999999992042, 126.4563064324884465, -339.9999999999999432 ) ) ;
#9299 = CARTESIAN_POINT ( 'NONE',  ( 792.2312462859673587, -395.9073299311465348, -307.2067596250082602 ) ) ;
#9300 = CARTESIAN_POINT ( 'NONE',  ( 799.9999999999993179, -462.9681489794448339, 309.9999999999998863 ) ) ;
#9301 = CARTESIAN_POINT ( 'NONE',  ( 755.5713283507202505, -29.36187538569318178, 334.6858677611754729 ) ) ;
#9302 = CARTESIAN_POINT ( 'NONE',  ( 786.2694204179717872, -333.2817908451523863, 305.1769319972829067 ) ) ;
#9303 = CARTESIAN_POINT ( 'NONE',  ( 805.0032342141412300, -277.5436935675105019, 314.9967657858571783 ) ) ;
#9304 = CARTESIAN_POINT ( 'NONE',  ( 812.7932403749906598, -15.18005720387504631, -327.7687537140311633 ) ) ;
#9305 = CARTESIAN_POINT ( 'NONE',  ( 802.1676090361156639, -254.6346026584196238, -327.8955696845344505 ) ) ;
#9306 = DIRECTION ( 'NONE',  ( 0.000000000000000000, 0.7071067811865513475, 0.7071067811865435759 ) ) ;
#9307 = CARTESIAN_POINT ( 'NONE',  ( 802.1676090361156639, -374.6346026584192828, 327.8955696845344505 ) ) ;
#9308 = CARTESIAN_POINT ( 'NONE',  ( 763.0428371773158460, -107.4636090269713122, 358.7617431975195359 ) ) ;
#9309 = CARTESIAN_POINT ( 'NONE',  ( 803.8651313633788504, -53.26014174441475291, -332.4468031744301015 ) ) ;
#9310 = CARTESIAN_POINT ( 'NONE',  ( 745.1769319972822814, -41.80559628986934229, 346.2694204179732083 ) ) ;
#9311 = CARTESIAN_POINT ( 'NONE',  ( 802.1676090361155502, -374.6346026584193396, 327.8955696845344505 ) ) ;
#9312 = FACE_BOUND ( 'NONE', #36246, .T. ) ;
#9313 = FACE_OUTER_BOUND ( 'NONE', #15449, .T. ) ;
#9314 = CARTESIAN_POINT ( 'NONE',  ( 762.3223304703356007, -439.5436935675101040, 322.3223304703362828 ) ) ;
#9315 = VERTEX_POINT ( 'NONE', #11681 ) ;
#9316 = CIRCLE ( 'NONE', #1174, 6.118999999999985562 ) ;
#9317 = CARTESIAN_POINT ( 'NONE',  ( 755.8398074228967971, -331.4419599262320162, -333.4516893846970333 ) ) ;
#9319 = CARTESIAN_POINT ( 'NONE',  ( 778.1981804954715471, -202.2709662947835341, 314.8072714833591021 ) ) ;
#9318 = CARTESIAN_POINT ( 'NONE',  ( 794.9819416627830151, -204.9982390220562820, 319.9864689768909898 ) ) ;
#9320 = ADVANCED_FACE ( 'NONE', ( #7310 ), #14225, .F. ) ;
#9321 = CARTESIAN_POINT ( 'NONE',  ( 788.7631598425961101, -361.4419599262319593, -305.7194118038759143 ) ) ;
#9322 = DIRECTION ( 'NONE',  ( -0.000000000000000000, 1.000000000000000000, -0.000000000000000000 ) ) ;
#9323 = ORIENTED_EDGE ( 'NONE', *, *, #9654, .T. ) ;
#9324 = CARTESIAN_POINT ( 'NONE',  ( 762.1405469898971887, -385.5436935675102745, 357.8594530101015607 ) ) ;
#9325 = ORIENTED_EDGE ( 'NONE', *, *, #29475, .F. ) ;
#9326 = VECTOR ( 'NONE', #39284, 1000.000000000000000 ) ;
#9327 = CARTESIAN_POINT ( 'NONE',  ( 808.3070685750230950, -234.9982390220561683, -361.1904061080339261 ) ) ;
#9328 = CARTESIAN_POINT ( 'NONE',  ( 796.7737145352015204, -116.6346026584201780, 370.7187646348536987 ) ) ;
#9329 = VERTEX_POINT ( 'NONE', #22278 ) ;
#9330 = CARTESIAN_POINT ( 'NONE',  ( 755.0636971347428243, -220.2709662947834772, -341.7834795799807353 ) ) ;
#9331 = VERTEX_POINT ( 'NONE', #18389 ) ;
#9332 = CARTESIAN_POINT ( 'NONE',  ( 778.2165204200184689, -310.8164208402377540, -364.9363028652563230 ) ) ;
#9333 = CARTESIAN_POINT ( 'NONE',  ( 769.9779781133707957, -451.0999726633339151, -316.7813123517150871 ) ) ;
#9334 = CARTESIAN_POINT ( 'NONE',  ( 777.4774526936600978, -250.2709662947832783, 304.7301800767027657 ) ) ;
#9335 = CARTESIAN_POINT ( 'NONE',  ( 795.9930595647434757, -195.0783235625961538, 320.7433823573372820 ) ) ;
#9337 = CARTESIAN_POINT ( 'NONE',  ( 794.9999999999993179, 240.0000000000000853, -275.0000000000000000 ) ) ;
#9336 = DIRECTION ( 'NONE',  ( -1.000000000000000000, -0.000000000000000000, -0.000000000000000000 ) ) ;
#9338 = PLANE ( 'NONE',  #5856 ) ;
#9339 = ORIENTED_EDGE ( 'NONE', *, *, #23300, .F. ) ;
#9340 = CARTESIAN_POINT ( 'NONE',  ( 759.0159684113467620, -448.9181544815156144, -325.8855110935213020 ) ) ;
#9341 = CARTESIAN_POINT ( 'NONE',  ( 762.3515768340985232, 20.87080523294372014, -315.3598267498177847 ) ) ;
#9342 = CARTESIAN_POINT ( 'NONE',  ( -728.8365100919714905, 260.0000000000001705, -199.9999999999890861 ) ) ;
#9343 = ORIENTED_EDGE ( 'NONE', *, *, #13311, .F. ) ;
#9344 = CARTESIAN_POINT ( 'NONE',  ( 749.5768839229115201, -228.5545181178799794, -358.0661480581553064 ) ) ;
#9345 = CARTESIAN_POINT ( 'NONE',  ( 805.6418435158337843, -101.4636090269713264, 363.8556311672236916 ) ) ;
#9346 = AXIS2_PLACEMENT_3D ( 'NONE', #40690, #33532, #25915 ) ;
#9348 = CARTESIAN_POINT ( 'NONE',  ( 754.8072714833581358, -196.8164208402380950, -338.1981804954720587 ) ) ;
#9347 = DIRECTION ( 'NONE',  ( 0.000000000000000000, 0.000000000000000000, 1.000000000000000000 ) ) ;
#9349 = CARTESIAN_POINT ( 'NONE',  ( 764.0069404352550464, -375.0783235625955285, -359.2566176426627180 ) ) ;
#9350 = CARTESIAN_POINT ( 'NONE',  ( 757.7880784355613741, -210.0090635724255321, -312.4576283171834916 ) ) ;
#9351 = CARTESIAN_POINT ( 'NONE',  ( 939.9999999999992042, -185.0721577059061929, -75.19946970736496894 ) ) ;
#9352 = CARTESIAN_POINT ( 'NONE',  ( 759.9999999999992042, 166.4563064324884465, -319.9999999999999432 ) ) ;
#9353 = CARTESIAN_POINT ( 'NONE',  ( 758.4439275373578084, -84.55451811788046257, -353.2243759319684386 ) ) ;
#9354 = AXIS2_PLACEMENT_3D ( 'NONE', #24545, #31714, #38428 ) ;
#9355 = CARTESIAN_POINT ( 'NONE',  ( 757.4527132478984868, -424.3726999360612808, 329.1273215169538844 ) ) ;
#9356 = VECTOR ( 'NONE', #8942, 1000.000000000000000 ) ;
#9357 = CARTESIAN_POINT ( 'NONE',  ( 521.6730038022808458, 239.9999999999999432, -122.7905160835442615 ) ) ;
#9358 = CARTESIAN_POINT ( 'NONE',  ( 745.7998596910086917, -269.3618753856924286, -332.5602148656461168 ) ) ;
#9359 = DIRECTION ( 'NONE',  ( -1.000000000000000000, 0.000000000000000000, 0.000000000000000000 ) ) ;
#9360 = DIRECTION ( 'NONE',  ( -0.000000000000000000, 1.000000000000000000, -0.000000000000000000 ) ) ;
#9361 = CARTESIAN_POINT ( 'NONE',  ( 803.6646147819161570, -65.90732993114758642, -348.8264449731210561 ) ) ;
#9362 = VECTOR ( 'NONE', #44617, 1000.000000000000227 ) ;
#9363 = CARTESIAN_POINT ( 'NONE',  ( 755.8990559732751535, -227.4636090269709143, 365.9055244015606831 ) ) ;
#9364 = CARTESIAN_POINT ( 'NONE',  ( 803.8556311672234642, -153.6237781080508000, -365.6418435158340117 ) ) ;
#9365 = CARTESIAN_POINT ( 'NONE',  ( 810.7187646348534145, -162.4527844766018632, 356.7737145352016341 ) ) ;
#9366 = CARTESIAN_POINT ( 'NONE',  ( 747.2067596250078623, -411.1800572038738437, -352.2312462859687230 ) ) ;
#9367 = CIRCLE ( 'NONE', #35174, 10.00000000000000888 ) ;
#9368 = PLANE ( 'NONE',  #35735 ) ;
#9369 = CARTESIAN_POINT ( 'NONE',  ( 755.5713283507202505, -245.3618753856925139, 334.6858677611754729 ) ) ;
#9370 = CARTESIAN_POINT ( 'NONE',  ( 761.4292242960306112, -41.46360902697149697, 323.2154366446414429 ) ) ;
#9371 = CARTESIAN_POINT ( 'NONE',  ( 759.7806653035534055, -414.9982390220555430, -324.8639956371180801 ) ) ;
#9372 = LINE ( 'NONE', #8701, #42396 ) ;
#9373 = LINE ( 'NONE', #16071, #43188 ) ;
#9374 = CARTESIAN_POINT ( 'NONE',  ( 800.7704444035546203, -100.1692326535055315, 326.0291762391768771 ) ) ;
#9375 = ORIENTED_EDGE ( 'NONE', *, *, #8380, .F. ) ;
#9376 = EDGE_CURVE ( 'NONE', #37957, #42212, #21806, .T. ) ;
#9377 = CARTESIAN_POINT ( 'NONE',  ( 772.3691319403857278, -215.2601417444141987, -315.8894580844506663 ) ) ;
#9378 = CARTESIAN_POINT ( 'NONE',  ( 771.1735550268778070, -129.1800572038746111, -316.3353852180827630 ) ) ;
#9379 = CARTESIAN_POINT ( 'NONE',  ( 803.6646147819161570, -65.90732993114758642, 348.8264449731210561 ) ) ;
#9380 = CARTESIAN_POINT ( 'NONE',  ( 813.2346286133761168, -245.2601417444141987, -328.9521613784389160 ) ) ;
#9381 = CARTESIAN_POINT ( 'NONE',  ( 810.1134526219336749, -368.5328690171409676, 357.8822607201570349 ) ) ;
#9382 = ORIENTED_EDGE ( 'NONE', *, *, #30289, .F. ) ;
#9383 = CARTESIAN_POINT ( 'NONE',  ( 814.2001403089898304, 6.638124614306706306, 347.4397851343538264 ) ) ;
#9384 = CARTESIAN_POINT ( 'NONE',  ( 804.9363028652555840, -184.2709662947835909, -338.2165204200192079 ) ) ;
#9385 = CARTESIAN_POINT ( 'NONE',  ( 802.1676090361156639, -374.6346026584192828, 327.8955696845344505 ) ) ;
#9386 = VECTOR ( 'NONE', #26715, 1000.000000000000114 ) ;
#9387 = CARTESIAN_POINT ( 'NONE',  ( 814.2001403089898304, -113.3618753856929260, -347.4397851343538264 ) ) ;
#9388 = CARTESIAN_POINT ( 'NONE',  ( 778.1981804954715471, -58.27096629478398881, -314.8072714833591021 ) ) ;
#9389 = CARTESIAN_POINT ( 'NONE',  ( 758.4439275373578084, -60.55451811788051941, -353.2243759319684386 ) ) ;
#9390 = CARTESIAN_POINT ( 'NONE',  ( 790.0220218866281812, -343.0999726633342561, -363.2186876482849129 ) ) ;
#9392 = CARTESIAN_POINT ( 'NONE',  ( 793.0897708529556667, -414.5545181178795247, 361.3366627262616362 ) ) ;
#9391 = CARTESIAN_POINT ( 'NONE',  ( 804.4286716492782716, -89.36187538569299704, 345.3141322388244703 ) ) ;
#9393 = CARTESIAN_POINT ( 'NONE',  ( 802.7791456095903868, -100.7146871989600356, 329.0155153010375102 ) ) ;
#9394 = AXIS2_PLACEMENT_3D ( 'NONE', #36836, #36620, #43534 ) ;
#9397 = CARTESIAN_POINT ( 'NONE',  ( 813.9316612368132837, -367.4419599262319025, 348.6739635108323228 ) ) ;
#9396 = DIRECTION ( 'NONE',  ( -1.058954862565134068E-16, 0.6438296778008191223, -0.7651688349527137056 ) ) ;
#9395 = CARTESIAN_POINT ( 'NONE',  ( 763.0537975583476964, -432.4527844766009252, 371.0346526505628617 ) ) ;
#9398 = CARTESIAN_POINT ( 'NONE',  ( 768.8385539511368734, -119.2601417444145397, 306.4236121716840557 ) ) ;
#9399 = CARTESIAN_POINT ( 'NONE',  ( 754.7162404726377645, -326.7363362996979390, -339.4709603349214717 ) ) ;
#9400 = CARTESIAN_POINT ( 'NONE',  ( 803.4237431249931660, -327.1800572038741279, -331.2633955100225194 ) ) ;
#9401 = CARTESIAN_POINT ( 'NONE',  ( 807.2620300519052989, -120.0090635724258021, -318.0141637701419768 ) ) ;
#9402 = CARTESIAN_POINT ( 'NONE',  ( 771.3260364891663130, 4.354572791210176597, 306.0683387631859773 ) ) ;
#9404 = CARTESIAN_POINT ( 'NONE',  ( 1007.605605532488426, -436.2161768796786987, 399.7184814855371542 ) ) ;
#9403 = DIRECTION ( 'NONE',  ( 0.000000000000000000, 0.000000000000000000, 1.000000000000000000 ) ) ;
#9405 = CARTESIAN_POINT ( 'NONE',  ( 810.4231160770870019, -120.5545181178803205, -321.9338519418446936 ) ) ;
#9406 = CARTESIAN_POINT ( 'NONE',  ( 779.9999999999992042, 126.4563064324884465, -339.9999999999999432 ) ) ;
#9407 = LINE ( 'NONE', #31329, #11262 ) ;
#9408 = CARTESIAN_POINT ( 'NONE',  ( 759.0159684113467620, -328.9181544815160692, 325.8855110935213020 ) ) ;
#9409 = CARTESIAN_POINT ( 'NONE',  ( 800.2193346964447755, -186.9982390220563104, 355.1360043628815788 ) ) ;
#9410 = ORIENTED_EDGE ( 'NONE', *, *, #34612, .T. ) ;
#9411 = CARTESIAN_POINT ( 'NONE',  ( 814.8207195650702488, -290.1908817542434349, 336.2433038121456548 ) ) ;
#9412 = CARTESIAN_POINT ( 'NONE',  ( 808.3070685750232087, -162.9982390220563673, -361.1904061080339829 ) ) ;
#9413 = DIRECTION ( 'NONE',  ( 0.000000000000000000, -1.000000000000000000, -1.110223024625155554E-15 ) ) ;
#9414 = CARTESIAN_POINT ( 'NONE',  ( 812.3518521366052028, -97.09997266333496668, 326.5853460496235243 ) ) ;
#9415 = CARTESIAN_POINT ( 'NONE',  ( 808.0189434323515343, -302.0891481129650629, -319.0252816721025511 ) ) ;
#9416 = EDGE_CURVE ( 'NONE', #601, #25954, #7813, .T. ) ;
#9417 = DIRECTION ( 'NONE',  ( -1.000000000000000000, 2.412474565481389965E-32, -2.750100768424434704E-32 ) ) ;
#9418 = CARTESIAN_POINT ( 'NONE',  ( 762.3223304703356007, -151.5436935675109851, 322.3223304703362828 ) ) ;
#9419 = EDGE_LOOP ( 'NONE', ( #28813, #24598, #19852, #26539, #36879, #17634 ) ) ;
#9420 = CARTESIAN_POINT ( 'NONE',  ( 745.5313806188320314, -423.2817908451521589, 333.7943932421247268 ) ) ;
#9421 = CARTESIAN_POINT ( 'NONE',  ( 747.3154664389472828, -355.9874144716865203, -326.4474001241230781 ) ) ;
#9422 = VECTOR ( 'NONE', #15736, 1000.000000000000000 ) ;
#9423 = CARTESIAN_POINT ( 'NONE',  ( 754.9967657858570647, -121.5436935675110419, -365.0032342141425374 ) ) ;
#9424 = CARTESIAN_POINT ( 'NONE',  ( 804.4086373105744769, -49.64542720878965554, 333.3843516231986541 ) ) ;
#9425 = CARTESIAN_POINT ( 'NONE',  ( 812.7932403749906598, -375.1800572038739574, -327.7687537140311633 ) ) ;
#9426 = CARTESIAN_POINT ( 'NONE',  ( 779.9999999999992042, -452.9681489794448339, -339.9999999999999432 ) ) ;
#9427 = CARTESIAN_POINT ( 'NONE',  ( 804.1601925771018387, -439.4419599262316751, 346.5483106153029098 ) ) ;
#9428 = VERTEX_POINT ( 'NONE', #28999 ) ;
#9429 = CARTESIAN_POINT ( 'NONE',  ( 772.3691319403857278, -71.26014174441469606, 315.8894580844506663 ) ) ;
#9430 = ADVANCED_FACE ( 'NONE', ( #42394 ), #21387, .F. ) ;
#9431 = EDGE_CURVE ( 'NONE', #4463, #22016, #4737, .T. ) ;
#9432 = CARTESIAN_POINT ( 'NONE',  ( 793.4146539503750546, -169.9874144716871172, -307.6481478633938877 ) ) ;
#9433 = LINE ( 'NONE', #2257, #1923 ) ;
#9434 = CARTESIAN_POINT ( 'NONE',  ( 752.4576283171824116, -285.0783235625958127, 317.7880784355627952 ) ) ;
#9435 = CARTESIAN_POINT ( 'NONE',  ( 774.6858677611749044, -81.72551174932937101, 315.5713283507209894 ) ) ;
#9436 = EDGE_LOOP ( 'NONE', ( #23360, #45651, #40241, #764, #33427, #15880 ) ) ;
#9437 = CARTESIAN_POINT ( 'NONE',  ( 791.9812246680005501, -260.6346026584197375, 361.9419747391813189 ) ) ;
#9438 = CARTESIAN_POINT ( 'NONE',  ( 758.0141637701419768, -423.0783235625953580, -367.2620300519063790 ) ) ;
#9439 = FACE_OUTER_BOUND ( 'NONE', #367, .T. ) ;
#9440 = EDGE_CURVE ( 'NONE', #39281, #6808, #18838, .T. ) ;
#9441 = ORIENTED_EDGE ( 'NONE', *, *, #23778, .T. ) ;
#9442 = CARTESIAN_POINT ( 'NONE',  ( 794.9819416627830151, -180.9982390220563389, -319.9864689768909898 ) ) ;
#9443 = CARTESIAN_POINT ( 'NONE',  ( 776.2046728542105711, -380.1908817542431507, -304.8212110874238761 ) ) ;
#9444 =( BOUNDED_CURVE ( )  B_SPLINE_CURVE ( 3, ( #6837, #27402, #27626, #45663 ),
 .UNSPECIFIED., .F., .T. ) 
 B_SPLINE_CURVE_WITH_KNOTS ( ( 4, 4 ),
 ( 0.000000000000000000, 1.570796326794896558 ),
 .UNSPECIFIED. ) 
 CURVE ( )  GEOMETRIC_REPRESENTATION_ITEM ( )  RATIONAL_B_SPLINE_CURVE ( ( 1.000000000000000000, 0.8047378541243649375, 0.8047378541243649375, 1.000000000000000000 ) ) 
 REPRESENTATION_ITEM ( '' )  );
#9445 = EDGE_CURVE ( 'NONE', #43744, #44135, #14700, .T. ) ;
#9447 = CARTESIAN_POINT ( 'NONE',  ( 815.1787889125755555, -222.8965053807778531, 343.7953271457877804 ) ) ;
#9446 = CARTESIAN_POINT ( 'NONE',  ( 787.4397851343537695, -333.7255117493286320, 374.2001403089903988 ) ) ;
#9448 = CARTESIAN_POINT ( 'NONE',  ( 761.4292242960306112, -233.4636090269708575, -323.2154366446414429 ) ) ;
#9449 = CARTESIAN_POINT ( 'NONE',  ( 795.1360043628807261, -212.0891481129652902, -360.2193346964456282 ) ) ;
#9450 = CARTESIAN_POINT ( 'NONE',  ( 802.1676090361155502, -422.6346026584191691, -327.8955696845344505 ) ) ;
#9451 = ORIENTED_EDGE ( 'NONE', *, *, #30318, .F. ) ;
#9452 = CARTESIAN_POINT ( 'NONE',  ( 755.0636971347428243, -196.2709662947835909, 341.7834795799807353 ) ) ;
#9453 = CARTESIAN_POINT ( 'NONE',  ( 788.7366044899766848, -107.9073299311474727, -316.5762568750059813 ) ) ;
#9454 = ORIENTED_EDGE ( 'NONE', *, *, #8319, .F. ) ;
#9455 = CIRCLE ( 'NONE', #35267, 10.00000000000000888 ) ;
#9456 = CARTESIAN_POINT ( 'NONE',  ( 814.9108240113580450, -352.2709662947830225, 337.5031285880265273 ) ) ;
#9457 = PLANE ( 'NONE',  #18937 ) ;
#9458 = CARTESIAN_POINT ( 'NONE',  ( 785.1593951492109227, 16.45630643248848912, 313.8313994339321766 ) ) ;
#9459 = DIRECTION ( 'NONE',  ( 0.000000000000000000, 0.000000000000000000, 1.000000000000000000 ) ) ;
#9460 = CARTESIAN_POINT ( 'NONE',  ( 787.5531968255692163, -213.8272453906073167, 316.1348686366205811 ) ) ;
#9461 = CARTESIAN_POINT ( 'NONE',  ( 759.9864689768902508, -98.08914811296568814, 354.9819416627836404 ) ) ;
#9462 = ORIENTED_EDGE ( 'NONE', *, *, #27723, .T. ) ;
#9463 = CARTESIAN_POINT ( 'NONE',  ( 813.5763878283155464, -459.8272453906066062, -351.1614460488615350 ) ) ;
#9464 = CARTESIAN_POINT ( 'NONE',  ( 746.8695393053151292, -53.90732993114765037, -327.6429770376306578 ) ) ;
#9465 = CARTESIAN_POINT ( 'NONE',  ( 799.4546378042377910, -249.0783235625959549, 356.1575198192848006 ) ) ;
#9466 = CARTESIAN_POINT ( 'NONE',  ( 802.1676090361156639, -422.6346026584192259, -327.8955696845344505 ) ) ;
#9467 = CARTESIAN_POINT ( 'NONE',  ( 788.8264449731201466, -45.18005720387493795, -363.6646147819170665 ) ) ;
#9468 = ADVANCED_FACE ( 'NONE', ( #42854, #39404 ), #42639, .F. ) ;
#9469 = CARTESIAN_POINT ( 'NONE',  ( 814.8207195650702488, -2.190881754244347945, 336.2433038121456548 ) ) ;
#9470 = CARTESIAN_POINT ( 'NONE',  ( 791.9812246680005501, 3.365397341579444479, -361.9419747391813189 ) ) ;
#9471 = CARTESIAN_POINT ( 'NONE',  ( 801.5560724626406000, -288.5545181178798657, -326.7756240680316182 ) ) ;
#9472 = CARTESIAN_POINT ( 'NONE',  ( 748.9653473494363425, -194.6346026584198796, -356.9462024416521331 ) ) ;
#9473 = ADVANCED_FACE ( 'NONE', ( #39644 ), #38960, .F. ) ;
#9474 = CARTESIAN_POINT ( 'NONE',  ( 767.7687537140311633, -95.90732993114751537, 372.7932403749916830 ) ) ;
#9475 = CARTESIAN_POINT ( 'NONE',  ( 811.0346526505616112, -158.6346026584199933, 323.0537975583477532 ) ) ;
#9476 = CARTESIAN_POINT ( 'NONE',  ( 784.9999999999992042, 205.0000000000000568, -245.0000000000000284 ) ) ;
#9477 = CARTESIAN_POINT ( 'NONE',  ( 759.8311093483677041, -238.1692326535050768, -310.9282345327691814 ) ) ;
#9478 = CARTESIAN_POINT ( 'NONE',  ( 768.9521613784389729, -417.8272453906067199, 373.2346286133773106 ) ) ;
#9479 = CARTESIAN_POINT ( 'NONE',  ( 777.4774526936600978, -298.2709662947830793, -304.7301800767027657 ) ) ;
#9480 = FACE_OUTER_BOUND ( 'NONE', #7461, .T. ) ;
#9481 = CARTESIAN_POINT ( 'NONE',  ( 811.0346526505616112, -398.6346026584193396, 323.0537975583477532 ) ) ;
#9482 = CARTESIAN_POINT ( 'NONE',  ( 745.0891759886404770, -4.270966294784170003, 342.4968714119734159 ) ) ;
#9483 = CARTESIAN_POINT ( 'NONE',  ( 797.6776695296629214, -355.5436935675103882, -357.6776695296636603 ) ) ;
#9484 = EDGE_CURVE ( 'NONE', #38048, #22371, #599, .T. ) ;
#9485 = CARTESIAN_POINT ( 'NONE',  ( 805.1016975059191054, -6.896505380778533478, 343.0745993439771837 ) ) ;
#9486 = CARTESIAN_POINT ( 'NONE',  ( 764.1737431748507561, -82.37269993606227558, -371.6461892240376415 ) ) ;
#9487 = CARTESIAN_POINT ( 'NONE',  ( 793.2243759319678702, -170.5328690171416781, -318.4439275373583200 ) ) ;
#9488 = CARTESIAN_POINT ( 'NONE',  ( 791.1614460488616487, -155.2601417444144261, 373.5763878283158874 ) ) ;
#9489 = DIRECTION ( 'NONE',  ( 0.000000000000000000, -1.000000000000000000, 0.000000000000000000 ) ) ;
#9490 = AXIS2_PLACEMENT_3D ( 'NONE', #31456, #41, #42544 ) ;
#9491 = ORIENTED_EDGE ( 'NONE', *, *, #35724, .F. ) ;
#9492 = CARTESIAN_POINT ( 'NONE',  ( 774.6312213355099630, -47.36187538569312494, -364.6798772138717482 ) ) ;
#9493 = CARTESIAN_POINT ( 'NONE',  ( 760.5453621957607311, -165.0783235625962391, -323.8424801807151425 ) ) ;
#9494 = CARTESIAN_POINT ( 'NONE',  ( 755.0636971347428243, -148.2709662947837330, 341.7834795799807353 ) ) ;
#9495 = CARTESIAN_POINT ( 'NONE',  ( 813.2346286133761168, -5.260141744414903897, -328.9521613784389160 ) ) ;
#9496 = CARTESIAN_POINT ( 'NONE',  ( 795.1360043628808398, -284.0891481129651197, 360.2193346964456282 ) ) ;
#9497 = FACE_OUTER_BOUND ( 'NONE', #34391, .T. ) ;
#9498 = ORIENTED_EDGE ( 'NONE', *, *, #33454, .F. ) ;
#9499 = CARTESIAN_POINT ( 'NONE',  ( 772.3691319403857278, -23.26014174441484883, 315.8894580844506663 ) ) ;
#9500 = CARTESIAN_POINT ( 'NONE',  ( 750.9282345327678740, -280.9181544815162965, -319.8311093483690115 ) ) ;
#9501 = ORIENTED_EDGE ( 'NONE', *, *, #22196, .T. ) ;
#9502 = DIRECTION ( 'NONE',  ( 0.000000000000000000, 0.000000000000000000, 1.000000000000000000 ) ) ;
#9503 = CARTESIAN_POINT ( 'NONE',  ( 814.5518280994195948, -207.7255117493289731, 332.4837098697145166 ) ) ;
#9504 = CARTESIAN_POINT ( 'NONE',  ( 802.5472867521000353, -340.3726999360615082, 350.8726784830461156 ) ) ;
#9505 = CARTESIAN_POINT ( 'NONE',  ( 811.6461892240364477, 19.28531280103956647, 324.1737431748509835 ) ) ;
#9506 = ORIENTED_EDGE ( 'NONE', *, *, #10551, .F. ) ;
#9507 = CARTESIAN_POINT ( 'NONE',  ( 783.0745993439762742, -104.1908817542440175, -365.1016975059196739 ) ) ;
#9508 = CARTESIAN_POINT ( 'NONE',  ( 778.2165204200184689, -118.8164208402383508, -364.9363028652563230 ) ) ;
#9509 = CARTESIAN_POINT ( 'NONE',  ( 801.9419747391806368, -330.4527844766013231, -351.9812246680014027 ) ) ;
#9510 = VERTEX_POINT ( 'NONE', #25531 ) ;
#9511 = CARTESIAN_POINT ( 'NONE',  ( 781.7834795799800531, -442.8164208402372992, -315.0636971347436202 ) ) ;
#9512 = CARTESIAN_POINT ( 'NONE',  ( 765.8855110935204493, -310.1692326535048778, 319.0159684113471599 ) ) ;
#9513 = CARTESIAN_POINT ( 'NONE',  ( 793.3689467304194523, -456.0926483283658968, 371.2611151693469083 ) ) ;
#9514 = CARTESIAN_POINT ( 'NONE',  ( -78.83651009197140525, 258.0940000000000509, -199.9999999999936051 ) ) ;
#9515 = CARTESIAN_POINT ( 'NONE',  ( 787.5531968255692163, -117.8272453906076151, 316.1348686366205811 ) ) ;
#9516 = CARTESIAN_POINT ( 'NONE',  ( 788.7366044899766848, 12.09267006885214180, 316.5762568750059813 ) ) ;
#9517 = ORIENTED_EDGE ( 'NONE', *, *, #45271, .F. ) ;
#9518 = CARTESIAN_POINT ( 'NONE',  ( 748.6759233522253680, -328.3726999360615650, -324.3348316497537098 ) ) ;
#9519 = CARTESIAN_POINT ( 'NONE',  ( 760.0363995740630116, -202.9181544815164386, 368.7758568127991907 ) ) ;
#9520 = AXIS2_PLACEMENT_3D ( 'NONE', #38807, #7386, #38562 ) ;
#9521 = CARTESIAN_POINT ( 'NONE',  ( 759.9864689768902508, -338.0891481129649492, -354.9819416627836404 ) ) ;
#9522 = EDGE_CURVE ( 'NONE', #6890, #27336, #35928, .T. ) ;
#9523 =( NAMED_UNIT ( * ) SI_UNIT ( $, .STERADIAN. ) SOLID_ANGLE_UNIT ( ) );
#9524 = CARTESIAN_POINT ( 'NONE',  ( 757.0176451133909268, -181.0999726633347109, -349.9200121543848354 ) ) ;
#9525 = CARTESIAN_POINT ( 'NONE',  ( 787.5162901302840055, -35.36187538569316047, 305.4481719005792684 ) ) ;
#9526 = DIRECTION ( 'NONE',  ( -0.000000000000000000, -1.000000000000000000, -0.000000000000000000 ) ) ;
#9527 = CARTESIAN_POINT ( 'NONE',  ( 754.9967657858570647, -385.5436935675102745, -365.0032342141425943 ) ) ;
#9528 = CARTESIAN_POINT ( 'NONE',  ( 799.9999999999993179, 205.0000000000000568, 339.9999999999999432 ) ) ;
#9529 = CARTESIAN_POINT ( 'NONE',  ( 804.1009440267234822, -335.4636090269705733, 314.0944755984392600 ) ) ;
#9530 = DIRECTION ( 'NONE',  ( -0.000000000000000000, 1.000000000000000000, -0.000000000000000000 ) ) ;
#9531 = CARTESIAN_POINT ( 'NONE',  ( 812.7932403749906598, -303.1800572038740711, 327.7687537140311633 ) ) ;
#9532 = CARTESIAN_POINT ( 'NONE',  ( 808.3070685750230950, -18.99823902205683979, -361.1904061080339261 ) ) ;
#9533 = CARTESIAN_POINT ( 'NONE',  ( 797.6776695296629214, -235.5436935675107293, -357.6776695296636603 ) ) ;
#9534 = DIRECTION ( 'NONE',  ( 0.000000000000000000, 0.000000000000000000, 1.000000000000000000 ) ) ;
#9535 = CARTESIAN_POINT ( 'NONE',  ( 771.1735550268778070, -393.1800572038737300, 316.3353852180827630 ) ) ;
#9536 = CARTESIAN_POINT ( 'NONE',  ( 766.0291762391763086, -130.9181544815166660, 360.7704444035551319 ) ) ;
#9537 = CARTESIAN_POINT ( 'NONE',  ( 780.5290396650775619, -36.35105083532390324, -365.2837595273619513 ) ) ;
#9538 = CARTESIAN_POINT ( 'NONE',  ( 746.7653713866222915, -65.26014174441471027, 351.0478386215610271 ) ) ;
#9539 = CARTESIAN_POINT ( 'NONE',  ( 768.0187753319979720, -368.6346026584193964, 318.0580252608186242 ) ) ;
#9540 = DIRECTION ( 'NONE',  ( 0.000000000000000000, 0.000000000000000000, 1.000000000000000000 ) ) ;
#9541 = CARTESIAN_POINT ( 'NONE',  ( -728.8365100919714905, 260.0000000000001705, -199.9999999999890861 ) ) ;
#9542 = CARTESIAN_POINT ( 'NONE',  ( 805.9055244015594326, -147.6237781080508285, 315.8990559732753240 ) ) ;
#9543 = CARTESIAN_POINT ( 'NONE',  ( 797.8594530101008786, -445.5436935675098766, 322.1405469898980982 ) ) ;
#9544 = ORIENTED_EDGE ( 'NONE', *, *, #28972, .F. ) ;
#9545 = CARTESIAN_POINT ( 'NONE',  ( 778.2165204200184689, -70.81642084023850714, -364.9363028652563230 ) ) ;
#9546 = CARTESIAN_POINT ( 'NONE',  ( 796.7845633553578182, -369.6237781080500895, -358.5707757039688204 ) ) ;
#9548 = CARTESIAN_POINT ( 'NONE',  ( 785.3687786644885591, -203.3618753856926276, 315.3201227861280813 ) ) ;
#9547 = CARTESIAN_POINT ( 'NONE',  ( 801.9419747391806368, -186.4527844766017779, 351.9812246680014027 ) ) ;
#9549 = CARTESIAN_POINT ( 'NONE',  ( 748.3538107759620743, -352.7146871989593251, -355.8262568251490165 ) ) ;
#9550 = CARTESIAN_POINT ( 'NONE',  ( -786.4999999999993179, 26.27639943461401018, 900.0000000000001137 ) ) ;
#9551 = B_SPLINE_CURVE_WITH_KNOTS ( 'NONE', 3,
 ( #27068, #430, #40920, #17987, #2568, #9513, #23578, #16433, #2333, #30760, #6031, #34199 ),
 .UNSPECIFIED., .F., .F.,
 ( 4, 2, 2, 2, 2, 4 ),
 ( 0.2497888289850607457, 0.3123416217387972038, 0.3748944144925336897, 0.4374472072462701200, 0.4687236036231350322, 0.5000000000000000000 ),
 .UNSPECIFIED. ) ;
#9552 = ORIENTED_EDGE ( 'NONE', *, *, #13110, .F. ) ;
#9553 = CARTESIAN_POINT ( 'NONE',  ( 771.2633955100217236, -383.9073299311466485, 363.4237431249939618 ) ) ;
#9554 = VECTOR ( 'NONE', #3082, 1000.000000000000000 ) ;
#9555 = VERTEX_POINT ( 'NONE', #19060 ) ;
#9556 = CARTESIAN_POINT ( 'NONE',  ( 919.9999999999993179, 154.9999999999998863, 360.0000000000000000 ) ) ;
#9557 = CARTESIAN_POINT ( 'NONE',  ( 745.4481719005789273, -219.7255117493289447, -347.5162901302853129 ) ) ;
#9558 = CARTESIAN_POINT ( 'NONE',  ( 767.6429770376291799, -105.1800572038747390, 306.8695393053162093 ) ) ;
#9559 = ORIENTED_EDGE ( 'NONE', *, *, #36894, .T. ) ;
#9560 = CARTESIAN_POINT ( 'NONE',  ( 762.3223304703356007, -223.5436935675107577, -322.3223304703362828 ) ) ;
#9561 = ORIENTED_EDGE ( 'NONE', *, *, #7550, .T. ) ;
#9562 = CARTESIAN_POINT ( 'NONE',  ( 797.8594530101008786, -325.5436935675105019, -322.1405469898980982 ) ) ;
#9563 = CARTESIAN_POINT ( 'NONE',  ( 763.0428371773158460, -443.4636090269702322, -358.7617431975195359 ) ) ;
#9564 = CARTESIAN_POINT ( 'NONE',  ( 749.2812353651451076, -270.4527844766014937, 323.2262854647983090 ) ) ;
#9565 = CARTESIAN_POINT ( 'NONE',  ( 787.6308680596127942, -203.2601417444143124, 364.1105419155492768 ) ) ;
#9567 = DIRECTION ( 'NONE',  ( -0.000000000000000000, 1.000000000000000000, -0.000000000000000000 ) ) ;
#9566 = CARTESIAN_POINT ( 'NONE',  ( 701.1634899080286232, 259.9999999999999432, -202.7499999999988916 ) ) ;
#9568 = DIRECTION ( 'NONE',  ( -1.000000000000000000, 0.000000000000000000, 0.000000000000000000 ) ) ;
#9569 = ORIENTED_EDGE ( 'NONE', *, *, #43347, .F. ) ;
#9570 = CARTESIAN_POINT ( 'NONE',  ( 800.0135310231082713, 9.910851887033969021, -325.0180583372163028 ) ) ;
#9571 = DIRECTION ( 'NONE',  ( 0.000000000000000000, -1.000000000000000000, 0.000000000000000000 ) ) ;
#9572 = DIRECTION ( 'NONE',  ( 0.000000000000000000, 0.000000000000000000, 1.000000000000000000 ) ) ;
#9573 = EDGE_LOOP ( 'NONE', ( #41204, #29943, #39340, #4392 ) ) ;
#9574 = CARTESIAN_POINT ( 'NONE',  ( 752.7379699480933368, -228.0090635724254753, -361.9858362298580232 ) ) ;
#9575 = CARTESIAN_POINT ( 'NONE',  ( 745.5313806188320314, -111.2817908451530968, 333.7943932421247268 ) ) ;
#9577 = CARTESIAN_POINT ( 'NONE',  ( 771.1735550268778070, -225.1800572038743269, -316.3353852180827630 ) ) ;
#9576 = CYLINDRICAL_SURFACE ( 'NONE', #20916, 2.749999999999863665 ) ;
#9578 = CARTESIAN_POINT ( 'NONE',  ( 755.8398074228967971, -355.4419599262319593, -333.4516893846970333 ) ) ;
#9579 = CARTESIAN_POINT ( 'NONE',  ( 768.9521613784389729, -249.8272453906072315, -373.2346286133773106 ) ) ;
#9580 = FACE_OUTER_BOUND ( 'NONE', #12419, .T. ) ;
#9581 = DIRECTION ( 'NONE',  ( -0.000000000000000000, 1.000000000000000000, -0.000000000000000000 ) ) ;
#9582 = CARTESIAN_POINT ( 'NONE',  ( 776.9254006560222479, -68.19088175424413123, -314.8983024940802125 ) ) ;
#9583 = CARTESIAN_POINT ( 'NONE',  ( 758.4439275373578084, -444.5545181178792973, 353.2243759319684386 ) ) ;
#9584 = CARTESIAN_POINT ( 'NONE',  ( 810.4231160770870019, -360.5545181178796383, 321.9338519418446936 ) ) ;
#9585 = DIRECTION ( 'NONE',  ( -1.000000000000000000, -0.000000000000000000, -0.000000000000000000 ) ) ;
#9586 = CARTESIAN_POINT ( 'NONE',  ( 783.0433043558608688, -432.8965053807771142, -315.1538015810313027 ) ) ;
#9587 = CARTESIAN_POINT ( 'NONE',  ( 814.2001403089898304, -281.3618753856923718, -347.4397851343538264 ) ) ;
#9588 = CYLINDRICAL_SURFACE ( 'NONE', #27665, 6.118999999999985562 ) ;
#9589 = DIRECTION ( 'NONE',  ( -1.000000000000000000, -0.000000000000000000, -0.000000000000000000 ) ) ;
#9590 = CARTESIAN_POINT ( 'NONE',  ( 771.2633955100217236, -47.90732993114767169, -363.4237431249939618 ) ) ;
#9591 = CARTESIAN_POINT ( 'NONE',  ( 754.3581564841646241, -209.4636090269709996, 316.1443688327762516 ) ) ;
#9592 = CARTESIAN_POINT ( 'NONE',  ( 781.2497674668890113, -180.3510508353234343, -375.3608509340180603 ) ) ;
#9593 = CARTESIAN_POINT ( 'NONE',  ( 755.2512626584698410, -175.5436935675108998, 315.2512626584710915 ) ) ;
#9594 = CARTESIAN_POINT ( 'NONE',  ( 812.7932403749906598, -399.1800572038738437, -327.7687537140311633 ) ) ;
#9595 = CARTESIAN_POINT ( 'NONE',  ( 927.9999999999993179, 154.9999999999998863, 359.9749999999999659 ) ) ;
#9596 = CARTESIAN_POINT ( 'NONE',  ( 755.3201227861273992, -267.7255117493286320, 345.3687786644892981 ) ) ;
#9597 = CARTESIAN_POINT ( 'NONE',  ( 755.3028492785439312, -63.28179084515324604, 335.9200461376539693 ) ) ;
#9598 = CARTESIAN_POINT ( 'NONE',  ( 800.2193346964447755, -426.9982390220554862, -355.1360043628815788 ) ) ;
#9599 = LINE ( 'NONE', #7047, #26961 ) ;
#9600 = CARTESIAN_POINT ( 'NONE',  ( 187.1337867209877857, 62.85347435602256638, -357.4246812887967053 ) ) ;
#9602 = CARTESIAN_POINT ( 'NONE',  ( 785.3687786644884454, -323.3618753856923149, 315.3201227861279676 ) ) ;
#9601 = CARTESIAN_POINT ( 'NONE',  ( 805.1016975059191054, -78.89650538077832209, 343.0745993439771837 ) ) ;
#9603 = CARTESIAN_POINT ( 'NONE',  ( 786.6156483768007774, -265.4419599262323004, -315.5913626894246136 ) ) ;
#9604 = CARTESIAN_POINT ( 'NONE',  ( 781.8018195045266339, -46.27096629478404566, 365.1927285166406705 ) ) ;
#9605 = CARTESIAN_POINT ( 'NONE',  ( 793.4146539503750546, -265.9874144716867477, -307.6481478633938877 ) ) ;
#9606 = PLANE ( 'NONE',  #39375 ) ;
#9607 = CARTESIAN_POINT ( 'NONE',  ( 798.0661480581538854, -386.5328690171409676, 309.5768839229118043 ) ) ;
#9608 = ORIENTED_EDGE ( 'NONE', *, *, #45264, .T. ) ;
#9609 = CARTESIAN_POINT ( 'NONE',  ( 774.6312213355099630, -287.3618753856923718, 364.6798772138717482 ) ) ;
#9610 = CARTESIAN_POINT ( 'NONE',  ( 811.0346526505616112, 9.365397341579420498, 323.0537975583477532 ) ) ;
#9611 = CARTESIAN_POINT ( 'NONE',  ( 786.6156483768007774, -25.44195992623301450, -315.5913626894246136 ) ) ;
#9612 = CARTESIAN_POINT ( 'NONE',  ( 804.6798772138708955, -159.7255117493291436, -334.6312213355107019 ) ) ;
#9613 = CARTESIAN_POINT ( 'NONE',  ( 762.1405469898971887, -361.5436935675103882, 357.8594530101015607 ) ) ;
#9614 = CARTESIAN_POINT ( 'NONE',  ( 787.4397851343537695, -117.7255117493292715, -374.2001403089903988 ) ) ;
#9615 = CARTESIAN_POINT ( 'NONE',  ( 762.3223304703356007, -103.5436935675111272, -322.3223304703362828 ) ) ;
#9616 = EDGE_LOOP ( 'NONE', ( #32288, #12871 ) ) ;
#9617 = CARTESIAN_POINT ( 'NONE',  ( 804.4086373105744769, -49.64542720878965554, -333.3843516231986541 ) ) ;
#9618 = CARTESIAN_POINT ( 'NONE',  ( 787.5531968255692163, -357.8272453906068904, -316.1348686366205811 ) ) ;
#9620 = CARTESIAN_POINT ( 'NONE',  ( 773.4516893846965786, -403.6454272087884760, 315.8398074228977066 ) ) ;
#9619 = CARTESIAN_POINT ( 'NONE',  ( 768.0187753319979720, -104.6346026584202207, 318.0580252608186242 ) ) ;
#9621 = CARTESIAN_POINT ( 'NONE',  ( 757.2208543904082489, -88.71468719896009247, 350.9844846989624330 ) ) ;
#9624 = CARTESIAN_POINT ( 'NONE',  ( 766.5853460496234675, -349.9874144716865771, 372.3518521366060554 ) ) ;
#9623 = CARTESIAN_POINT ( 'NONE',  ( 441.1634899080286232, 259.9999999999999432, -199.9999999999972431 ) ) ;
#9622 = DIRECTION ( 'NONE',  ( -0.000000000000000000, -0.000000000000000000, 1.000000000000000000 ) ) ;
#9625 = CARTESIAN_POINT ( 'NONE',  ( 758.4439275373578084, -372.5545181178796383, -353.2243759319684386 ) ) ;
#9626 = CARTESIAN_POINT ( 'NONE',  ( 762.1405469898971887, -337.5436935675102177, -357.8594530101015607 ) ) ;
#9627 = CARTESIAN_POINT ( 'NONE',  ( 799.9636004259356241, -118.9181544815167229, -311.2241431872006956 ) ) ;
#9628 = CARTESIAN_POINT ( 'NONE',  ( 783.7953271457878373, -8.190881754244330182, 375.1787889125761239 ) ) ;
#9629 = CARTESIAN_POINT ( 'NONE',  ( 795.2725662613897839, 16.45630643248849267, 314.1785221222716586 ) ) ;
#9630 = CARTESIAN_POINT ( 'NONE',  ( 805.1016975059191054, -270.8965053807777394, -343.0745993439771837 ) ) ;
#9631 = CARTESIAN_POINT ( 'NONE',  ( 755.8990559732751535, -107.4636090269713122, -365.9055244015606831 ) ) ;
#9632 = DIRECTION ( 'NONE',  ( 1.000000000000000000, 0.000000000000000000, 0.000000000000000000 ) ) ;
#9633 = DIRECTION ( 'NONE',  ( 1.000000000000000000, 0.000000000000000000, 0.000000000000000000 ) ) ;
#9634 = CARTESIAN_POINT ( 'NONE',  ( 775.8780910478218402, -321.2817908451525000, 364.9511171171680530 ) ) ;
#9635 = VERTEX_POINT ( 'NONE', #37274 ) ;
#9636 = CARTESIAN_POINT ( 'NONE',  ( 757.7880784355613741, -306.0090635724252479, 312.4576283171834916 ) ) ;
#9637 = CARTESIAN_POINT ( 'NONE',  ( 787.4397851343537695, -165.7255117493291152, -374.2001403089903988 ) ) ;
#9638 = CARTESIAN_POINT ( 'NONE',  ( -769.9999999999992042, 205.0000000000000568, -319.9999999999999432 ) ) ;
#9639 = CARTESIAN_POINT ( 'NONE',  ( 746.4236121716829757, -111.8272453906076151, 328.8385539511384650 ) ) ;
#9640 = CARTESIAN_POINT ( 'NONE',  ( 814.2001403089898304, -305.3618753856922581, -347.4397851343538264 ) ) ;
#9641 = DIRECTION ( 'NONE',  ( 0.000000000000000000, -1.000000000000000000, 0.000000000000000000 ) ) ;
#9642 = CARTESIAN_POINT ( 'NONE',  ( 989.9999999999992042, 249.9999999999998863, -360.0000000000000000 ) ) ;
#9643 = CARTESIAN_POINT ( 'NONE',  ( 767.8955696845333705, -144.4527844766018632, 362.1676090361162323 ) ) ;
#9644 = VERTEX_POINT ( 'NONE', #23407 ) ;
#9645 = CARTESIAN_POINT ( 'NONE',  ( 814.8207195650702488, -434.1908817542430370, 336.2433038121456548 ) ) ;
#9646 = CARTESIAN_POINT ( 'NONE',  ( 815.0009284576459549, -390.3510508353227237, -338.7629533639073429 ) ) ;
#9647 = CARTESIAN_POINT ( 'NONE',  ( 744.7301800767019131, -124.8164208402383508, -337.4774526936615757 ) ) ;
#9648 = CARTESIAN_POINT ( 'NONE',  ( 784.1219089521767955, -45.28179084515329578, 315.0488828828318333 ) ) ;
#9649 = CARTESIAN_POINT ( 'NONE',  ( 792.2312462859673587, -371.9073299311465917, -307.2067596250082602 ) ) ;
#9650 = FACE_BOUND ( 'NONE', #11495, .T. ) ;
#9651 = CARTESIAN_POINT ( 'NONE',  ( 799.4546378042377910, -441.0783235625953580, 356.1575198192848006 ) ) ;
#9652 = ORIENTED_EDGE ( 'NONE', *, *, #11738, .T. ) ;
#9653 = CARTESIAN_POINT ( 'NONE',  ( 759.9864689768902508, -266.0891481129651197, 354.9819416627836404 ) ) ;
#9654 = EDGE_CURVE ( 'NONE', #15578, #27431, #7083, .T. ) ;
#9655 = CARTESIAN_POINT ( 'NONE',  ( 756.1443688327750579, -141.6237781080508569, -314.3581564841659315 ) ) ;
#9656 = LINE ( 'NONE', #23719, #28482 ) ;
#9657 = CARTESIAN_POINT ( 'NONE',  ( 756.1443688327750579, -285.6237781080502600, 314.3581564841659315 ) ) ;
#9658 = CARTESIAN_POINT ( 'NONE',  ( 755.3201227861273992, -99.72551174932931417, 345.3687786644892981 ) ) ;
#9659 = EDGE_LOOP ( 'NONE', ( #4738, #36761, #26527, #41847 ) ) ;
#9660 = CARTESIAN_POINT ( 'NONE',  ( 792.1044303154645831, -276.4527844766013800, 317.8323909638837677 ) ) ;
#9661 = CARTESIAN_POINT ( 'NONE',  ( 792.3570229623688874, -21.18005720387502677, -373.1304606946836202 ) ) ;
#9662 = DIRECTION ( 'NONE',  ( 0.000000000000000000, 0.000000000000000000, -1.000000000000000000 ) ) ;
#9663 = ORIENTED_EDGE ( 'NONE', *, *, #1807, .F. ) ;
#9664 = ORIENTED_EDGE ( 'NONE', *, *, #28357, .T. ) ;
#9665 = CARTESIAN_POINT ( 'NONE',  ( 752.7379699480933368, -396.0090635724249637, -361.9858362298580232 ) ) ;
#9666 = CARTESIAN_POINT ( 'NONE',  ( 794.9819416627830151, -276.9982390220559978, -319.9864689768909898 ) ) ;
#9668 = CARTESIAN_POINT ( 'NONE',  ( 744.8212110874229666, -258.8965053807777963, 336.2046728542121627 ) ) ;
#9667 = CARTESIAN_POINT ( 'NONE',  ( 800.9747183278959710, -348.9982390220558273, 311.9810565676471583 ) ) ;
#9669 = EDGE_CURVE ( 'NONE', #11791, #10012, #33638, .T. ) ;
#9670 = CARTESIAN_POINT ( 'NONE',  ( 802.9823548866075953, -265.0999726633344267, -330.0799878456151077 ) ) ;
#9671 = CARTESIAN_POINT ( 'NONE',  ( 778.2165204200184689, -214.8164208402380666, -364.9363028652563230 ) ) ;
#9672 = CARTESIAN_POINT ( 'NONE',  ( 804.4286716492782716, -425.3618753856919170, -345.3141322388244703 ) ) ;
#9673 = CARTESIAN_POINT ( 'NONE',  ( 781.8018195045266339, -262.2709662947831930, 365.1927285166406705 ) ) ;
#9674 = EDGE_LOOP ( 'NONE', ( #7421, #36199, #42960, #15361 ) ) ;
#9675 = CARTESIAN_POINT ( 'NONE',  ( 758.8095938919642549, -344.0891481129647786, 311.6929314249763365 ) ) ;
#9676 = CARTESIAN_POINT ( 'NONE',  ( 791.7608162188021197, 178.9475563372491251, 360.0000000000000000 ) ) ;
#9677 = CARTESIAN_POINT ( 'NONE',  ( 790.2803779376845341, 16.45630643248849623, 314.3272116953297086 ) ) ;
#9678 = DIRECTION ( 'NONE',  ( -0.000000000000000000, 1.000000000000000000, -0.000000000000000000 ) ) ;
#9679 = EDGE_CURVE ( 'NONE', #26697, #9876, #40318, .T. ) ;
#9680 = CARTESIAN_POINT ( 'NONE',  ( 801.5560724626406000, -240.5545181178798941, 326.7756240680316182 ) ) ;
#9681 = CARTESIAN_POINT ( 'NONE',  ( 756.3353852180819104, -77.90732993114757221, 331.1735550268788302 ) ) ;
#9682 = ORIENTED_EDGE ( 'NONE', *, *, #30903, .F. ) ;
#9683 = CARTESIAN_POINT ( 'NONE',  ( 754.3581564841646241, -449.4636090269702322, -316.1443688327762516 ) ) ;
#9684 = CARTESIAN_POINT ( 'NONE',  ( 755.2512626584698410, -79.54369356751119824, -315.2512626584710915 ) ) ;
#9685 = CARTESIAN_POINT ( 'NONE',  ( 766.7756240680305382, -254.5328690171413655, 361.5560724626415663 ) ) ;
#9686 = CARTESIAN_POINT ( 'NONE',  ( 765.0180583372156207, -432.9982390220555999, -360.0135310231089534 ) ) ;
#9687 = CARTESIAN_POINT ( 'NONE',  ( 778.2165204200184689, -46.81642084023858530, -364.9363028652563230 ) ) ;
#9688 = CARTESIAN_POINT ( 'NONE',  ( 799.9636004259356241, -22.91815448151701062, 311.2241431872006956 ) ) ;
#9689 = FACE_OUTER_BOUND ( 'NONE', #2379, .T. ) ;
#9690 = CARTESIAN_POINT ( 'NONE',  ( 766.0291762391763086, -274.9181544815161828, -360.7704444035551319 ) ) ;
#9691 = CARTESIAN_POINT ( 'NONE',  ( 792.2312462859673587, -203.9073299311471885, -307.2067596250082602 ) ) ;
#9692 = CARTESIAN_POINT ( 'NONE',  ( 744.7301800767019131, -100.8164208402383792, 337.4774526936615757 ) ) ;
#9693 = CARTESIAN_POINT ( 'NONE',  ( 777.4774526936600978, -130.2709662947837899, 304.7301800767027657 ) ) ;
#9694 = DIRECTION ( 'NONE',  ( 1.000000000000000000, 0.000000000000000000, 0.000000000000000000 ) ) ;
#9695 = DIRECTION ( 'NONE',  ( 1.000000000000000000, 0.000000000000000000, -0.000000000000000000 ) ) ;
#9696 = CARTESIAN_POINT ( 'NONE',  ( 778.7502325331095108, -288.3510508353231216, -304.6391490659818828 ) ) ;
#9697 = CARTESIAN_POINT ( 'NONE',  ( 754.3581564841646241, -401.4636090269704027, 316.1443688327762516 ) ) ;
#9698 = ADVANCED_FACE ( 'NONE', ( #44209 ), #26644, .F. ) ;
#9699 = CARTESIAN_POINT ( 'NONE',  ( 812.7932403749906598, -279.1800572038741848, -327.7687537140311633 ) ) ;
#9700 = CARTESIAN_POINT ( 'NONE',  ( -190.7583438952258916, 294.6698570112193920, -244.9999999999999716 ) ) ;
#9701 = CARTESIAN_POINT ( 'NONE',  ( 767.7687537140311633, -383.9073299311466485, 372.7932403749916830 ) ) ;
#9702 = CARTESIAN_POINT ( 'NONE',  ( 792.3570229623691148, 2.819942796124898621, 373.1304606946836770 ) ) ;
#9703 = CARTESIAN_POINT ( 'NONE',  ( 755.0636971347428243, -340.2709662947831362, -341.7834795799807353 ) ) ;
#9704 = CARTESIAN_POINT ( 'NONE',  ( 784.0799538623451781, -11.80559628986942577, 364.6971507214555572 ) ) ;
#9705 = EDGE_CURVE ( 'NONE', #14504, #24267, #32164, .T. ) ;
#9706 = CARTESIAN_POINT ( 'NONE',  ( 791.1614460488616487, -35.26014174441480264, -373.5763878283158874 ) ) ;
#9707 = CARTESIAN_POINT ( 'NONE',  ( 803.8651313633788504, -149.2601417444144261, -332.4468031744301015 ) ) ;
#9708 = CARTESIAN_POINT ( 'NONE',  ( 776.2433038121456548, -180.8965053807779952, 374.8207195650711014 ) ) ;
#9709 = CARTESIAN_POINT ( 'NONE',  ( 788.8264449731201466, 2.819942796124898621, 363.6646147819170665 ) ) ;
#9710 = ORIENTED_EDGE ( 'NONE', *, *, #9416, .T. ) ;
#9711 = CARTESIAN_POINT ( 'NONE',  ( 774.6312213355099630, -71.36187538569302546, -364.6798772138717482 ) ) ;
#9712 = CARTESIAN_POINT ( 'NONE',  ( 804.9511171171677688, -173.8055962898689302, -335.8780910478229202 ) ) ;
#9713 = CARTESIAN_POINT ( 'NONE',  ( 792.1044303154645831, -156.4527844766018916, 317.8323909638837677 ) ) ;
#9714 = CARTESIAN_POINT ( 'NONE',  ( 811.6461892240364477, -4.714687198960358039, -324.1737431748509835 ) ) ;
#9715 = CARTESIAN_POINT ( 'NONE',  ( 785.3141322388236176, -309.7255117493287457, 364.4286716492789537 ) ) ;
#9716 = VECTOR ( 'NONE', #22908, 1000.000000000000000 ) ;
#9717 = DIRECTION ( 'NONE',  ( 0.000000000000000000, -0.7517448203044211352, 0.6594541114781782287 ) ) ;
#9718 = ORIENTED_EDGE ( 'NONE', *, *, #27310, .F. ) ;
#9719 = CARTESIAN_POINT ( 'NONE',  ( 772.3691319403857278, 0.7398582555850804487, 315.8894580844506663 ) ) ;
#9720 = CARTESIAN_POINT ( 'NONE',  ( 813.5763878283155464, -315.8272453906070609, -351.1614460488615350 ) ) ;
#9721 = ADVANCED_FACE ( 'NONE', ( #12569 ), #12785, .F. ) ;
#9722 = SHAPE_DEFINITION_REPRESENTATION ( #12958, #26911 ) ;
#9723 = CARTESIAN_POINT ( 'NONE',  ( 792.2312462859673587, -227.9073299311471033, 307.2067596250082602 ) ) ;
#9724 = ADVANCED_FACE ( 'NONE', ( #22945 ), #2169, .F. ) ;
#9725 = CARTESIAN_POINT ( 'NONE',  ( 790.0220218866281812, -319.0999726633342561, 363.2186876482849129 ) ) ;
#9726 = CARTESIAN_POINT ( 'NONE',  ( 754.8983024940795303, -426.8965053807771142, 336.9254006560228163 ) ) ;
#9727 = CARTESIAN_POINT ( 'NONE',  ( 804.6971507214547046, -123.2817908451530542, -344.0799538623459739 ) ) ;
#9728 = CARTESIAN_POINT ( 'NONE',  ( 758.0580252608178853, -102.4527844766020337, -328.0187753319985404 ) ) ;
#9729 = CARTESIAN_POINT ( 'NONE',  ( 762.1405469898973024, -313.5436935675103882, -357.8594530101016176 ) ) ;
#9730 = CARTESIAN_POINT ( 'NONE',  ( 797.8594530101008786, -445.5436935675098766, -322.1405469898980982 ) ) ;
#9731 = CARTESIAN_POINT ( 'NONE',  ( 775.9200461376533440, -287.8055962898685038, 315.3028492785443291 ) ) ;
#9732 = CARTESIAN_POINT ( 'NONE',  ( 911.9999999999993179, 219.9999999999998863, 360.0000000000000000 ) ) ;
#9733 = CARTESIAN_POINT ( 'NONE',  ( 792.0613484971601110, -458.0032201311295807, -367.4685979341032294 ) ) ;
#9734 = ADVANCED_FACE ( 'NONE', ( #40740 ), #28470, .F. ) ;
#9735 = CARTESIAN_POINT ( 'NONE',  ( 802.5472867521000353, -124.3726999360621619, 350.8726784830461156 ) ) ;
#9736 = DIRECTION ( 'NONE',  ( 0.000000000000000000, 0.000000000000000000, 1.000000000000000000 ) ) ;
#9737 = EDGE_LOOP ( 'NONE', ( #28668, #31558 ) ) ;
#9738 = CARTESIAN_POINT ( 'NONE',  ( 754.3581564841646241, -329.4636090269706870, -316.1443688327762516 ) ) ;
#9739 = CARTESIAN_POINT ( 'NONE',  ( 778.7629533639073998, -200.7363362996982801, 375.0009284576466371 ) ) ;
#9740 = CARTESIAN_POINT ( 'NONE',  ( 800.0135310231082713, -326.0891481129649492, -325.0180583372163028 ) ) ;
#9741 = CARTESIAN_POINT ( 'NONE',  ( -26.63011601220122060, -544.8427095258973623, -369.9999999999999432 ) ) ;
#9742 = CARTESIAN_POINT ( 'NONE',  ( 784.1219089521767955, -189.2817908451528979, -315.0488828828318333 ) ) ;
#9743 = CARTESIAN_POINT ( 'NONE',  ( 796.9462024416508257, -60.45278447660215448, 308.9653473494370246 ) ) ;
#9744 = AXIS2_PLACEMENT_3D ( 'NONE', #29466, #36167, #11233 ) ;
#9745 = CARTESIAN_POINT ( 'NONE',  ( 773.4999999999993179, -513.1383975375929367, -369.9999999999999432 ) ) ;
#9746 = CARTESIAN_POINT ( 'NONE',  ( 749.2812353651451076, -366.4527844766012095, -323.2262854647983090 ) ) ;
#9747 = CARTESIAN_POINT ( 'NONE',  ( 989.9999999999992042, 249.9999999999998863, -360.0000000000000000 ) ) ;
#9748 = EDGE_CURVE ( 'NONE', #9048, #42700, #35118, .T. ) ;
#9749 = CARTESIAN_POINT ( 'NONE',  ( 791.0478386215596629, -309.8272453906070041, 306.7653713866226326 ) ) ;
#9750 = EDGE_CURVE ( 'NONE', #18427, #12174, #22503, .T. ) ;
#9751 = LINE ( 'NONE', #29692, #12450 ) ;
#9752 = CARTESIAN_POINT ( 'NONE',  ( 814.9108240113580450, -304.2709662947832499, 337.5031285880265273 ) ) ;
#9753 = CARTESIAN_POINT ( 'NONE',  ( 792.3570229623688874, -21.18005720387502677, -373.1304606946836202 ) ) ;
#9754 = CARTESIAN_POINT ( 'NONE',  ( 771.2633955100217236, -239.9073299311470748, -363.4237431249939618 ) ) ;
#9755 = CARTESIAN_POINT ( 'NONE',  ( -468.8365100919714337, 260.0000000000001705, -202.7499999999907345 ) ) ;
#9756 = CARTESIAN_POINT ( 'NONE',  ( 795.1360043628807261, -404.0891481129646081, 360.2193346964456282 ) ) ;
#9757 = CARTESIAN_POINT ( 'NONE',  ( 799.2566176426618085, -144.0090635724257027, 324.0069404352559559 ) ) ;
#9758 = CARTESIAN_POINT ( 'NONE',  ( 790.8726784830453198, -34.71468719896025590, -362.5472867521010585 ) ) ;
#9759 = CARTESIAN_POINT ( 'NONE',  ( 795.6651683502461765, -58.71468719896019905, 371.3240766477733814 ) ) ;
#9760 = CARTESIAN_POINT ( 'NONE',  ( 756.3353852180820240, -365.9073299311466485, 331.1735550268787733 ) ) ;
#9761 = CARTESIAN_POINT ( 'NONE',  ( 767.6429770376291799, 14.81994279612486309, 306.8695393053162093 ) ) ;
#9762 = CARTESIAN_POINT ( 'NONE',  ( 802.1676090361156639, -446.6346026584189985, 327.8955696845344505 ) ) ;
#9763 = VERTEX_POINT ( 'NONE', #26204 ) ;
#9764 = CARTESIAN_POINT ( 'NONE',  ( 757.8323909638827445, -74.63460265842032015, -352.1044303154654358 ) ) ;
#9765 = CARTESIAN_POINT ( 'NONE',  ( 804.1601925771018387, -367.4419599262319025, -346.5483106153029098 ) ) ;
#9767 = CARTESIAN_POINT ( 'NONE',  ( 792.1044303154646968, -180.4527844766017495, 317.8323909638837677 ) ) ;
#9766 = CARTESIAN_POINT ( 'NONE',  ( 797.8594530101008786, -205.5436935675108430, 322.1405469898980982 ) ) ;
#9768 = VECTOR ( 'NONE', #45196, 1000.000000000000000 ) ;
#9769 = CARTESIAN_POINT ( 'NONE',  ( 759.8311093483677041, -358.1692326535047641, -310.9282345327691814 ) ) ;
#9770 = CARTESIAN_POINT ( 'NONE',  ( 180.7583438952258348, 394.6698570112193920, -274.9999999999999432 ) ) ;
#9771 = VERTEX_POINT ( 'NONE', #30122 ) ;
#9772 = EDGE_CURVE ( 'NONE', #16409, #30556, #19267, .T. ) ;
#9773 = ORIENTED_EDGE ( 'NONE', *, *, #5829, .F. ) ;
#9774 = CARTESIAN_POINT ( 'NONE',  ( 777.4774526936600978, -202.2709662947834772, -304.7301800767027657 ) ) ;
#9775 = CARTESIAN_POINT ( 'NONE',  ( 763.0537975583476964, -120.4527844766019768, 371.0346526505628617 ) ) ;
#9776 = ADVANCED_FACE ( 'NONE', ( #9096 ), #1698, .F. ) ;
#9777 = ORIENTED_EDGE ( 'NONE', *, *, #39309, .F. ) ;
#9778=STYLED_ITEM('',(#45751),#16696);
#9779 = CARTESIAN_POINT ( 'NONE',  ( 771.1735550268780344, -201.1800572038744690, -316.3353852180828198 ) ) ;
#9780 = EDGE_LOOP ( 'NONE', ( #37451, #20911, #29168, #1816 ) ) ;
#9781 = CARTESIAN_POINT ( 'NONE',  ( 803.4237431249931660, -327.1800572038741279, -331.2633955100225194 ) ) ;
#9782 = CARTESIAN_POINT ( 'NONE',  ( 773.4516893846965786, -451.6454272087884192, -315.8398074228977066 ) ) ;
#9783 = CARTESIAN_POINT ( 'NONE',  ( 796.7845633553578182, -201.6237781080506863, 358.5707757039688204 ) ) ;
#9784 = EDGE_CURVE ( 'NONE', #39697, #36781, #33816, .T. ) ;
#9786 = CARTESIAN_POINT ( 'NONE',  ( 989.9999999999992042, 50.81038600091411439, -217.3872392842761769 ) ) ;
#9785 = DIRECTION ( 'NONE',  ( 0.000000000000000000, 0.000000000000000000, 1.000000000000000000 ) ) ;
#9787 = FACE_OUTER_BOUND ( 'NONE', #5065, .T. ) ;
#9788 = ORIENTED_EDGE ( 'NONE', *, *, #41294, .T. ) ;
#9789 = CARTESIAN_POINT ( 'NONE',  ( 769.9779781133707957, -451.0999726633339151, -316.7813123517150871 ) ) ;
#9790 = CARTESIAN_POINT ( 'NONE',  ( 759.2380499001254748, 21.41625977839825978, -318.3449445151863415 ) ) ;
#9791 = CARTESIAN_POINT ( 'NONE',  ( 939.9999999999992042, 62.85347435602262323, -357.4246812887967621 ) ) ;
#9792 = CARTESIAN_POINT ( 'NONE',  ( 809.0717654672305343, -244.9181544815162681, -360.1688906516309885 ) ) ;
#9793 = CARTESIAN_POINT ( 'NONE',  ( 750.9282345327678740, -88.91815448151682233, 319.8311093483690115 ) ) ;
#9795 = CARTESIAN_POINT ( 'NONE',  ( 756.3353852180819104, -221.9073299311470464, -331.1735550268788302 ) ) ;
#9794 = CARTESIAN_POINT ( 'NONE',  ( 701.1634899080286232, 259.9999999999999432, -199.9999999999990337 ) ) ;
#9796 = CARTESIAN_POINT ( 'NONE',  ( 773.3843516231979720, -373.4419599262319593, -364.4086373105754433 ) ) ;
#9797 = CARTESIAN_POINT ( 'NONE',  ( 745.1792804349281596, -254.1908817542435770, -343.7566961878542884 ) ) ;
#9798 = DIRECTION ( 'NONE',  ( 0.000000000000000000, 0.7071067811865578978, 0.7071067811865372477 ) ) ;
#9799 = LINE ( 'NONE', #16053, #25297 ) ;
#9800 = CARTESIAN_POINT ( 'NONE',  ( 772.4468031744293057, -81.82724539060772884, -363.8651313633793620 ) ) ;
#9801 = CARTESIAN_POINT ( 'NONE',  ( 759.0159684113467620, -448.9181544815156144, 325.8855110935213020 ) ) ;
#9802 = AXIS2_PLACEMENT_3D ( 'NONE', #40544, #19503, #33600 ) ;
#9803 = FACE_BOUND ( 'NONE', #27502, .T. ) ;
#9804 = CARTESIAN_POINT ( 'NONE',  ( 796.7845633553578182, -417.6237781080499190, -358.5707757039688204 ) ) ;
#9805 = CARTESIAN_POINT ( 'NONE',  ( 763.0537975583476964, -288.4527844766014937, -371.0346526505628617 ) ) ;
#9806 = CARTESIAN_POINT ( 'NONE',  ( 939.9999999999993179, -600.0000000000001137, 360.0000000000000000 ) ) ;
#9807 = CARTESIAN_POINT ( 'NONE',  ( -26.63011601220122060, -513.1383975375929367, -349.9999999999999432 ) ) ;
#9808 = CARTESIAN_POINT ( 'NONE',  ( 802.1676090361156639, -62.63460265842031305, -327.8955696845344505 ) ) ;
#9809 =( GEOMETRIC_REPRESENTATION_CONTEXT ( 3 ) GLOBAL_UNCERTAINTY_ASSIGNED_CONTEXT ( ( #19472 ) ) GLOBAL_UNIT_ASSIGNED_CONTEXT ( ( #1202, #4896, #35616 ) ) REPRESENTATION_CONTEXT ( 'NONE', 'WORKASPACE' ) );
#9810 = CARTESIAN_POINT ( 'NONE',  ( 748.6759233522253680, -208.3726999360619061, 324.3348316497537098 ) ) ;
#9811 = CARTESIAN_POINT ( 'NONE',  ( 766.5853460496234675, -157.9874144716871456, -372.3518521366060554 ) ) ;
#9812 = CARTESIAN_POINT ( 'NONE',  ( 745.0891759886404770, -196.2709662947835909, 342.4968714119734159 ) ) ;
#9813 = CARTESIAN_POINT ( 'NONE',  ( 814.9108240113580450, -400.2709662947828519, -337.5031285880265273 ) ) ;
#9814 = FACE_OUTER_BOUND ( 'NONE', #14920, .T. ) ;
#9815 = CARTESIAN_POINT ( 'NONE',  ( 758.0580252608178853, -294.4527844766013800, 328.0187753319985404 ) ) ;
#9816 = CARTESIAN_POINT ( 'NONE',  ( 804.8461984189677878, -74.19088175424410281, 336.9566956441385628 ) ) ;
#9817 = CARTESIAN_POINT ( 'NONE',  ( 765.0180583372156207, -432.9982390220555999, -360.0135310231089534 ) ) ;
#9818 = CARTESIAN_POINT ( 'NONE',  ( -809.9999999999993179, -512.9681489794448908, -339.9999999999999432 ) ) ;
#9819 = DIRECTION ( 'NONE',  ( -0.000000000000000000, -1.000000000000000000, 0.000000000000000000 ) ) ;
#9821 = CARTESIAN_POINT ( 'NONE',  ( 801.9419747391806368, -330.4527844766013231, 351.9812246680014027 ) ) ;
#9820 = CARTESIAN_POINT ( 'NONE',  ( 761.2382568024794409, -111.6237781080509279, 356.9571628226838129 ) ) ;
#9822 = EDGE_LOOP ( 'NONE', ( #5137, #2321, #44202, #36220 ) ) ;
#9823 = CARTESIAN_POINT ( 'NONE',  ( 801.3366627262608972, -272.5328690171413086, -353.0897708529566899 ) ) ;
#9824 = CARTESIAN_POINT ( 'NONE',  ( 794.9819416627830151, -132.9982390220564810, -319.9864689768909898 ) ) ;
#9825 = CARTESIAN_POINT ( 'NONE',  ( 767.8955696845333705, -96.45278447660203369, 362.1676090361162323 ) ) ;
#9826 = CARTESIAN_POINT ( 'NONE',  ( 815.1787889125755555, -270.8965053807777394, -343.7953271457877804 ) ) ;
#9827 = CARTESIAN_POINT ( 'NONE',  ( 794.9999999999993179, -365.3551492539851893, 1.867567485292990437 ) ) ;
#9828 = CARTESIAN_POINT ( 'NONE',  ( 791.1614460488616487, -395.2601417444136587, 373.5763878283158874 ) ) ;
#9829 = ORIENTED_EDGE ( 'NONE', *, *, #28866, .F. ) ;
#9830 = CARTESIAN_POINT ( 'NONE',  ( 785.3141322388236176, -285.7255117493286889, 364.4286716492789537 ) ) ;
#9831 = PRODUCT_DEFINITION ( 'UNKNOWN', '', #19396, #15787 ) ;
#9832 = CARTESIAN_POINT ( 'NONE',  ( 775.9200461376533440, -47.80559628986931386, -315.3028492785443291 ) ) ;
#9833 = CARTESIAN_POINT ( 'NONE',  ( 800.2193346964447755, -162.9982390220563673, -355.1360043628815788 ) ) ;
#9834 = CARTESIAN_POINT ( 'NONE',  ( 778.1981804954714335, -370.2709662947831362, 314.8072714833589885 ) ) ;
#9835 = CARTESIAN_POINT ( 'NONE',  ( 748.9653473494363425, -98.63460265842024910, -356.9462024416521331 ) ) ;
#9836 = AXIS2_PLACEMENT_3D ( 'NONE', #21729, #45612, #39774 ) ;
#9837 = CARTESIAN_POINT ( 'NONE',  ( 778.2165204200184689, -94.81642084023843609, -364.9363028652563230 ) ) ;
#9838 = ORIENTED_EDGE ( 'NONE', *, *, #39646, .T. ) ;
#9839 = CARTESIAN_POINT ( 'NONE',  ( 805.2837595273609850, -50.73633629969874193, -340.5290396650784714 ) ) ;
#9840 = AXIS2_PLACEMENT_3D ( 'NONE', #20974, #3444, #14537 ) ;
#9841 = CARTESIAN_POINT ( 'NONE',  ( 793.9708237608222134, -358.9181544815160123, -319.2295555964448681 ) ) ;
#9842 = CARTESIAN_POINT ( 'NONE',  ( 757.4527132478984868, -400.3726999360612808, 329.1273215169538844 ) ) ;
#9845 = CARTESIAN_POINT ( 'NONE',  ( 748.3538107759620743, -352.7146871989593251, 355.8262568251490165 ) ) ;
#9844 = DIRECTION ( 'NONE',  ( 0.000000000000000000, 0.000000000000000000, 1.000000000000000000 ) ) ;
#9843 = CARTESIAN_POINT ( 'NONE',  ( 801.1904061080338124, -452.0891481129646081, 368.3070685750236066 ) ) ;
#9846 = CARTESIAN_POINT ( 'NONE',  ( 796.1575198192839480, -342.0090635724251342, -359.4546378042384163 ) ) ;
#9847 = CARTESIAN_POINT ( 'NONE',  ( 757.8323909638827445, -362.6346026584194533, -352.1044303154654358 ) ) ;
#9848 = CARTESIAN_POINT ( 'NONE',  ( 805.6418435158337843, -5.463609026971610660, 363.8556311672236916 ) ) ;
#9849 = AXIS2_PLACEMENT_3D ( 'NONE', #20719, #7343, #21420 ) ;
#9851 = DIRECTION ( 'NONE',  ( -1.000000000000000000, -0.000000000000000000, 0.000000000000000000 ) ) ;
#9850 = DIRECTION ( 'NONE',  ( 1.000000000000000000, 0.000000000000000000, -0.000000000000000000 ) ) ;
#9852 = CARTESIAN_POINT ( 'NONE',  ( 755.8398074228967971, -259.4419599262322436, -333.4516893846970333 ) ) ;
#9853 = CARTESIAN_POINT ( 'NONE',  ( 766.4474001241216001, -139.0999726633348530, -307.3154664389482491 ) ) ;
#9854 = DIRECTION ( 'NONE',  ( -1.000000000000000000, -0.000000000000000000, 0.000000000000000000 ) ) ;
#9855 = DIRECTION ( 'NONE',  ( -1.000000000000000000, -0.000000000000000000, 0.000000000000000000 ) ) ;
#9856 = CARTESIAN_POINT ( 'NONE',  ( 757.0176451133909268, -325.0999726633342561, 349.9200121543848354 ) ) ;
#9857 = VERTEX_POINT ( 'NONE', #33586 ) ;
#9858 = CARTESIAN_POINT ( 'NONE',  ( 805.6418435158337843, -317.4636090269706301, 363.8556311672236916 ) ) ;
#9859 = CARTESIAN_POINT ( 'NONE',  ( 813.1304606946831655, -185.9073299311472169, -352.3570229623691716 ) ) ;
#9860 = LINE ( 'NONE', #31573, #14262 ) ;
#9861 = CARTESIAN_POINT ( 'NONE',  ( 764.1737431748507561, -106.3726999360621903, 371.6461892240376415 ) ) ;
#9862 = CARTESIAN_POINT ( 'NONE',  ( 801.1904061080336987, -308.0891481129650629, -368.3070685750235498 ) ) ;
#9863 = CARTESIAN_POINT ( 'NONE',  ( 794.9999999999993179, -365.3551492539851893, 18.13243251470705886 ) ) ;
#9864 = DIRECTION ( 'NONE',  ( -0.000000000000000000, -0.000000000000000000, -1.000000000000000000 ) ) ;
#9865 = CARTESIAN_POINT ( 'NONE',  ( 804.6798772138708955, -183.7255117493290015, 334.6312213355107019 ) ) ;
#9866 = AXIS2_PLACEMENT_3D ( 'NONE', #20927, #14026, #28095 ) ;
#9867 = EDGE_LOOP ( 'NONE', ( #18095, #26764, #8253, #12212, #34371, #25364 ) ) ;
#9868 = AXIS2_PLACEMENT_3D ( 'NONE', #999, #4263, #1231 ) ;
#9869 = CARTESIAN_POINT ( 'NONE',  ( 802.2119215644370342, -438.0090635724247932, 367.5423716828165084 ) ) ;
#9870 = CARTESIAN_POINT ( 'NONE',  ( 766.5853460496234675, -373.9874144716864066, -372.3518521366060554 ) ) ;
#9871 = CARTESIAN_POINT ( 'NONE',  ( 792.3570229623688874, -117.1800572038746964, -373.1304606946836202 ) ) ;
#9872 = CARTESIAN_POINT ( 'NONE',  ( 766.9102291470427417, -42.55451811788057626, 318.6633372737382501 ) ) ;
#9873 = CARTESIAN_POINT ( 'NONE',  ( 796.9462024416508257, -396.4527844766010389, -308.9653473494370246 ) ) ;
#9874 = DIRECTION ( 'NONE',  ( 4.625929269271485914E-16, -1.000000000000000000, 0.000000000000000000 ) ) ;
#9875 = CARTESIAN_POINT ( 'NONE',  ( 800.7704444035546203, -436.1692326535044231, 326.0291762391768771 ) ) ;
#9876 = VERTEX_POINT ( 'NONE', #1936 ) ;
#9877 = CARTESIAN_POINT ( 'NONE',  ( 771.2368401574024119, -157.4419599262326130, -374.2805881961240857 ) ) ;
#9878 = CARTESIAN_POINT ( 'NONE',  ( 999.9999999999992042, 478.9999999999999432, 200.9999999999999432 ) ) ;
#9879 = CARTESIAN_POINT ( 'NONE',  ( 773.7943932421234194, -263.8055962898686175, 305.5313806188329409 ) ) ;
#9880 = CARTESIAN_POINT ( 'NONE',  ( 785.3687786644885591, -131.3618753856928549, 315.3201227861280813 ) ) ;
#9881 = ORIENTED_EDGE ( 'NONE', *, *, #26982, .F. ) ;
#9882 = AXIS2_PLACEMENT_3D ( 'NONE', #85, #28246, #42345 ) ;
#9883 = CARTESIAN_POINT ( 'NONE',  ( 801.9419747391806368, -258.4527844766016074, 351.9812246680014027 ) ) ;
#9884 = CARTESIAN_POINT ( 'NONE',  ( 792.2312462859673587, -11.90732993114778182, -307.2067596250082602 ) ) ;
#9885 = DIRECTION ( 'NONE',  ( 0.000000000000000000, 0.000000000000000000, 1.000000000000000000 ) ) ;
#9886 = ORIENTED_EDGE ( 'NONE', *, *, #15887, .T. ) ;
#9887 = VERTEX_POINT ( 'NONE', #16039 ) ;
#9888 = CARTESIAN_POINT ( 'NONE',  ( 760.0363995740630116, -418.9181544815157849, -368.7758568127991907 ) ) ;
#9889 = CARTESIAN_POINT ( 'NONE',  ( 754.8072714833581358, -268.8164208402378108, -338.1981804954720587 ) ) ;
#9891 = CARTESIAN_POINT ( 'NONE',  ( 746.7653713866222915, -257.2601417444141134, 351.0478386215610271 ) ) ;
#9890 = CARTESIAN_POINT ( 'NONE',  ( 811.0346526505617248, -350.6346026584193396, 323.0537975583478101 ) ) ;
#9892 = CARTESIAN_POINT ( 'NONE',  ( 787.5531968255692163, -237.8272453906072599, -316.1348686366205811 ) ) ;
#9893 = CARTESIAN_POINT ( 'NONE',  ( 788.7366044899766848, -251.9073299311470748, -316.5762568750059813 ) ) ;
#9894 = AXIS2_PLACEMENT_3D ( 'NONE', #41455, #2882, #45382 ) ;
#9895 = CARTESIAN_POINT ( 'NONE',  ( 785.3141322388236176, -405.7255117493283478, -364.4286716492789537 ) ) ;
#9896 = CARTESIAN_POINT ( 'NONE',  ( 803.6646147819161570, -89.90732993114750116, -348.8264449731210561 ) ) ;
#9897 = CIRCLE ( 'NONE', #43884, 10.00000000000000888 ) ;
#9898 = CARTESIAN_POINT ( 'NONE',  ( 759.7806653035534055, -246.9982390220560546, 324.8639956371180801 ) ) ;
#9899 = ORIENTED_EDGE ( 'NONE', *, *, #22960, .F. ) ;
#9900 = CARTESIAN_POINT ( 'NONE',  ( 801.1904061080336987, -356.0891481129647218, 368.3070685750235498 ) ) ;
#9901 = LINE ( 'NONE', #13840, #19641 ) ;
#9902 = CARTESIAN_POINT ( 'NONE',  ( 762.1177392798416577, -66.55451811788050520, -309.8865473780659272 ) ) ;
#9903 = CARTESIAN_POINT ( 'NONE',  ( 774.9293440288117836, 16.45630643248849623, 314.9535949064562601 ) ) ;
#9904 = DIRECTION ( 'NONE',  ( -1.000000000000000000, -0.000000000000000000, -0.000000000000000000 ) ) ;
#9905 = CARTESIAN_POINT ( 'NONE',  ( 758.4439275373578084, -228.5545181178799794, 353.2243759319684386 ) ) ;
#9906 = CARTESIAN_POINT ( 'NONE',  ( 805.1927285166397041, -112.8164208402383508, 341.8018195045277707 ) ) ;
#9907 = EDGE_CURVE ( 'NONE', #11556, #1648, #3420, .T. ) ;
#9908 = ORIENTED_EDGE ( 'NONE', *, *, #16809, .F. ) ;
#9909 = CARTESIAN_POINT ( 'NONE',  ( 802.5472867521000353, -28.37269993606244967, -350.8726784830461156 ) ) ;
#9910 = CARTESIAN_POINT ( 'NONE',  ( 759.0252816721024374, -72.99823902205667991, -368.0189434323527280 ) ) ;
#9911 = CARTESIAN_POINT ( 'NONE',  ( 805.1016975059191054, -294.8965053807775689, 343.0745993439771837 ) ) ;
#9912 = CARTESIAN_POINT ( 'NONE',  ( 768.0187753319979720, -416.6346026584192259, -318.0580252608186242 ) ) ;
#9913 = CARTESIAN_POINT ( 'NONE',  ( 781.7834795799800531, -34.81642084023861372, -315.0636971347436202 ) ) ;
#9914 = AXIS2_PLACEMENT_3D ( 'NONE', #41533, #45224, #9662 ) ;
#9915 = CARTESIAN_POINT ( 'NONE',  ( 793.5525998758768083, -7.099972663335241130, 372.6845335610516941 ) ) ;
#9916 = CARTESIAN_POINT ( 'NONE',  ( 787.5162901302840055, -203.3618753856925991, -305.4481719005792684 ) ) ;
#9917 = CARTESIAN_POINT ( 'NONE',  ( 805.0032342141412300, -85.54369356751118403, 314.9967657858571783 ) ) ;
#9918 = CARTESIAN_POINT ( 'NONE',  ( 777.5031285880264704, -166.8164208402382087, 374.9108240113588408 ) ) ;
#9919 = CARTESIAN_POINT ( 'NONE',  ( 911.9999999999993179, 154.9999999999998863, -350.0000000000000000 ) ) ;
#9920 = CARTESIAN_POINT ( 'NONE',  ( 791.7608162188021197, 205.0000000000000568, 339.9999999999999432 ) ) ;
#9921 = CARTESIAN_POINT ( 'NONE',  ( 807.5423716828161105, -273.0783235625958696, -362.2119215644372048 ) ) ;
#9922 = CARTESIAN_POINT ( 'NONE',  ( 786.2694204179717872, -405.2817908451522158, 305.1769319972829067 ) ) ;
#9923 = CARTESIAN_POINT ( 'NONE',  ( 751.6929314249748586, -270.9982390220561115, -318.8095938919659034 ) ) ;
#9924 = CARTESIAN_POINT ( 'NONE',  ( -728.8365100919714905, 258.0940000000001646, -199.9999999999890861 ) ) ;
#9925 = CARTESIAN_POINT ( 'NONE',  ( 745.0891759886404770, -412.2709662947829088, 342.4968714119734159 ) ) ;
#9926 = CARTESIAN_POINT ( 'NONE',  ( 744.7301800767020268, -4.816420840238714085, 337.4774526936615189 ) ) ;
#9927 = CARTESIAN_POINT ( 'NONE',  ( 804.9363028652555840, -352.2709662947830225, -338.2165204200192079 ) ) ;
#9928 = VECTOR ( 'NONE', #19460, 1000.000000000000000 ) ;
#9929 = CARTESIAN_POINT ( 'NONE',  ( 756.1348686366196716, -17.26014174441486659, 347.5531968255698416 ) ) ;
#9930 = PRESENTATION_LAYER_ASSIGNMENT (  '', '', ( #11425 ) ) ;
#9931 = CARTESIAN_POINT ( 'NONE',  ( 801.9858362298568863, -51.07832356259657303, -312.7379699480935642 ) ) ;
#9932 = CARTESIAN_POINT ( 'NONE',  ( 760.5453621957607311, -141.0783235625962959, -323.8424801807151425 ) ) ;
#9933 = CARTESIAN_POINT ( 'NONE',  ( 783.7566961878529810, -168.8965053807780237, 305.1792804349288417 ) ) ;
#9934 = CARTESIAN_POINT ( 'NONE',  ( 787.4999999999992042, -512.9681489794448908, -309.9999999999998863 ) ) ;
#9935 = AXIS2_PLACEMENT_3D ( 'NONE', #40932, #30296, #23125 ) ;
#9936 = ORIENTED_EDGE ( 'NONE', *, *, #13763, .T. ) ;
#9937 = CARTESIAN_POINT ( 'NONE',  ( 757.8323909638827445, -50.63460265842036989, -352.1044303154654358 ) ) ;
#9938 = CARTESIAN_POINT ( 'NONE',  ( 764.0069404352550464, -159.0783235625962391, -359.2566176426627180 ) ) ;
#9939 = PRODUCT_DEFINITION_CONTEXT ( 'detailed design', #22838, 'design' ) ;
#9940 = CARTESIAN_POINT ( 'NONE',  ( 771.1735550268778070, -153.1800572038746395, 316.3353852180827630 ) ) ;
#9941 = EDGE_CURVE ( 'NONE', #23746, #577, #43528, .T. ) ;
#9942 = CARTESIAN_POINT ( 'NONE',  ( 783.7566961878529810, -0.8965053807785533513, -305.1792804349288417 ) ) ;
#9944 = CARTESIAN_POINT ( 'NONE',  ( 804.6798772138710092, -279.7255117493288026, 334.6312213355106451 ) ) ;
#9943 = CARTESIAN_POINT ( 'NONE',  ( 759.9864689768902508, -290.0891481129650629, 354.9819416627836404 ) ) ;
#9945 = CARTESIAN_POINT ( 'NONE',  ( 831.1634899080286232, 259.9999999999998863, -199.9999999999999432 ) ) ;
#9946 = EDGE_LOOP ( 'NONE', ( #14261, #4783 ) ) ;
#9947 = CARTESIAN_POINT ( 'NONE',  ( 798.7617431975189675, -3.623778108051270319, 323.0428371773161871 ) ) ;
#9948 = CARTESIAN_POINT ( 'NONE',  ( 795.8262568251477660, -310.3726999360616219, -308.3538107759623585 ) ) ;
#9949 = CIRCLE ( 'NONE', #15847, 19.99999999999998934 ) ;
#9950 = VECTOR ( 'NONE', #33385, 1000.000000000000000 ) ;
#9951 = CARTESIAN_POINT ( 'NONE',  ( 747.2067596250078623, -267.1800572038742985, 352.2312462859687230 ) ) ;
#9952 = CARTESIAN_POINT ( 'NONE',  ( 772.4468031744293057, -321.8272453906070609, 363.8651313633793620 ) ) ;
#9953 = CIRCLE ( 'NONE', #29152, 20.00000000000001776 ) ;
#9954 = CARTESIAN_POINT ( 'NONE',  ( 788.4001350590139054, -443.1233509495419298, 363.5803521658918385 ) ) ;
#9955 = CARTESIAN_POINT ( 'NONE',  ( 776.9254006560222479, -164.1908817542438612, -314.8983024940802125 ) ) ;
#9956 = CARTESIAN_POINT ( 'NONE',  ( 797.8594530101008786, -109.5436935675110988, -322.1405469898980982 ) ) ;
#9957 = CARTESIAN_POINT ( 'NONE',  ( 797.8594530101009923, -301.5436935675105588, -322.1405469898982119 ) ) ;
#9958 = EDGE_LOOP ( 'NONE', ( #15985, #30559, #20793, #31910 ) ) ;
#9959 = CARTESIAN_POINT ( 'NONE',  ( 758.6633372737375112, -284.5328690171412518, 326.9102291470432533 ) ) ;
#9960 = CARTESIAN_POINT ( 'NONE',  ( 769.9999999999992042, 178.9475563372491251, -360.0000000000000000 ) ) ;
#9961 = AXIS2_PLACEMENT_3D ( 'NONE', #24625, #6742, #3052 ) ;
#9962 = CARTESIAN_POINT ( 'NONE',  ( 763.0428371773158460, -131.4636090269711985, 358.7617431975195359 ) ) ;
#9963 = CARTESIAN_POINT ( 'NONE',  ( 758.0580252608178853, -30.45278447660226817, 328.0187753319985404 ) ) ;
#9964 = EDGE_CURVE ( 'NONE', #17907, #9771, #8434, .T. ) ;
#9965 = VERTEX_POINT ( 'NONE', #2389 ) ;
#9966 = CARTESIAN_POINT ( 'NONE',  ( 814.2805881961230625, -361.6454272087887603, -331.2368401574024119 ) ) ;
#9967 = PLANE ( 'NONE',  #11450 ) ;
#9968 = CARTESIAN_POINT ( 'NONE',  ( 747.6481478633932056, -229.0999726633345404, 353.4146539503763620 ) ) ;
#9969 = CARTESIAN_POINT ( 'NONE',  ( 754.9735926884551418, -186.3510508353234343, 340.5236548041000333 ) ) ;
#9970 = AXIS2_PLACEMENT_3D ( 'NONE', #44115, #44342, #12698 ) ;
#9971 = CARTESIAN_POINT ( 'NONE',  ( 757.8323909638827445, -338.6346026584195101, -352.1044303154654358 ) ) ;
#9972 = DIRECTION ( 'NONE',  ( -0.000000000000000000, 1.000000000000000000, -1.110223024625155554E-15 ) ) ;
#9973 = CARTESIAN_POINT ( 'NONE',  ( 793.9708237608222134, -190.9181544815164955, -319.2295555964448681 ) ) ;
#9974 = CARTESIAN_POINT ( 'NONE',  ( 807.9206849184947714, -452.9681489794447202, 338.7201299304387021 ) ) ;
#9975 = CARTESIAN_POINT ( 'NONE',  ( 758.8095938919644823, -392.0891481129647786, -311.6929314249762797 ) ) ;
#9976 = CARTESIAN_POINT ( 'NONE',  ( 799.9999999999993179, -365.3551492539851893, 18.13243251470705886 ) ) ;
#9977 = AXIS2_PLACEMENT_3D ( 'NONE', #28805, #8238, #7795 ) ;
#9978 = CARTESIAN_POINT ( 'NONE',  ( 745.5313806188320314, -303.2817908451525000, 333.7943932421247268 ) ) ;
#9979 = DIRECTION ( 'NONE',  ( 0.000000000000000000, 0.000000000000000000, -1.000000000000000000 ) ) ;
#9980 = CARTESIAN_POINT ( 'NONE',  ( 804.7487373415286811, -307.5436935675104451, 364.7487373415288516 ) ) ;
#9981 = CARTESIAN_POINT ( 'NONE',  ( 777.5031285880264704, -22.81642084023865280, -374.9108240113588408 ) ) ;
#9982 = CARTESIAN_POINT ( 'NONE',  ( 795.1360043628807261, -236.0891481129651766, -360.2193346964456282 ) ) ;
#9983 = AXIS2_PLACEMENT_3D ( 'NONE', #31009, #13464, #3289 ) ;
#9984 = EDGE_CURVE ( 'NONE', #39117, #22606, #37331, .T. ) ;
#9985 = LINE ( 'NONE', #45, #38003 ) ;
#9986 = CARTESIAN_POINT ( 'NONE',  ( 771.2633955100217236, -407.9073299311465348, 363.4237431249939618 ) ) ;
#9987 = CARTESIAN_POINT ( 'NONE',  ( 773.4516893846965786, -139.6454272087893571, 315.8398074228977066 ) ) ;
#9988 = CARTESIAN_POINT ( 'NONE',  ( 766.4474001241216001, -43.09997266333511590, -307.3154664389482491 ) ) ;
#9989 = CARTESIAN_POINT ( 'NONE',  ( 801.3366627262608972, -56.53286901714201917, -353.0897708529566899 ) ) ;
#9990 = CARTESIAN_POINT ( 'NONE',  ( 815.0009284576459549, -54.35105083532383219, 338.7629533639073429 ) ) ;
#9991 = CARTESIAN_POINT ( 'NONE',  ( 797.6776695296629214, -379.5436935675102745, 357.6776695296636603 ) ) ;
#9992 = DIRECTION ( 'NONE',  ( -1.000000000000000000, -0.000000000000000000, -0.000000000000000000 ) ) ;
#9993 =( NAMED_UNIT ( * ) SI_UNIT ( $, .STERADIAN. ) SOLID_ANGLE_UNIT ( ) );
#9994 = CARTESIAN_POINT ( 'NONE',  ( 785.3141322388236176, -429.7255117493282910, 364.4286716492789537 ) ) ;
#9995 = ORIENTED_EDGE ( 'NONE', *, *, #35112, .F. ) ;
#9996 = CARTESIAN_POINT ( 'NONE',  ( 805.1927285166397041, -64.81642084023852135, -341.8018195045277707 ) ) ;
#9997 = EDGE_CURVE ( 'NONE', #40519, #32688, #23852, .T. ) ;
#9998 = CARTESIAN_POINT ( 'NONE',  ( 754.8983024940795303, -378.8965053807772847, -336.9254006560228163 ) ) ;
#10000 = CARTESIAN_POINT ( 'NONE',  ( 781.8018195045267476, -190.2709662947835625, 365.1927285166407273 ) ) ;
#9999 = CARTESIAN_POINT ( 'NONE',  ( 771.2633955100217236, -191.9073299311471885, 363.4237431249939618 ) ) ;
#10001 = ORIENTED_EDGE ( 'NONE', *, *, #22731, .F. ) ;
#10002 = AXIS2_PLACEMENT_3D ( 'NONE', #30261, #33740, #37885 ) ;
#10003 = CARTESIAN_POINT ( 'NONE',  ( 813.2346286133761168, -365.2601417444137155, -328.9521613784389160 ) ) ;
#10004 = FACE_OUTER_BOUND ( 'NONE', #29565, .T. ) ;
#10005 = ORIENTED_EDGE ( 'NONE', *, *, #37944, .T. ) ;
#10006 = CARTESIAN_POINT ( 'NONE',  ( 771.2633955100217236, -407.9073299311465348, 363.4237431249939618 ) ) ;
#10007 = AXIS2_PLACEMENT_3D ( 'NONE', #9623, #23685, #37796 ) ;
#10008 = ORIENTED_EDGE ( 'NONE', *, *, #35689, .F. ) ;
#10009 = VECTOR ( 'NONE', #34332, 999.9999999999998863 ) ;
#10010 = CARTESIAN_POINT ( 'NONE',  ( 772.5602148656447525, -201.7255117493290015, -305.7998596910095443 ) ) ;
#10011 = CARTESIAN_POINT ( 'NONE',  ( 746.8695393053151292, -149.9073299311473875, 327.6429770376306578 ) ) ;
#10012 = VERTEX_POINT ( 'NONE', #17172 ) ;
#10013 = CARTESIAN_POINT ( 'NONE',  ( 800.2193346964446619, -210.9982390220562252, -355.1360043628816925 ) ) ;
#10014 = VERTEX_POINT ( 'NONE', #37968 ) ;
#10015 = EDGE_CURVE ( 'NONE', #31386, #15704, #13721, .T. ) ;
#10016 = CARTESIAN_POINT ( 'NONE',  ( 778.1981804954714335, -322.2709662947830225, -314.8072714833589885 ) ) ;
#10017 = CARTESIAN_POINT ( 'NONE',  ( 762.1405469898971887, -25.54369356751136877, -357.8594530101015607 ) ) ;
#10018 = VECTOR ( 'NONE', #26841, 1000.000000000000000 ) ;
#10019 = ADVANCED_FACE ( 'NONE', ( #24319 ), #27560, .T. ) ;
#10020 = CARTESIAN_POINT ( 'NONE',  ( 805.0264073115434940, -198.3510508353234059, 339.4763451958999099 ) ) ;
#10021 = CYLINDRICAL_SURFACE ( 'NONE', #5608, 6.118999999999985562 ) ;
#10022 = DIRECTION ( 'NONE',  ( 0.000000000000000000, 0.9235249282889856914, 0.3835384033298670503 ) ) ;
#10023 = AXIS2_PLACEMENT_3D ( 'NONE', #25756, #28294, #42853 ) ;
#10024 = ORIENTED_EDGE ( 'NONE', *, *, #30379, .F. ) ;
#10025 = CARTESIAN_POINT ( 'NONE',  ( 803.6646147819161570, 6.092670068852159559, -348.8264449731210561 ) ) ;
#10026 = CARTESIAN_POINT ( 'NONE',  ( 914.9999999999992042, 99.99999999999984368, 360.0000000000000000 ) ) ;
#10027 = DIRECTION ( 'NONE',  ( 0.000000000000000000, 0.7517448203044204691, -0.6594541114781790059 ) ) ;
#10028 = ADVANCED_FACE ( 'NONE', ( #6323 ), #10021, .F. ) ;
#10029 = ORIENTED_EDGE ( 'NONE', *, *, #40804, .F. ) ;
#10030 = CARTESIAN_POINT ( 'NONE',  ( 783.7953271457878373, -248.1908817542435202, -375.1787889125761239 ) ) ;
#10031 = CARTESIAN_POINT ( 'NONE',  ( 766.4474001241216001, -139.0999726633348530, 307.3154664389482491 ) ) ;
#10033 = CARTESIAN_POINT ( 'NONE',  ( 788.8264449731200330, -213.1800572038743553, -363.6646147819171233 ) ) ;
#10032 = PLANE ( 'NONE',  #12098 ) ;
#10034 = CARTESIAN_POINT ( 'NONE',  ( 799.4546378042377910, -393.0783235625954717, -356.1575198192848006 ) ) ;
#10035 = FACE_OUTER_BOUND ( 'NONE', #1241, .T. ) ;
#10036 = CARTESIAN_POINT ( 'NONE',  ( 800.0135310231082713, 9.910851887033969021, -325.0180583372163028 ) ) ;
#10037 = CARTESIAN_POINT ( 'NONE',  ( 784.1219089521767955, -93.28179084515315367, -315.0488828828318333 ) ) ;
#10038 = CARTESIAN_POINT ( 'NONE',  ( 778.7629533639073998, -368.7363362996977685, 375.0009284576466371 ) ) ;
#10039 = CARTESIAN_POINT ( 'NONE',  ( 998.9999999999992042, 479.9999999999998863, -199.9999999999999716 ) ) ;
#10040 = CARTESIAN_POINT ( 'NONE',  ( 749.8865473780648472, 3.467130982857797417, -322.1177392798429082 ) ) ;
#10041 = CARTESIAN_POINT ( 'NONE',  ( 754.9967657858570647, -265.5436935675106156, -365.0032342141425943 ) ) ;
#10042 = CARTESIAN_POINT ( 'NONE',  ( 804.6798772138708955, 8.274488250670337663, 334.6312213355107019 ) ) ;
#10043 = CARTESIAN_POINT ( 'NONE',  ( 804.4286716492782716, -89.36187538569299704, -345.3141322388244703 ) ) ;
#10044 = VECTOR ( 'NONE', #44670, 1000.000000000000000 ) ;
#10045 = ADVANCED_FACE ( 'NONE', ( #24088 ), #37736, .F. ) ;
#10046 = CARTESIAN_POINT ( 'NONE',  ( 776.2046728542105711, -212.1908817542436623, 304.8212110874238761 ) ) ;
#10047 = CARTESIAN_POINT ( 'NONE',  ( 810.1134526219336749, -176.5328690171416213, -357.8822607201570349 ) ) ;
#10048 = CARTESIAN_POINT ( 'NONE',  ( 763.2262854647970016, -176.6346026584199933, 309.2812353651462445 ) ) ;
#10049 = AXIS2_PLACEMENT_3D ( 'NONE', #31512, #13279, #92 ) ;
#10050 = CARTESIAN_POINT ( 'NONE',  ( 812.7932403749906598, -423.1800572038737300, -327.7687537140311633 ) ) ;
#10051 = CARTESIAN_POINT ( 'NONE',  ( 787.4999999999992042, -462.9681489794448339, -370.0000000000000568 ) ) ;
#10052 = EDGE_CURVE ( 'NONE', #17907, #7675, #19623, .T. ) ;
#10053 = CARTESIAN_POINT ( 'NONE',  ( 774.6858677611749044, -273.7255117493288026, 315.5713283507209894 ) ) ;
#10054 = CARTESIAN_POINT ( 'NONE',  ( 796.9571628226829034, -47.46360902697148987, 321.2382568024804641 ) ) ;
#10055 = CARTESIAN_POINT ( 'NONE',  ( 791.9812246680005501, -428.6346026584192259, -361.9419747391813189 ) ) ;
#10056 = LINE ( 'NONE', #31289, #26171 ) ;
#10057 = LINE ( 'NONE', #24572, #32107 ) ;
#10059 = CARTESIAN_POINT ( 'NONE',  ( 805.1927285166397041, -328.8164208402375834, 341.8018195045277707 ) ) ;
#10058 = CARTESIAN_POINT ( 'NONE',  ( 794.1144889064781864, -130.1692326535054463, 360.9840315886528401 ) ) ;
#10060 = ORIENTED_EDGE ( 'NONE', *, *, #11724, .F. ) ;
#10061 = VECTOR ( 'NONE', #25650, 1000.000000000000000 ) ;
#10062 = EDGE_CURVE ( 'NONE', #31920, #28192, #13945, .T. ) ;
#10063 = CARTESIAN_POINT ( 'NONE',  ( 772.3691319403857278, -263.2601417444141134, -315.8894580844506663 ) ) ;
#10064 = CARTESIAN_POINT ( 'NONE',  ( 797.6776695296629214, -91.54369356751116982, 357.6776695296636603 ) ) ;
#10065 = CARTESIAN_POINT ( 'NONE',  ( 758.0141637701419768, -255.0783235625958980, -367.2620300519063790 ) ) ;
#10066 = CARTESIAN_POINT ( 'NONE',  ( -784.4999999999993179, -365.3551492539851893, -18.13243251470705886 ) ) ;
#10067 = CARTESIAN_POINT ( 'NONE',  ( 798.0661480581538854, -410.5328690171408539, 309.5768839229118043 ) ) ;
#10068 = EDGE_LOOP ( 'NONE', ( #30437, #6635, #23152, #33092 ) ) ;
#10069 = CARTESIAN_POINT ( 'NONE',  ( 771.2633955100217236, -287.9073299311468759, 363.4237431249939618 ) ) ;
#10070 = CARTESIAN_POINT ( 'NONE',  ( 754.8983024940795303, -42.89650538077842157, -336.9254006560228163 ) ) ;
#10071 = CARTESIAN_POINT ( 'NONE',  ( 800.0135310231082713, -206.0891481129653471, -325.0180583372163028 ) ) ;
#10072 = CARTESIAN_POINT ( 'NONE',  ( 804.9363028652555840, -400.2709662947828519, 338.2165204200192079 ) ) ;
#10073 = CARTESIAN_POINT ( 'NONE',  ( 747.2067596250078623, -123.1800572038747106, -352.2312462859687230 ) ) ;
#10074 = CARTESIAN_POINT ( 'NONE',  ( 759.7806653035535192, -102.9982390220565662, -324.8639956371181370 ) ) ;
#10075 = VERTEX_POINT ( 'NONE', #38202 ) ;
#10076 = CARTESIAN_POINT ( 'NONE',  ( 793.0897708529556667, -30.55451811788062244, -361.3366627262616362 ) ) ;
#10077 = CARTESIAN_POINT ( 'NONE',  ( 766.9102291470427417, -354.5545181178796383, -318.6633372737382501 ) ) ;
#10079 = CARTESIAN_POINT ( 'NONE',  ( 780.5236548040995785, -452.7363362996975411, 314.9735926884559944 ) ) ;
#10078 = CARTESIAN_POINT ( 'NONE',  ( 755.5713283507202505, -125.3618753856928834, 334.6858677611754729 ) ) ;
#10080 = AXIS2_PLACEMENT_3D ( 'NONE', #9342, #12572, #12358 ) ;
#10083 = CARTESIAN_POINT ( 'NONE',  ( 781.2497674668890113, -372.3510508353228374, 375.3608509340180603 ) ) ;
#10082 = DIRECTION ( 'NONE',  ( -0.000000000000000000, 0.000000000000000000, -1.000000000000000000 ) ) ;
#10081 = PLANE ( 'NONE',  #12230 ) ;
#10084 = CARTESIAN_POINT ( 'NONE',  ( 790.0220218866281812, -343.0999726633342561, -363.2186876482849129 ) ) ;
#10085 = CARTESIAN_POINT ( 'NONE',  ( 762.3223304703356007, -343.5436935675103314, -322.3223304703362828 ) ) ;
#10086 = CARTESIAN_POINT ( 'NONE',  ( 797.8822607201568644, -126.5545181178803205, -370.1134526219340160 ) ) ;
#10087 = CARTESIAN_POINT ( 'NONE',  ( 766.4474001241216001, -43.09997266333511590, 307.3154664389482491 ) ) ;
#10089 = DIRECTION ( 'NONE',  ( 1.000000000000000000, 0.000000000000000000, 0.000000000000000000 ) ) ;
#10088 = CARTESIAN_POINT ( 'NONE',  ( -879.9999999999992042, 260.0000000000002274, -179.9999999999999716 ) ) ;
#10090 = CARTESIAN_POINT ( 'NONE',  ( 763.2154366446407039, -309.6237781080502600, -321.4292242960311228 ) ) ;
#10091 = CARTESIAN_POINT ( 'NONE',  ( 814.2805881961230625, -145.6454272087893287, -331.2368401574024119 ) ) ;
#10092 = FACE_OUTER_BOUND ( 'NONE', #7760, .T. ) ;
#10093 = CARTESIAN_POINT ( 'NONE',  ( -858.8365100919713768, 260.0000000000002274, -199.9999999999881481 ) ) ;
#10094 = VECTOR ( 'NONE', #43379, 1000.000000000000000 ) ;
#10095 = CARTESIAN_POINT ( 'NONE',  ( 804.8461984189677878, -338.1908817542433212, 336.9566956441385628 ) ) ;
#10096 = CARTESIAN_POINT ( 'NONE',  ( 811.3240766477731540, -316.3726999360615082, 355.6651683502462902 ) ) ;
#10097 = CARTESIAN_POINT ( 'NONE',  ( 763.0537975583476964, -168.4527844766018347, -371.0346526505628617 ) ) ;
#10098 = CARTESIAN_POINT ( 'NONE',  ( -78.83651009197140525, 240.0000000000000853, -197.2499999999937756 ) ) ;
#10099 = EDGE_CURVE ( 'NONE', #17152, #32355, #20176, .T. ) ;
#10100 = CARTESIAN_POINT ( 'NONE',  ( 750.9282345327678740, -112.9181544815167229, 319.8311093483690115 ) ) ;
#10101 = CARTESIAN_POINT ( 'NONE',  ( 782.5225473063381969, -310.2709662947832499, -375.2698199232970637 ) ) ;
#10102 = CARTESIAN_POINT ( 'NONE',  ( 790.0183182880230106, -452.9681489794449476, -362.9048749981275250 ) ) ;
#10103 = LINE ( 'NONE', #27417, #44866 ) ;
#10104 = CARTESIAN_POINT ( 'NONE',  ( 755.5713283507202505, -197.3618753856926560, 334.6858677611754729 ) ) ;
#10105 = ORIENTED_EDGE ( 'NONE', *, *, #9679, .F. ) ;
#10106 = CARTESIAN_POINT ( 'NONE',  ( 778.7629533639073998, -440.7363362996975980, 375.0009284576466371 ) ) ;
#10107 = CARTESIAN_POINT ( 'NONE',  ( 776.2433038121456548, -372.8965053807773415, -374.8207195650711014 ) ) ;
#10108 = CARTESIAN_POINT ( 'NONE',  ( 808.0189434323515343, -134.0891481129655745, -319.0252816721025511 ) ) ;
#10109 = CARTESIAN_POINT ( 'NONE',  ( 802.5472867521000353, -52.37269993606237506, 350.8726784830461156 ) ) ;
#10110 = CARTESIAN_POINT ( 'NONE',  ( 767.6429770376289525, -393.1800572038737300, -306.8695393053162093 ) ) ;
#10111 = CYLINDRICAL_SURFACE ( 'NONE', #32804, 20.00000000000001776 ) ;
#10112 = CARTESIAN_POINT ( 'NONE',  ( 744.8212110874229666, 5.103494619221427442, 336.2046728542121627 ) ) ;
#10113 = ORIENTED_EDGE ( 'NONE', *, *, #960, .T. ) ;
#10114 = AXIS2_PLACEMENT_3D ( 'NONE', #41791, #31146, #24437 ) ;
#10115 = CARTESIAN_POINT ( 'NONE',  ( 815.1787889125755555, -150.8965053807781089, -343.7953271457877804 ) ) ;
#10116 = CARTESIAN_POINT ( 'NONE',  ( 571.1634899080285095, 256.4999999999999432, -199.9999999999981526 ) ) ;
#10117 = CARTESIAN_POINT ( 'NONE',  ( 764.3348316497523456, -262.7146871989594956, 308.6759233522265617 ) ) ;
#10118 = CARTESIAN_POINT ( 'NONE',  ( 756.5762568750052424, -123.1800572038747106, 348.7366044899774238 ) ) ;
#10119 = VERTEX_POINT ( 'NONE', #27800 ) ;
#10120 = CARTESIAN_POINT ( 'NONE',  ( 778.1981804954714335, -298.2709662947830793, 314.8072714833589885 ) ) ;
#10121 = AXIS2_PLACEMENT_3D ( 'NONE', #25301, #39412, #21843 ) ;
#10122 = CARTESIAN_POINT ( 'NONE',  ( 758.8095938919642549, -8.089148112965974136, -311.6929314249763365 ) ) ;
#10123 = CARTESIAN_POINT ( 'NONE',  ( 792.8617558976345663, -450.5553044913475560, 371.8789995216883995 ) ) ;
#10124 = EDGE_LOOP ( 'NONE', ( #22556, #17858, #39759, #19047 ) ) ;
#10125 = CARTESIAN_POINT ( 'NONE',  ( 797.6776695296629214, -187.5436935675108430, -357.6776695296636603 ) ) ;
#10126 = CARTESIAN_POINT ( 'NONE',  ( 754.3581564841646241, -401.4636090269704027, -316.1443688327762516 ) ) ;
#10127 = CARTESIAN_POINT ( 'NONE',  ( 778.1981804954714335, -34.27096629478407408, 314.8072714833589885 ) ) ;
#10128 = CARTESIAN_POINT ( 'NONE',  ( 759.9864689768902508, -266.0891481129651197, -354.9819416627836404 ) ) ;
#10130 = CARTESIAN_POINT ( 'NONE',  ( 815.0009284576459549, -246.3510508353232638, 338.7629533639073429 ) ) ;
#10129 = CARTESIAN_POINT ( 'NONE',  ( 758.8095938919644823, -368.0891481129647786, 311.6929314249762797 ) ) ;
#10131 = CARTESIAN_POINT ( 'NONE',  ( 814.8230680027162407, -53.80559628986930676, 333.7305795820267917 ) ) ;
#10132 = CARTESIAN_POINT ( 'NONE',  ( 804.1105419155481968, -243.8272453906072030, -347.6308680596136469 ) ) ;
#10133 = CARTESIAN_POINT ( 'NONE',  ( 756.5762568750052424, -267.1800572038742985, -348.7366044899774238 ) ) ;
#10134 = CARTESIAN_POINT ( 'NONE',  ( 802.1676090361155502, -446.6346026584191122, -327.8955696845344505 ) ) ;
#10135 = CARTESIAN_POINT ( 'NONE',  ( 802.1676090361156639, -86.63460265842023489, -327.8955696845344505 ) ) ;
#10136 = CARTESIAN_POINT ( 'NONE',  ( 794.9819416627830151, -252.9982390220560831, 319.9864689768909898 ) ) ;
#10137 = ORIENTED_EDGE ( 'NONE', *, *, #15665, .T. ) ;
#10138 = CARTESIAN_POINT ( 'NONE',  ( 772.5602148656447525, -369.7255117493284615, 305.7998596910095443 ) ) ;
#10139 = LINE ( 'NONE', #38539, #466 ) ;
#10140 = CARTESIAN_POINT ( 'NONE',  ( 748.6759233522253680, -40.37269993606240348, -324.3348316497537098 ) ) ;
#10141 = FACE_OUTER_BOUND ( 'NONE', #11002, .T. ) ;
#10142 = CARTESIAN_POINT ( 'NONE',  ( 831.1634899080286232, 259.9999999999998863, -202.7499999999998295 ) ) ;
#10143 = CARTESIAN_POINT ( 'NONE',  ( 772.4468031744293057, -225.8272453906072599, 363.8651313633793620 ) ) ;
#10144 = CARTESIAN_POINT ( 'NONE',  ( 803.6646147819161570, -113.9073299311474301, 348.8264449731210561 ) ) ;
#10145 = ORIENTED_EDGE ( 'NONE', *, *, #21098, .F. ) ;
#10146 = CARTESIAN_POINT ( 'NONE',  ( 804.8461984189677878, -2.190881754244347945, -336.9566956441385628 ) ) ;
#10147 = CARTESIAN_POINT ( 'NONE',  ( 745.7998596910086917, -77.36187538569302546, -332.5602148656461168 ) ) ;
#10148 = CARTESIAN_POINT ( 'NONE',  ( 786.6156483768007774, -289.4419599262321299, 315.5913626894246136 ) ) ;
#10149 = CARTESIAN_POINT ( 'NONE',  ( 805.1927285166397041, -448.8164208402371855, -341.8018195045277707 ) ) ;
#10150 = CARTESIAN_POINT ( 'NONE',  ( 757.8323909638828582, -26.63460265842046226, -352.1044303154654358 ) ) ;
#10151 = CARTESIAN_POINT ( 'NONE',  ( 791.0478386215596629, 2.172754609392001601, 306.7653713866226326 ) ) ;
#10152 = CARTESIAN_POINT ( 'NONE',  ( 745.4481719005789273, -195.7255117493289731, -347.5162901302853129 ) ) ;
#10153 = CARTESIAN_POINT ( 'NONE',  ( 802.1676090361156639, -86.63460265842023489, 327.8955696845344505 ) ) ;
#10154 = CARTESIAN_POINT ( 'NONE',  ( 939.9999999999992042, 56.60618624968560653, 350.0000000000000000 ) ) ;
#10155 = CARTESIAN_POINT ( 'NONE',  ( 999.9999999999992042, 479.5857864376268935, -359.5857864376268935 ) ) ;
#10156 = CARTESIAN_POINT ( 'NONE',  ( 754.0944755984390895, -279.6237781080503737, -364.1009440267246760 ) ) ;
#10157 = CARTESIAN_POINT ( 'NONE',  ( 814.8207195650702488, -410.1908817542430370, 336.2433038121456548 ) ) ;
#10158 = CARTESIAN_POINT ( 'NONE',  ( 808.3070685750230950, -282.9982390220558841, -361.1904061080339261 ) ) ;
#10159 = CARTESIAN_POINT ( 'NONE',  ( -809.9999999999993179, -512.9681489794448908, -339.9999999999999432 ) ) ;
#10160 = CARTESIAN_POINT ( 'NONE',  ( 782.5225473063381969, -382.2709662947828519, 375.2698199232970637 ) ) ;
#10161 = CARTESIAN_POINT ( 'NONE',  ( 758.8095938919644823, -8.089148112965974136, 311.6929314249762797 ) ) ;
#10162 = CARTESIAN_POINT ( 'NONE',  ( 759.9864689768902508, -386.0891481129647786, -354.9819416627836404 ) ) ;
#10163 = CARTESIAN_POINT ( 'NONE',  ( 770.0799878456142551, -13.98741447168760033, 362.9823548866085616 ) ) ;
#10164 = CARTESIAN_POINT ( 'NONE',  ( 781.2497674668890113, -60.35105083532383219, -375.3608509340180603 ) ) ;
#10165 = CARTESIAN_POINT ( 'NONE',  ( 757.2208543904082489, -184.7146871989598083, -350.9844846989624330 ) ) ;
#10166 = CARTESIAN_POINT ( 'NONE',  ( 812.6845335610512393, -175.9874144716871172, 353.5525998758768651 ) ) ;
#10167 = CARTESIAN_POINT ( 'NONE',  ( 794.9819416627830151, -12.99823902205686821, 319.9864689768909898 ) ) ;
#10168 = ORIENTED_EDGE ( 'NONE', *, *, #21300, .T. ) ;
#10169 = CARTESIAN_POINT ( 'NONE',  ( 762.1405469898971887, -73.54369356751118403, -357.8594530101015607 ) ) ;
#10170 = CARTESIAN_POINT ( 'NONE',  ( 793.2243759319678702, -194.5328690171415644, -318.4439275373583200 ) ) ;
#10171 = CARTESIAN_POINT ( 'NONE',  ( 774.6858677611749044, -153.7255117493291721, 315.5713283507209894 ) ) ;
#10172 = CARTESIAN_POINT ( 'NONE',  ( 747.3154664389472828, 4.012585528312341054, -326.4474001241230781 ) ) ;
#10173 =( REPRESENTATION_RELATIONSHIP ('NONE','NONE', #39835, #20360 ) REPRESENTATION_RELATIONSHIP_WITH_TRANSFORMATION ( #28346 )SHAPE_REPRESENTATION_RELATIONSHIP( ) );
#10174 = CARTESIAN_POINT ( 'NONE',  ( 805.1927285166399315, -280.8164208402378108, 341.8018195045277707 ) ) ;
#10175 = DIRECTION ( 'NONE',  ( 1.000000000000000000, 0.000000000000000000, 0.000000000000000000 ) ) ;
#10176 = ORIENTED_EDGE ( 'NONE', *, *, #25485, .F. ) ;
#10177 = CARTESIAN_POINT ( 'NONE',  ( 805.0264073115434940, -30.35105083532391390, 339.4763451958999099 ) ) ;
#10178 = CARTESIAN_POINT ( 'NONE',  ( 745.7194118038753459, -301.6454272087889308, -348.7631598425976449 ) ) ;
#10179 = VECTOR ( 'NONE', #18760, 1000.000000000000000 ) ;
#10180 = CARTESIAN_POINT ( 'NONE',  ( 754.9967657858570647, -265.5436935675106156, 365.0032342141425943 ) ) ;
#10181 = CARTESIAN_POINT ( 'NONE',  ( 779.4763451958990572, -344.7363362996978253, 365.0264073115438919 ) ) ;
#10182 = CARTESIAN_POINT ( 'NONE',  ( 758.6633372737375112, -428.5328690171409107, 326.9102291470432533 ) ) ;
#10183 = CARTESIAN_POINT ( 'NONE',  ( 780.5236548040995785, -140.7363362996984506, -314.9735926884559944 ) ) ;
#10184 = CARTESIAN_POINT ( 'NONE',  ( 804.4286716492782716, -137.3618753856928265, -345.3141322388244703 ) ) ;
#10185 = CARTESIAN_POINT ( 'NONE',  ( 759.7806653035535192, -318.9982390220558841, -324.8639956371181370 ) ) ;
#10186 = ORIENTED_EDGE ( 'NONE', *, *, #24165, .F. ) ;
#10187 = CARTESIAN_POINT ( 'NONE',  ( 775.9200461376533440, -335.8055962898683902, 315.3028492785443291 ) ) ;
#10188 = DIRECTION ( 'NONE',  ( 1.337618101958019798E-16, -1.000000000000000000, 0.000000000000000000 ) ) ;
#10189 = CARTESIAN_POINT ( 'NONE',  ( 755.3028492785439312, -135.2817908451530116, 335.9200461376539693 ) ) ;
#10190 = CARTESIAN_POINT ( 'NONE',  ( 781.7834795799800531, -10.81642084023869543, 315.0636971347436202 ) ) ;
#10191 = ORIENTED_EDGE ( 'NONE', *, *, #3007, .T. ) ;
#10192 = CARTESIAN_POINT ( 'NONE',  ( 804.1009440267234822, -383.4636090269704596, -314.0944755984392600 ) ) ;
#10193 = FACE_BOUND ( 'NONE', #19044, .T. ) ;
#10194 = CARTESIAN_POINT ( 'NONE',  ( 779.4763451958990572, -224.7363362996982232, 365.0264073115438919 ) ) ;
#10195 = CARTESIAN_POINT ( 'NONE',  ( 773.7305795820266212, -225.2817908451527273, 374.8230680027170365 ) ) ;
#10196 = CARTESIAN_POINT ( 'NONE',  ( 799.4546378042377910, -201.0783235625961254, 356.1575198192848006 ) ) ;
#10197 = CARTESIAN_POINT ( 'NONE',  ( 805.1927285166397041, -328.8164208402375834, -341.8018195045277707 ) ) ;
#10198 =( NAMED_UNIT ( * ) PLANE_ANGLE_UNIT ( ) SI_UNIT ( $, .RADIAN. ) );
#10199 = CARTESIAN_POINT ( 'NONE',  ( 766.0291762391763086, -226.9181544815163534, -360.7704444035551319 ) ) ;
#10200 = CARTESIAN_POINT ( 'NONE',  ( 747.2067596250078623, -75.18005720387485269, 352.2312462859687230 ) ) ;
#10201 = CARTESIAN_POINT ( 'NONE',  ( 803.8904222555790966, -452.9681489794450044, 350.1048529224749473 ) ) ;
#10202 = CARTESIAN_POINT ( 'NONE',  ( 751.9810565676468741, -410.0891481129647218, -360.9747183278973921 ) ) ;
#10203 = DIRECTION ( 'NONE',  ( -1.000000000000000000, 0.000000000000000000, 0.000000000000000000 ) ) ;
#10204 = VECTOR ( 'NONE', #44836, 1000.000000000000000 ) ;
#10205 = CARTESIAN_POINT ( 'NONE',  ( 814.2805881961230625, -361.6454272087887603, 331.2368401574024119 ) ) ;
#10206 = CARTESIAN_POINT ( 'NONE',  ( 804.6401732501814195, -455.9581923679652391, -357.6484231659003967 ) ) ;
#10207 = CARTESIAN_POINT ( 'NONE',  ( 792.3570229623688874, -285.1800572038740711, 373.1304606946836202 ) ) ;
#10208 = CARTESIAN_POINT ( 'NONE',  ( 814.5518280994195948, -63.72551174932939233, -332.4837098697145734 ) ) ;
#10209 = CARTESIAN_POINT ( 'NONE',  ( 801.9419747391806368, -282.4527844766014937, -351.9812246680014027 ) ) ;
#10210 = DIRECTION ( 'NONE',  ( 0.000000000000000000, -0.6438296778008192334, -0.7651688349527138167 ) ) ;
#10211 = CARTESIAN_POINT ( 'NONE',  ( 757.8323909638827445, -410.6346026584191122, 352.1044303154654358 ) ) ;
#10212 = CARTESIAN_POINT ( 'NONE',  ( 779.4763451958990572, -152.7363362996983938, 365.0264073115438919 ) ) ;
#10213 = CARTESIAN_POINT ( 'NONE',  ( 807.2620300519052989, -24.00906357242609346, -318.0141637701419768 ) ) ;
#10214 = CARTESIAN_POINT ( 'NONE',  ( 754.8983024940795303, -66.89650538077835051, -336.9254006560228163 ) ) ;
#10215 = CARTESIAN_POINT ( 'NONE',  ( 812.6845335610512393, -79.98741447168740137, 353.5525998758768651 ) ) ;
#10216 = CARTESIAN_POINT ( 'NONE',  ( 756.5762568750052424, -411.1800572038738437, 348.7366044899774238 ) ) ;
#10217 = CARTESIAN_POINT ( 'NONE',  ( -180.7583438952258348, 394.6698570112193920, -274.9999999999999432 ) ) ;
#10218 = DIRECTION ( 'NONE',  ( 0.000000000000000000, 0.000000000000000000, -1.000000000000000000 ) ) ;
#10219 = CARTESIAN_POINT ( 'NONE',  ( 804.9363028652555840, -424.2709662947829088, 338.2165204200192079 ) ) ;
#10220 = VERTEX_POINT ( 'NONE', #38653 ) ;
#10221 = CARTESIAN_POINT ( 'NONE',  ( 759.9864689768902508, -74.08914811296577341, -354.9819416627836404 ) ) ;
#10222 = CARTESIAN_POINT ( 'NONE',  ( 756.7813123517142913, -355.9874144716865203, -329.9779781133712504 ) ) ;
#10224 = CARTESIAN_POINT ( 'NONE',  ( 781.7834795799800531, -178.8164208402381519, 315.0636971347436202 ) ) ;
#10223 = CARTESIAN_POINT ( 'NONE',  ( 774.6312213355099630, -239.3618753856924570, 364.6798772138717482 ) ) ;
#10225 = CARTESIAN_POINT ( 'NONE',  ( 813.9316612368132837, -391.4419599262317888, -348.6739635108323228 ) ) ;
#10226 = PLANE ( 'NONE',  #38925 ) ;
#10227 = VERTEX_POINT ( 'NONE', #31494 ) ;
#10228 = CARTESIAN_POINT ( 'NONE',  ( 800.2193346964447755, -402.9982390220555430, 355.1360043628815788 ) ) ;
#10229 = EDGE_LOOP ( 'NONE', ( #34944, #43643 ) ) ;
#10230 = CARTESIAN_POINT ( 'NONE',  ( 744.7301800767019131, -220.8164208402379529, -337.4774526936615757 ) ) ;
#10231 = CARTESIAN_POINT ( 'NONE',  ( 751.9810565676468741, -146.0891481129655176, 360.9747183278973921 ) ) ;
#10232 = ORIENTED_EDGE ( 'NONE', *, *, #25795, .F. ) ;
#10233 = CARTESIAN_POINT ( 'NONE',  ( 744.9990715423526808, -186.3510508353234343, 341.2370466360926002 ) ) ;
#10234 = CARTESIAN_POINT ( 'NONE',  ( 756.3353852180820240, -197.9073299311472169, -331.1735550268787733 ) ) ;
#10235 = ORIENTED_EDGE ( 'NONE', *, *, #10256, .T. ) ;
#10236 = AXIS2_PLACEMENT_3D ( 'NONE', #17139, #7217, #24505 ) ;
#10237 = CARTESIAN_POINT ( 'NONE',  ( 765.0180583372156207, -360.9982390220557704, -360.0135310231089534 ) ) ;
#10238 = CARTESIAN_POINT ( 'NONE',  ( 771.2633955100217236, -23.90732993114773919, -363.4237431249939618 ) ) ;
#10239 = CARTESIAN_POINT ( 'NONE',  ( 780.5290396650775619, -228.3510508353232922, 365.2837595273619513 ) ) ;
#10240 = CARTESIAN_POINT ( 'NONE',  ( 794.9999999999993179, 205.0000000000000568, -255.0000000000000000 ) ) ;
#10241 = FACE_OUTER_BOUND ( 'NONE', #41389, .T. ) ;
#10242 = EDGE_CURVE ( 'NONE', #45600, #15704, #41002, .T. ) ;
#10243 = ORIENTED_EDGE ( 'NONE', *, *, #36032, .F. ) ;
#10244 = CARTESIAN_POINT ( 'NONE',  ( 771.2633955100217236, 0.09267006885218045942, -363.4237431249939618 ) ) ;
#10245 = DIRECTION ( 'NONE',  ( -0.7014439490181307857, 0.1263042864341424876, -0.7014439490181749726 ) ) ;
#10246 = LINE ( 'NONE', #20634, #15975 ) ;
#10247 = VERTEX_POINT ( 'NONE', #16726 ) ;
#10248 = CARTESIAN_POINT ( 'NONE',  ( 812.3518521366052028, -289.0999726633343698, -326.5853460496235243 ) ) ;
#10249 = CARTESIAN_POINT ( 'NONE',  ( 813.5763878283155464, -123.8272453906076009, 351.1614460488615350 ) ) ;
#10251 = CARTESIAN_POINT ( 'NONE',  ( 792.1044303154645831, -228.4527844766015789, -317.8323909638837677 ) ) ;
#10250 = CARTESIAN_POINT ( 'NONE',  ( 939.9999999999992042, 74.99999999999984368, -360.0000000000000000 ) ) ;
#10252 = CARTESIAN_POINT ( 'NONE',  ( 776.9566956441375396, -396.8965053807772847, -364.8461984189686405 ) ) ;
#10253 = CARTESIAN_POINT ( 'NONE',  ( 939.9999999999992042, 47.45399382421949497, -201.9999999999999432 ) ) ;
#10254 = CARTESIAN_POINT ( 'NONE',  ( 803.4237431249931660, 8.819942796124882634, -331.2633955100225194 ) ) ;
#10255 = CARTESIAN_POINT ( 'NONE',  ( 760.7433823573367135, -108.0090635724258448, -355.9930595647440441 ) ) ;
#10256 = EDGE_CURVE ( 'NONE', #22008, #7346, #10464, .T. ) ;
#10257 = CARTESIAN_POINT ( 'NONE',  ( 793.5525998758768083, -391.0999726633340288, 372.6845335610516941 ) ) ;
#10258 = DIRECTION ( 'NONE',  ( 1.644774851296528363E-16, -1.000000000000000000, 0.000000000000000000 ) ) ;
#10259 = CARTESIAN_POINT ( 'NONE',  ( 793.4146539503750546, -1.987414471687640294, -307.6481478633938877 ) ) ;
#10260 = CARTESIAN_POINT ( 'NONE',  ( 747.2067596250078623, -315.1800572038740711, -352.2312462859687230 ) ) ;
#10261 = FACE_OUTER_BOUND ( 'NONE', #19715, .T. ) ;
#10262 = CARTESIAN_POINT ( 'NONE',  ( 774.6858677611749044, 14.27448825067031812, 315.5713283507209894 ) ) ;
#10263 = CARTESIAN_POINT ( 'NONE',  ( 800.2193346964447755, -66.99823902205672255, -355.1360043628815788 ) ) ;
#10264 = CARTESIAN_POINT ( 'NONE',  ( 754.3581564841646241, -233.4636090269708575, 316.1443688327762516 ) ) ;
#10265 = CARTESIAN_POINT ( 'NONE',  ( 746.7653713866222915, -161.2601417444143976, -351.0478386215610271 ) ) ;
#10266 = CARTESIAN_POINT ( 'NONE',  ( 745.7998596910086917, -173.3618753856927128, 332.5602148656461168 ) ) ;
#10267 = CARTESIAN_POINT ( 'NONE',  ( 810.4231160770870019, -0.5545181178807169209, -321.9338519418446936 ) ) ;
#10268 = FACE_OUTER_BOUND ( 'NONE', #33046, .T. ) ;
#10269 = CARTESIAN_POINT ( 'NONE',  ( 778.1981804954714335, -298.2709662947830793, 314.8072714833589885 ) ) ;
#10270 = CARTESIAN_POINT ( 'NONE',  ( 798.5707757039680246, -53.46360902697146855, 356.7845633553585003 ) ) ;
#10271 = EDGE_CURVE ( 'NONE', #2255, #36814, #32900, .T. ) ;
#10272 = CARTESIAN_POINT ( 'NONE',  ( 762.1405469898971887, -409.5436935675101040, -357.8594530101015607 ) ) ;
#10273 = VECTOR ( 'NONE', #27260, 1000.000000000000000 ) ;
#10274 = CARTESIAN_POINT ( 'NONE',  ( 769.9999999999992042, 205.0000000000000568, -339.9999999999999432 ) ) ;
#10276 = ADVANCED_FACE ( 'NONE', ( #45361 ), #41895, .T. ) ;
#10275 = DIRECTION ( 'NONE',  ( -1.000000000000000000, 0.000000000000000000, -0.000000000000000000 ) ) ;
#10278 = CARTESIAN_POINT ( 'NONE',  ( 771.2633955100217236, -335.9073299311468190, 363.4237431249939618 ) ) ;
#10277 = CARTESIAN_POINT ( 'NONE',  ( 761.2382568024794409, -135.6237781080508853, 356.9571628226838129 ) ) ;
#10279 = ORIENTED_EDGE ( 'NONE', *, *, #15141, .F. ) ;
#10280 = CARTESIAN_POINT ( 'NONE',  ( 775.9200461376533440, -263.8055962898686175, -315.3028492785443291 ) ) ;
#10281 = CARTESIAN_POINT ( 'NONE',  ( 756.3353852180819104, -101.9073299311474727, 331.1735550268788302 ) ) ;
#10282 = CARTESIAN_POINT ( 'NONE',  ( 791.1614460488616487, -275.2601417444140566, -373.5763878283158874 ) ) ;
#10283 = CARTESIAN_POINT ( 'NONE',  ( 989.9999999999992042, 249.9999999999998863, -209.9999999999999716 ) ) ;
#10284 = CARTESIAN_POINT ( 'NONE',  ( 812.6845335610512393, -415.9874144716862361, 353.5525998758768651 ) ) ;
#10285 = VERTEX_POINT ( 'NONE', #6774 ) ;
#10286 = CARTESIAN_POINT ( 'NONE',  ( 778.2165204200184689, -286.8164208402378677, 364.9363028652563230 ) ) ;
#10287 = CARTESIAN_POINT ( 'NONE',  ( 769.1273215169530886, -46.71468719896022748, -317.4527132478988847 ) ) ;
#10288 = CARTESIAN_POINT ( 'NONE',  ( 755.5713283507202505, -197.3618753856926560, -334.6858677611754729 ) ) ;
#10289 = CARTESIAN_POINT ( 'NONE',  ( 767.8955696845333705, -408.4527844766009252, 362.1676090361162323 ) ) ;
#10290 = CARTESIAN_POINT ( 'NONE',  ( 754.9967657858570647, -97.54369356751112718, -365.0032342141425374 ) ) ;
#10291 = CARTESIAN_POINT ( 'NONE',  ( 755.3201227861273992, -99.72551174932931417, -345.3687786644892981 ) ) ;
#10292 = ORIENTED_EDGE ( 'NONE', *, *, #16475, .T. ) ;
#10293 = CARTESIAN_POINT ( 'NONE',  ( 800.9840315886518738, -52.91815448151692891, -354.1144889064786412 ) ) ;
#10294 = CARTESIAN_POINT ( 'NONE',  ( 754.7162404726377645, -374.7363362996978253, -339.4709603349214717 ) ) ;
#10295 = EDGE_CURVE ( 'NONE', #13889, #16040, #34032, .T. ) ;
#10297 = CARTESIAN_POINT ( 'NONE',  ( 800.9840315886518738, -436.9181544815157281, 354.1144889064786412 ) ) ;
#10296 = CARTESIAN_POINT ( 'NONE',  ( 774.6858677611749044, -129.7255117493292289, 315.5713283507209894 ) ) ;
#10298 = CARTESIAN_POINT ( 'NONE',  ( 758.6633372737375112, -116.5328690171418202, 326.9102291470432533 ) ) ;
#10301 = CARTESIAN_POINT ( 'NONE',  ( 795.6651683502461765, -346.7146871989592682, 371.3240766477733814 ) ) ;
#10300 = DIRECTION ( 'NONE',  ( -1.000000000000000000, -0.000000000000000000, 0.000000000000000000 ) ) ;
#10299 = DIRECTION ( 'NONE',  ( 0.000000000000000000, 0.000000000000000000, 1.000000000000000000 ) ) ;
#10302 = EDGE_CURVE ( 'NONE', #12556, #30518, #13030, .T. ) ;
#10303 = ORIENTED_EDGE ( 'NONE', *, *, #17898, .T. ) ;
#10304 = CARTESIAN_POINT ( 'NONE',  ( 804.1105419155481968, -363.8272453906068336, -347.6308680596136469 ) ) ;
#10305 = CARTESIAN_POINT ( 'NONE',  ( 797.8594530101008786, -349.5436935675102745, -322.1405469898980982 ) ) ;
#10306 = CARTESIAN_POINT ( 'NONE',  ( 748.6759233522253680, -160.3726999360620482, -324.3348316497537098 ) ) ;
#10307 = VECTOR ( 'NONE', #13946, 1000.000000000000114 ) ;
#10308 = CARTESIAN_POINT ( 'NONE',  ( 745.5313806188320314, -39.28179084515331709, 333.7943932421247268 ) ) ;
#10310 = LINE ( 'NONE', #7085, #34439 ) ;
#10309 = CARTESIAN_POINT ( 'NONE',  ( 779.9999999999992042, 16.45630643248849267, 339.9999999999999432 ) ) ;
#10311 = CARTESIAN_POINT ( 'NONE',  ( 759.2295555964440155, -280.1692326535049347, -353.9708237608231229 ) ) ;
#10312 = CARTESIAN_POINT ( 'NONE',  ( 800.0135310231082713, -446.0891481129646081, -325.0180583372163028 ) ) ;
#10313 = CARTESIAN_POINT ( 'NONE',  ( 812.3518521366052028, -145.0999726633347677, -326.5853460496235243 ) ) ;
#10314 = CARTESIAN_POINT ( 'NONE',  ( 989.9999999999992042, -431.4567479753240491, -350.0000000000000000 ) ) ;
#10315 = DIRECTION ( 'NONE',  ( -1.880165489482579047E-16, -1.000000000000000000, -0.000000000000000000 ) ) ;
#10316 = EDGE_CURVE ( 'NONE', #6854, #12114, #27649, .T. ) ;
#10317 = CARTESIAN_POINT ( 'NONE',  ( 793.9708237608222134, -358.9181544815160123, 319.2295555964448681 ) ) ;
#10318 = CARTESIAN_POINT ( 'NONE',  ( 762.1177392798416577, -354.5545181178796383, 309.8865473780659272 ) ) ;
#10319 = CARTESIAN_POINT ( 'NONE',  ( 745.7998596910086917, -197.3618753856926560, -332.5602148656461168 ) ) ;
#10320 = DIRECTION ( 'NONE',  ( 0.000000000000000000, 0.000000000000000000, 1.000000000000000000 ) ) ;
#10321 = CARTESIAN_POINT ( 'NONE',  ( 807.2620300519052989, -120.0090635724258021, 318.0141637701419768 ) ) ;
#10322 = CARTESIAN_POINT ( 'NONE',  ( 748.9653473494363425, -314.6346026584194533, -356.9462024416521331 ) ) ;
#10323 = CARTESIAN_POINT ( 'NONE',  ( 999.9999999999992042, 249.9999999999998863, -200.9999999999999432 ) ) ;
#10324 = FACE_OUTER_BOUND ( 'NONE', #34544, .T. ) ;
#10325 = CARTESIAN_POINT ( 'NONE',  ( 756.5762568750052424, -171.1800572038745543, 348.7366044899774238 ) ) ;
#10326 = ORIENTED_EDGE ( 'NONE', *, *, #38314, .T. ) ;
#10327 = CARTESIAN_POINT ( 'NONE',  ( 802.2119215644370342, -414.0090635724249637, 367.5423716828165084 ) ) ;
#10328 = CARTESIAN_POINT ( 'NONE',  ( 798.0661480581538854, -362.5328690171410813, -309.5768839229118043 ) ) ;
#10329 = CARTESIAN_POINT ( 'NONE',  ( 813.1304606946830518, -137.9073299311473875, -352.3570229623690580 ) ) ;
#10330 = CARTESIAN_POINT ( 'NONE',  ( 796.7737145352015204, -428.6346026584192259, -370.7187646348536987 ) ) ;
#10332 = ADVANCED_FACE ( 'NONE', ( #31932 ), #11387, .F. ) ;
#10331 = FACE_BOUND ( 'NONE', #30063, .T. ) ;
#10333 = CARTESIAN_POINT ( 'NONE',  ( 805.9055244015594326, -3.623778108051270319, 315.8990559732753240 ) ) ;
#10334 = ORIENTED_EDGE ( 'NONE', *, *, #43836, .T. ) ;
#10335 = CARTESIAN_POINT ( 'NONE',  ( 744.9990715423526808, -162.3510508353235196, -341.2370466360926002 ) ) ;
#10336 = DIRECTION ( 'NONE',  ( 0.000000000000000000, 0.000000000000000000, 1.000000000000000000 ) ) ;
#10337 = CARTESIAN_POINT ( 'NONE',  ( 805.9055244015594326, -315.6237781080503169, 315.8990559732753240 ) ) ;
#10338 = CARTESIAN_POINT ( 'NONE',  ( 792.1044303154646968, -132.4527844766019200, 317.8323909638837677 ) ) ;
#10339 = VERTEX_POINT ( 'NONE', #17864 ) ;
#10340 = CARTESIAN_POINT ( 'NONE',  ( 759.9864689768902508, -314.0891481129650629, 354.9819416627836404 ) ) ;
#10341 = CARTESIAN_POINT ( 'NONE',  ( 763.0537975583475827, -24.45278447660229304, -371.0346526505627480 ) ) ;
#10342 = DIRECTION ( 'NONE',  ( 0.000000000000000000, 0.000000000000000000, 1.000000000000000000 ) ) ;
#10343 = VERTEX_POINT ( 'NONE', #769 ) ;
#10344 = CARTESIAN_POINT ( 'NONE',  ( 791.0478386215596629, -405.8272453906067199, -306.7653713866226326 ) ) ;
#10345 = VERTEX_POINT ( 'NONE', #35184 ) ;
#10346 = ADVANCED_FACE ( 'NONE', ( #18100 ), #14405, .F. ) ;
#10347 = CARTESIAN_POINT ( 'NONE',  ( 768.0187753319979720, -32.63460265842044095, 318.0580252608186242 ) ) ;
#10348 = CARTESIAN_POINT ( 'NONE',  ( 755.5713283507202505, -245.3618753856925139, -334.6858677611754729 ) ) ;
#10350 = CARTESIAN_POINT ( 'NONE',  ( 764.3348316497523456, -238.7146871989596661, 308.6759233522265617 ) ) ;
#10349 = CARTESIAN_POINT ( 'NONE',  ( 772.5602148656447525, -345.7255117493285184, 305.7998596910095443 ) ) ;
#10351 = ADVANCED_FACE ( 'NONE', ( #25016 ), #7011, .T. ) ;
#10352 = CARTESIAN_POINT ( 'NONE',  ( 772.4468031744293057, -249.8272453906072315, -363.8651313633793620 ) ) ;
#10353 = CARTESIAN_POINT ( 'NONE',  ( 754.8072714833581358, -268.8164208402378108, -338.1981804954720587 ) ) ;
#10354 = CARTESIAN_POINT ( 'NONE',  ( 795.1360043628808398, -452.0891481129646081, -360.2193346964456282 ) ) ;
#10355 = CARTESIAN_POINT ( 'NONE',  ( 792.1044303154645831, -84.45278447660206211, -317.8323909638837677 ) ) ;
#10356 = CARTESIAN_POINT ( 'NONE',  ( 802.1676090361156639, -254.6346026584196238, 327.8955696845344505 ) ) ;
#10357 = EDGE_LOOP ( 'NONE', ( #42044, #27787, #16948, #8868 ) ) ;
#10358 = CARTESIAN_POINT ( 'NONE',  ( 772.4837098697144029, -407.3618753856920307, 374.5518280994205611 ) ) ;
#10359 = DIRECTION ( 'NONE',  ( -1.000000000000000000, 0.000000000000000000, 0.000000000000000000 ) ) ;
#10360 = CARTESIAN_POINT ( 'NONE',  ( 771.3260364891663130, -43.64542720878966975, -306.0683387631859773 ) ) ;
#10361 = DIRECTION ( 'NONE',  ( -0.000000000000000000, 1.000000000000000000, -0.000000000000000000 ) ) ;
#10363 = EDGE_CURVE ( 'NONE', #33702, #24407, #42802, .T. ) ;
#10362 = CARTESIAN_POINT ( 'NONE',  ( 999.9999999999992042, 248.9999999999998863, -200.9999999999999432 ) ) ;
#10364 = CARTESIAN_POINT ( 'NONE',  ( 760.7433823573367135, -276.0090635724253048, 355.9930595647440441 ) ) ;
#10365 = CARTESIAN_POINT ( 'NONE',  ( 768.0187753319979720, -128.6346026584201354, 318.0580252608186242 ) ) ;
#10366 = ORIENTED_EDGE ( 'NONE', *, *, #28918, .F. ) ;
#10367 = CARTESIAN_POINT ( 'NONE',  ( 800.9840315886518738, -4.918154481517067467, -354.1144889064786412 ) ) ;
#10368 = CARTESIAN_POINT ( 'NONE',  ( 792.2312462859673587, -59.90732993114762905, -307.2067596250082602 ) ) ;
#10369 = CARTESIAN_POINT ( 'NONE',  ( 804.9511171171677688, -293.8055962898685607, 335.8780910478229202 ) ) ;
#10370 = CARTESIAN_POINT ( 'NONE',  ( 800.2193346964447755, -450.9982390220554294, -355.1360043628815788 ) ) ;
#10371 = CARTESIAN_POINT ( 'NONE',  ( 757.7880784355613741, 5.990936427573807954, 312.4576283171834916 ) ) ;
#10372 = CARTESIAN_POINT ( 'NONE',  ( 772.4837098697144029, -215.3618753856925423, -374.5518280994205611 ) ) ;
#10373 = CARTESIAN_POINT ( 'NONE',  ( 792.3570229623688874, -189.1800572038744122, 373.1304606946836202 ) ) ;
#10374 = CARTESIAN_POINT ( 'NONE',  ( 759.7806653035534055, -78.99823902205662307, 324.8639956371180801 ) ) ;
#10375 = DIRECTION ( 'NONE',  ( 0.000000000000000000, 1.000000000000000000, 0.000000000000000000 ) ) ;
#10376 = CARTESIAN_POINT ( 'NONE',  ( 746.0683387631852383, -259.4419599262322436, -331.3260364891676204 ) ) ;
#10377 = CARTESIAN_POINT ( 'NONE',  ( 814.2805881961230625, -409.6454272087884760, 331.2368401574024119 ) ) ;
#10378 = CARTESIAN_POINT ( 'NONE',  ( 749.2812353651451076, -294.4527844766013800, -323.2262854647983090 ) ) ;
#10379 = DIRECTION ( 'NONE',  ( 0.000000000000000000, 0.000000000000000000, 1.000000000000000000 ) ) ;
#10380 = CARTESIAN_POINT ( 'NONE',  ( 765.8855110935204493, -358.1692326535047641, 319.0159684113471599 ) ) ;
#10381 = CARTESIAN_POINT ( 'NONE',  ( 811.0346526505617248, -38.63460265842041963, 323.0537975583478101 ) ) ;
#10382 = CARTESIAN_POINT ( 'NONE',  ( 812.6845335610512393, -31.98741447168754348, -353.5525998758768651 ) ) ;
#10383 = CARTESIAN_POINT ( 'NONE',  ( 754.8072714833581358, -388.8164208402374129, -338.1981804954720587 ) ) ;
#10384 = CARTESIAN_POINT ( 'NONE',  ( 789.9200121543843807, -25.98741447168755769, 317.0176451133914384 ) ) ;
#10385 = CARTESIAN_POINT ( 'NONE',  ( 755.5713283507202505, -197.3618753856926560, -334.6858677611754729 ) ) ;
#10386 = CARTESIAN_POINT ( 'NONE',  ( 766.5853460496234675, -37.98741447168752927, -372.3518521366060554 ) ) ;
#10387 = CARTESIAN_POINT ( 'NONE',  ( 799.4546378042377910, -201.0783235625961254, -356.1575198192848006 ) ) ;
#10388 = CARTESIAN_POINT ( 'NONE',  ( 800.1688906516307043, -202.1692326535051905, 369.0717654672308186 ) ) ;
#10389 = CARTESIAN_POINT ( 'NONE',  ( 762.3223304703356007, -7.543693567511430942, 322.3223304703362828 ) ) ;
#10390 = EDGE_LOOP ( 'NONE', ( #40177, #25499, #16666, #24008, #19432, #34508 ) ) ;
#10391 = CARTESIAN_POINT ( 'NONE',  ( 805.1927285166397041, -88.81642084023842187, -341.8018195045277707 ) ) ;
#10392 = CARTESIAN_POINT ( 'NONE',  ( 757.2208543904082489, -208.7146871989596946, -350.9844846989624330 ) ) ;
#10393 = CARTESIAN_POINT ( 'NONE',  ( 804.6798772138708955, -207.7255117493289447, 334.6312213355107019 ) ) ;
#10394 = PRODUCT_DEFINITION_SHAPE ( 'NONE', 'NONE',  #24214 ) ;
#10395 = CARTESIAN_POINT ( 'NONE',  ( 771.2368401574024119, -37.44195992623299674, -374.2805881961240857 ) ) ;
#10396 = CARTESIAN_POINT ( 'NONE',  ( 797.8594530101009923, -325.5436935675104451, 322.1405469898982119 ) ) ;
#10397 = CARTESIAN_POINT ( 'NONE',  ( 1820.038553321469863, -418.3138125091624602, 201.9999999999998863 ) ) ;
#10398 = ORIENTED_EDGE ( 'NONE', *, *, #10616, .F. ) ;
#10399 = CARTESIAN_POINT ( 'NONE',  ( 754.8983024940795303, -66.89650538077835051, 336.9254006560228163 ) ) ;
#10400 = CARTESIAN_POINT ( 'NONE',  ( 744.6391490659812007, -302.7363362996979959, -338.7502325331110455 ) ) ;
#10401 = CARTESIAN_POINT ( 'NONE',  ( 755.2512626584698410, -247.5436935675106724, 315.2512626584710915 ) ) ;
#10402 = CARTESIAN_POINT ( 'NONE',  ( 755.8894580844503253, -351.8272453906068336, 332.3691319403863531 ) ) ;
#10403 = CARTESIAN_POINT ( 'NONE',  ( 756.1348686366196716, -425.2601417444136018, 347.5531968255698416 ) ) ;
#10404 = CARTESIAN_POINT ( 'NONE',  ( 790.0220218866281812, -151.0999726633347677, -363.2186876482849129 ) ) ;
#10405 = CARTESIAN_POINT ( 'NONE',  ( 785.3687786644884454, -131.3618753856928834, -315.3201227861279676 ) ) ;
#10406 = CARTESIAN_POINT ( 'NONE',  ( 804.6798772138710092, -351.7255117493284615, -334.6312213355106451 ) ) ;
#10407 = ORIENTED_EDGE ( 'NONE', *, *, #20111, .F. ) ;
#10408 = CARTESIAN_POINT ( 'NONE',  ( 805.1927285166397041, -448.8164208402371855, -341.8018195045277707 ) ) ;
#10409 = CARTESIAN_POINT ( 'NONE',  ( 796.7737145352015204, -284.6346026584196807, 370.7187646348536987 ) ) ;
#10410 = CARTESIAN_POINT ( 'NONE',  ( 805.0264073115434940, -318.3510508353230080, 339.4763451958999099 ) ) ;
#10411 = LINE ( 'NONE', #20795, #16751 ) ;
#10412 = CARTESIAN_POINT ( 'NONE',  ( 790.0220218866281812, -127.0999726633348672, 363.2186876482849129 ) ) ;
#10413 = CARTESIAN_POINT ( 'NONE',  ( 768.0187753319979720, -8.634602658420517329, 318.0580252608186242 ) ) ;
#10414 = EDGE_LOOP ( 'NONE', ( #3992, #31864, #20259, #413 ) ) ;
#10415 = CARTESIAN_POINT ( 'NONE',  ( 752.7379699480933368, -372.0090635724250205, -361.9858362298580232 ) ) ;
#10416 = CARTESIAN_POINT ( 'NONE',  ( -28.63011601220122415, -544.8427095258973623, -350.0000000000000000 ) ) ;
#10417 = CARTESIAN_POINT ( 'NONE',  ( 798.5707757039680246, -221.4636090269709428, 356.7845633553585003 ) ) ;
#10418 = CARTESIAN_POINT ( 'NONE',  ( 793.5525998758768083, -247.0999726633344835, 372.6845335610516941 ) ) ;
#10419 = CARTESIAN_POINT ( 'NONE',  ( 764.0069404352550464, -183.0783235625961538, 359.2566176426627180 ) ) ;
#10420 = CARTESIAN_POINT ( 'NONE',  ( 767.8955696845333705, -336.4527844766012095, -362.1676090361162323 ) ) ;
#10421 = CARTESIAN_POINT ( 'NONE',  ( 758.4439275373578084, -204.5545181178800931, -353.2243759319684386 ) ) ;
#10422 = CARTESIAN_POINT ( 'NONE',  ( 748.9653473494363425, -26.63460265842045871, 356.9462024416521331 ) ) ;
#10423 = CARTESIAN_POINT ( 'NONE',  ( 814.2001403089898304, -65.36187538569306810, 347.4397851343538264 ) ) ;
#10424 = DIRECTION ( 'NONE',  ( -1.000000000000000000, -0.000000000000000000, 0.000000000000000000 ) ) ;
#10425 = CARTESIAN_POINT ( 'NONE',  ( 763.2262854647970016, -416.6346026584192259, -309.2812353651462445 ) ) ;
#10426 = FACE_OUTER_BOUND ( 'NONE', #30621, .T. ) ;
#10427 = CARTESIAN_POINT ( 'NONE',  ( 802.2119215644370342, -342.0090635724251342, 367.5423716828165084 ) ) ;
#10428 = DIRECTION ( 'NONE',  ( 1.000000000000000000, 0.000000000000000000, 0.000000000000000000 ) ) ;
#10429 = CARTESIAN_POINT ( 'NONE',  ( 747.2067596250078623, -315.1800572038740711, 352.2312462859687230 ) ) ;
#10430 = CARTESIAN_POINT ( 'NONE',  ( 804.7487373415286811, -43.54369356751131903, -364.7487373415288516 ) ) ;
#10431 = CARTESIAN_POINT ( 'NONE',  ( 781.7834795799800531, -274.8164208402378108, -315.0636971347436202 ) ) ;
#10432 = CARTESIAN_POINT ( 'NONE',  ( 939.9999999999993179, -590.0000000000001137, 350.0000000000000000 ) ) ;
#10433 = APPLICATION_CONTEXT ( 'automotive_design' ) ;
#10434 = CARTESIAN_POINT ( 'NONE',  ( 771.2633955100217236, -383.9073299311466485, 363.4237431249939618 ) ) ;
#10435 = COLOUR_RGB ( '',0.7921568627450980005, 0.8196078431372548767, 0.9333333333333333481 ) ;
#10436 = CARTESIAN_POINT ( 'NONE',  ( 784.1219089521767955, -141.2817908451530400, 315.0488828828318333 ) ) ;
#10437 = CARTESIAN_POINT ( 'NONE',  ( 745.7194118038753459, -37.64542720878968396, -348.7631598425976449 ) ) ;
#10438 = CARTESIAN_POINT ( 'NONE',  ( 798.7617431975189675, -99.62377810805098477, -323.0428371773161871 ) ) ;
#10439 = CARTESIAN_POINT ( 'NONE',  ( 783.7566961878529810, -72.89650538077830788, 305.1792804349288417 ) ) ;
#10440 = CARTESIAN_POINT ( 'NONE',  ( 801.9419747391806368, -402.4527844766010389, 351.9812246680014027 ) ) ;
#10441 = LINE ( 'NONE', #34478, #15888 ) ;
#10442 = DIRECTION ( 'NONE',  ( 0.000000000000000000, 0.000000000000000000, 1.000000000000000000 ) ) ;
#10443 = CARTESIAN_POINT ( 'NONE',  ( 805.1927285166397041, 7.183579159761247723, -341.8018195045277707 ) ) ;
#10445 = ORIENTED_EDGE ( 'NONE', *, *, #41975, .T. ) ;
#10444 = CARTESIAN_POINT ( 'NONE',  ( 803.2186876482843445, -103.9874144716873161, -350.0220218866286928 ) ) ;
#10446 = CARTESIAN_POINT ( 'NONE',  ( 800.0135310231082713, -62.08914811296580183, -325.0180583372163028 ) ) ;
#10447 = CARTESIAN_POINT ( 'NONE',  ( 800.7704444035546203, -388.1692326535045936, -326.0291762391768771 ) ) ;
#10449 = CARTESIAN_POINT ( 'NONE',  ( 757.8323909638828582, -218.6346026584198228, 352.1044303154654358 ) ) ;
#10448 = CARTESIAN_POINT ( 'NONE',  ( 778.2165204200184689, -214.8164208402380666, 364.9363028652563230 ) ) ;
#10450 = CARTESIAN_POINT ( 'NONE',  ( 759.8311093483677041, -382.1692326535045936, -310.9282345327691814 ) ) ;
#10451 = FACE_OUTER_BOUND ( 'NONE', #24773, .T. ) ;
#10452 = ORIENTED_EDGE ( 'NONE', *, *, #16779, .T. ) ;
#10453 = CARTESIAN_POINT ( 'NONE',  ( 800.0135310231082713, -422.0891481129647218, 325.0180583372163028 ) ) ;
#10454 = EDGE_LOOP ( 'NONE', ( #9886, #8705, #24590, #5960 ) ) ;
#10455 = CARTESIAN_POINT ( 'NONE',  ( 772.4837098697144029, -239.3618753856924570, -374.5518280994205611 ) ) ;
#10456 = CARTESIAN_POINT ( 'NONE',  ( 804.7487373415286811, -139.5436935675110135, 364.7487373415288516 ) ) ;
#10457 = ORIENTED_EDGE ( 'NONE', *, *, #11411, .T. ) ;
#10459 = EDGE_CURVE ( 'NONE', #35164, #5266, #543, .T. ) ;
#10458 = CARTESIAN_POINT ( 'NONE',  ( 762.1405469898973024, -241.5436935675106440, -357.8594530101016176 ) ) ;
#10460 = ORIENTED_EDGE ( 'NONE', *, *, #13110, .T. ) ;
#10461 = CARTESIAN_POINT ( 'NONE',  ( 762.3223304703356007, -367.5436935675102745, -322.3223304703362828 ) ) ;
#10462 = CARTESIAN_POINT ( 'NONE',  ( 797.8594530101008786, -13.54369356751140785, -322.1405469898980982 ) ) ;
#10463 = CARTESIAN_POINT ( 'NONE',  ( 766.7756240680305382, -230.5328690171415076, 361.5560724626415663 ) ) ;
#10464 = LINE ( 'NONE', #24540, #4156 ) ;
#10465 = DIRECTION ( 'NONE',  ( 0.000000000000000000, 0.000000000000000000, -1.000000000000000000 ) ) ;
#10466 = EDGE_LOOP ( 'NONE', ( #2897, #28930, #10623, #28009 ) ) ;
#10467 = CARTESIAN_POINT ( 'NONE',  ( 774.6312213355099630, -23.36187538569318889, -364.6798772138717482 ) ) ;
#10468 = CARTESIAN_POINT ( 'NONE',  ( 989.9999999999992042, 249.9999999999998863, 350.0000000000000000 ) ) ;
#10469 = DIRECTION ( 'NONE',  ( 0.000000000000000000, 0.000000000000000000, 1.000000000000000000 ) ) ;
#10470 = ORIENTED_EDGE ( 'NONE', *, *, #21358, .F. ) ;
#10471 = CARTESIAN_POINT ( 'NONE',  ( 771.3260364891663130, -259.6454272087890445, -306.0683387631859773 ) ) ;
#10472 = VECTOR ( 'NONE', #26657, 1000.000000000000000 ) ;
#10473 = CARTESIAN_POINT ( 'NONE',  ( 749.5768839229115201, -132.5545181178802920, 358.0661480581553064 ) ) ;
#10475 = CARTESIAN_POINT ( 'NONE',  ( 785.3141322388236176, -237.7255117493289163, -364.4286716492789537 ) ) ;
#10474 = CARTESIAN_POINT ( 'NONE',  ( -928.0249999999991815, 154.9999999999998863, 339.9999999999999432 ) ) ;
#10476 = CARTESIAN_POINT ( 'NONE',  ( 775.9200461376533440, -407.8055962898681628, -315.3028492785443291 ) ) ;
#10477 = DIRECTION ( 'NONE',  ( 0.000000000000000000, -1.000000000000000000, 0.000000000000000000 ) ) ;
#10478 = DIRECTION ( 'NONE',  ( -1.000000000000000000, -0.000000000000000000, 0.000000000000000000 ) ) ;
#10479 = CARTESIAN_POINT ( 'NONE',  ( 766.0291762391763086, -106.9181544815167371, -360.7704444035551319 ) ) ;
#10480 = CARTESIAN_POINT ( 'NONE',  ( 783.7953271457878373, -392.1908817542432075, 375.1787889125761239 ) ) ;
#10481 = DIRECTION ( 'NONE',  ( -0.000000000000000000, 1.000000000000000000, -0.000000000000000000 ) ) ;
#10482 = CARTESIAN_POINT ( 'NONE',  ( 803.8556311672234642, 14.37622189194867417, -365.6418435158340117 ) ) ;
#10483 = CARTESIAN_POINT ( 'NONE',  ( 814.2001403089898304, -305.3618753856922581, -347.4397851343538264 ) ) ;
#10484 = DIRECTION ( 'NONE',  ( 0.000000000000000000, 0.000000000000000000, 1.000000000000000000 ) ) ;
#10485 = PLANE ( 'NONE',  #24624 ) ;
#10486 = CARTESIAN_POINT ( 'NONE',  ( 791.9812246680005501, -92.63460265842026331, -361.9419747391813189 ) ) ;
#10487 = CARTESIAN_POINT ( 'NONE',  ( 766.4474001241216001, -259.0999726633343698, 307.3154664389482491 ) ) ;
#10488 = CARTESIAN_POINT ( 'NONE',  ( 801.9858362298568863, -195.0783235625961538, -312.7379699480935642 ) ) ;
#10489 = CARTESIAN_POINT ( 'NONE',  ( 777.5031285880264704, -190.8164208402381234, 374.9108240113588408 ) ) ;
#10490 = CARTESIAN_POINT ( 'NONE',  ( 801.1904061080336987, -452.0891481129646650, -368.3070685750235498 ) ) ;
#10491 = DIRECTION ( 'NONE',  ( -0.000000000000000000, 1.000000000000000000, -0.000000000000000000 ) ) ;
#10492 = CARTESIAN_POINT ( 'NONE',  ( 755.0636971347428243, -292.2709662947831930, 341.7834795799807353 ) ) ;
#10493 = AXIS2_PLACEMENT_3D ( 'NONE', #31614, #4141, #25128 ) ;
#10494 = CARTESIAN_POINT ( 'NONE',  ( 775.8780910478218402, -81.28179084515319630, 364.9511171171680530 ) ) ;
#10495 = CARTESIAN_POINT ( 'NONE',  ( 794.9819416627830151, -444.9982390220554862, -319.9864689768909898 ) ) ;
#10496 = LINE ( 'NONE', #13980, #14421 ) ;
#10497 = DIRECTION ( 'NONE',  ( 0.000000000000000000, 1.000000000000000000, 0.000000000000000000 ) ) ;
#10499 = CARTESIAN_POINT ( 'NONE',  ( 797.6776695296629214, -331.5436935675104451, 357.6776695296636603 ) ) ;
#10498 = CARTESIAN_POINT ( 'NONE',  ( 755.8398074228967971, -139.4419599262326699, 333.4516893846970333 ) ) ;
#10500 = ORIENTED_EDGE ( 'NONE', *, *, #21278, .T. ) ;
#10501 = CARTESIAN_POINT ( 'NONE',  ( 803.8651313633788504, -245.2601417444141987, -332.4468031744301015 ) ) ;
#10502 = CARTESIAN_POINT ( 'NONE',  ( 759.9864689768902508, -98.08914811296568814, 354.9819416627836404 ) ) ;
#10503 = CARTESIAN_POINT ( 'NONE',  ( 768.8385539511368734, -287.2601417444140566, -306.4236121716840557 ) ) ;
#10504 = CARTESIAN_POINT ( 'NONE',  ( 939.9999999999993179, 62.79977829742944095, -207.3621835540873235 ) ) ;
#10505 = CARTESIAN_POINT ( 'NONE',  ( 761.9338519418445230, -422.5328690171408539, 370.4231160770881957 ) ) ;
#10506 = ORIENTED_EDGE ( 'NONE', *, *, #7494, .T. ) ;
#10507 = CARTESIAN_POINT ( 'NONE',  ( 802.1676090361156639, -302.6346026584196238, 327.8955696845344505 ) ) ;
#10508 = CARTESIAN_POINT ( 'NONE',  ( 786.6156483768007774, -49.44195992623295410, -315.5913626894246136 ) ) ;
#10509 = CARTESIAN_POINT ( 'NONE',  ( 768.0187753319979720, -152.6346026584200786, -318.0580252608186242 ) ) ;
#10510 = CARTESIAN_POINT ( 'NONE',  ( 764.8639956371174549, -200.0891481129653187, -319.7806653035542013 ) ) ;
#10511 = CARTESIAN_POINT ( 'NONE',  ( 759.9864689768902508, -410.0891481129647218, 354.9819416627836404 ) ) ;
#10512 = EDGE_CURVE ( 'NONE', #40012, #29996, #12978, .T. ) ;
#10513 = CARTESIAN_POINT ( 'NONE',  ( 800.9747183278959710, -132.9982390220564810, -311.9810565676471583 ) ) ;
#10514 = CARTESIAN_POINT ( 'NONE',  ( 755.0636971347428243, -100.2709662947838609, -341.7834795799807353 ) ) ;
#10515 = ORIENTED_EDGE ( 'NONE', *, *, #28565, .F. ) ;
#10516 = CARTESIAN_POINT ( 'NONE',  ( 766.0291762391763086, -394.9181544815158418, -360.7704444035551319 ) ) ;
#10518 = CARTESIAN_POINT ( 'NONE',  ( 780.5236548040995785, -428.7363362996975980, 314.9735926884559944 ) ) ;
#10517 = CARTESIAN_POINT ( 'NONE',  ( 762.1405469898971887, -121.5436935675110419, 357.8594530101015607 ) ) ;
#10519 = CARTESIAN_POINT ( 'NONE',  ( 754.8983024940795303, -114.8965053807782226, 336.9254006560228163 ) ) ;
#10522 = CARTESIAN_POINT ( 'NONE',  ( 756.1443688327750579, -405.6237781080500326, 314.3581564841659315 ) ) ;
#10521 = DIRECTION ( 'NONE',  ( -0.000000000000000000, 1.000000000000000000, -0.000000000000000000 ) ) ;
#10520 = FACE_BOUND ( 'NONE', #11836, .T. ) ;
#10523 = VERTEX_POINT ( 'NONE', #11626 ) ;
#10524 = CARTESIAN_POINT ( 'NONE',  ( 800.9840315886518738, -364.9181544815158986, -354.1144889064786412 ) ) ;
#10525 = CARTESIAN_POINT ( 'NONE',  ( 762.3223304703356007, -367.5436935675102745, -322.3223304703362828 ) ) ;
#10526 = AXIS2_PLACEMENT_3D ( 'NONE', #8222, #22291, #32943 ) ;
#10527 = CARTESIAN_POINT ( 'NONE',  ( 802.2119215644370342, -174.0090635724256742, -367.5423716828165084 ) ) ;
#10528 = CARTESIAN_POINT ( 'NONE',  ( 807.2620300519052989, -48.00906357242602951, 318.0141637701419768 ) ) ;
#10530 = CARTESIAN_POINT ( 'NONE',  ( -338.8365100919713200, 260.0000000000001137, -199.9999999999917861 ) ) ;
#10529 = CARTESIAN_POINT ( 'NONE',  ( 919.9999999999993179, 154.9999999999998863, -350.0000000000000000 ) ) ;
#10531 = CARTESIAN_POINT ( 'NONE',  ( 765.8855110935204493, -286.1692326535048778, -319.0159684113471599 ) ) ;
#10532 = CARTESIAN_POINT ( 'NONE',  ( -879.9999999999992042, 240.0000000000002274, -244.9999999999999716 ) ) ;
#10533 = CARTESIAN_POINT ( 'NONE',  ( 791.0478386215596629, -165.8272453906074873, -306.7653713866226326 ) ) ;
#10534 = DIRECTION ( 'NONE',  ( -0.000000000000000000, -0.000000000000000000, 1.000000000000000000 ) ) ;
#10535 = CARTESIAN_POINT ( 'NONE',  ( 180.7583438952258348, 394.6698570112193920, -274.9999999999999432 ) ) ;
#10536 = CARTESIAN_POINT ( 'NONE',  ( 790.0220218866281812, -367.0999726633342561, 363.2186876482849129 ) ) ;
#10537 = CARTESIAN_POINT ( 'NONE',  ( 815.3608509340175488, -338.7363362996978822, 341.2497674668889545 ) ) ;
#10538 = CARTESIAN_POINT ( 'NONE',  ( 810.7187646348534145, -210.4527844766016926, -356.7737145352016341 ) ) ;
#10539 = DIRECTION ( 'NONE',  ( 1.644774851296528363E-16, -1.000000000000000000, 0.000000000000000000 ) ) ;
#10540 = FACE_OUTER_BOUND ( 'NONE', #7526, .T. ) ;
#10541 = CARTESIAN_POINT ( 'NONE',  ( 814.2805881961230625, -145.6454272087893287, 331.2368401574024119 ) ) ;
#10542 = CARTESIAN_POINT ( 'NONE',  ( 751.2241431872005251, -112.1692326535054889, -359.9636004259367610 ) ) ;
#10543 = CARTESIAN_POINT ( 'NONE',  ( 747.2067596250078623, -339.1800572038740142, -352.2312462859687230 ) ) ;
#10544 = DIRECTION ( 'NONE',  ( -1.000000000000000000, 0.000000000000000000, 0.000000000000000000 ) ) ;
#10545 = DIRECTION ( 'NONE',  ( -0.000000000000000000, 1.000000000000000000, -0.000000000000000000 ) ) ;
#10546 = CARTESIAN_POINT ( 'NONE',  ( 759.9864689768902508, -170.0891481129654608, 354.9819416627836404 ) ) ;
#10547 = EDGE_LOOP ( 'NONE', ( #22370, #23386, #17959, #41159 ) ) ;
#10548 = CARTESIAN_POINT ( 'NONE',  ( 744.6391490659812007, -446.7363362996975980, 338.7502325331110455 ) ) ;
#10549 = CARTESIAN_POINT ( 'NONE',  ( 814.8230680027162407, -389.8055962898682765, -333.7305795820267917 ) ) ;
#10550 = CARTESIAN_POINT ( 'NONE',  ( 767.7687537140311633, -143.9073299311473590, -372.7932403749916830 ) ) ;
#10551 = EDGE_CURVE ( 'NONE', #14381, #16198, #21100, .T. ) ;
#10552 = CARTESIAN_POINT ( 'NONE',  ( 751.6929314249748586, -438.9982390220553157, -318.8095938919659034 ) ) ;
#10553 = CARTESIAN_POINT ( 'NONE',  ( 779.9999999999992042, -462.9681489794448339, -339.9999999999999432 ) ) ;
#10554 = CARTESIAN_POINT ( 'NONE',  ( 803.8556311672234642, -9.623778108051251223, 365.6418435158340117 ) ) ;
#10555 = EDGE_LOOP ( 'NONE', ( #41763, #44941, #21271, #4285 ) ) ;
#10556 = EDGE_CURVE ( 'NONE', #791, #17477, #4861, .T. ) ;
#10557 = VECTOR ( 'NONE', #4078, 1000.000000000000000 ) ;
#10558 = CARTESIAN_POINT ( 'NONE',  ( 801.9858362298568863, -195.0783235625961538, -312.7379699480935642 ) ) ;
#10559 = LINE ( 'NONE', #44999, #26268 ) ;
#10560 = CARTESIAN_POINT ( 'NONE',  ( 813.2346286133761168, -293.2601417444139429, 328.9521613784389160 ) ) ;
#10561 = CARTESIAN_POINT ( 'NONE',  ( 803.6646147819162707, -137.9073299311473875, 348.8264449731211130 ) ) ;
#10562 = CARTESIAN_POINT ( 'NONE',  ( 779.9999999999992042, 126.4563064324884465, -370.0000000000000568 ) ) ;
#10563 = ORIENTED_EDGE ( 'NONE', *, *, #7440, .T. ) ;
#10564 = ADVANCED_FACE ( 'NONE', ( #25704 ), #22012, .F. ) ;
#10565 = CARTESIAN_POINT ( 'NONE',  ( 755.0636971347428243, -316.2709662947832499, 341.7834795799807353 ) ) ;
#10566 = EDGE_CURVE ( 'NONE', #3123, #20161, #16672, .T. ) ;
#10567 = CARTESIAN_POINT ( 'NONE',  ( 745.7998596910086917, -5.361875385693257279, -332.5602148656461168 ) ) ;
#10568 = CARTESIAN_POINT ( 'NONE',  ( 789.4635523819913487, -451.6789215907663788, 363.3011154535611809 ) ) ;
#10569 = EDGE_LOOP ( 'NONE', ( #2212, #17051, #4271, #3809 ) ) ;
#10570 = ADVANCED_BREP_SHAPE_REPRESENTATION ( '', ( #33039, #26858 ), #7704 ) ;
#10571 = CARTESIAN_POINT ( 'NONE',  ( 752.7379699480933368, -420.0090635724249069, -361.9858362298580232 ) ) ;
#10572 = ORIENTED_EDGE ( 'NONE', *, *, #37945, .F. ) ;
#10573 = APPLICATION_PROTOCOL_DEFINITION ( 'draft international standard', 'automotive_design', 1998, #18153 ) ;
#10574 = VECTOR ( 'NONE', #29706, 1000.000000000000000 ) ;
#10575 = CARTESIAN_POINT ( 'NONE',  ( 757.8323909638827445, -26.63460265842045871, 352.1044303154654358 ) ) ;
#10576 = CARTESIAN_POINT ( 'NONE',  ( 788.8264449731200330, -261.1800572038741848, -363.6646147819171233 ) ) ;
#10578 = CARTESIAN_POINT ( 'NONE',  ( 783.7566961878529810, -288.8965053807775121, 305.1792804349288417 ) ) ;
#10577 = CARTESIAN_POINT ( 'NONE',  ( 755.2512626584698410, -343.5436935675103314, 315.2512626584710915 ) ) ;
#10579 = CARTESIAN_POINT ( 'NONE',  ( 814.8230680027162407, -77.80559628986920018, 333.7305795820267917 ) ) ;
#10580 = CARTESIAN_POINT ( 'NONE',  ( 766.0291762391763086, -250.9181544815163534, -360.7704444035551319 ) ) ;
#10581 = CARTESIAN_POINT ( 'NONE',  ( 764.8639956371174549, -248.0891481129651481, -319.7806653035542013 ) ) ;
#10582 = DIRECTION ( 'NONE',  ( 0.000000000000000000, -1.000000000000000000, 0.000000000000000000 ) ) ;
#10583 = CARTESIAN_POINT ( 'NONE',  ( 778.1981804954714335, -106.2709662947838467, -314.8072714833589885 ) ) ;
#10584 = EDGE_CURVE ( 'NONE', #518, #38954, #6385, .T. ) ;
#10585 = CARTESIAN_POINT ( 'NONE',  ( 785.3687786644884454, -251.3618753856923149, 315.3201227861279676 ) ) ;
#10586 = VERTEX_POINT ( 'NONE', #39124 ) ;
#10587 = CARTESIAN_POINT ( 'NONE',  ( 755.2512626584698410, -391.5436935675101608, 315.2512626584710915 ) ) ;
#10589 = DIRECTION ( 'NONE',  ( 0.000000000000000000, 0.000000000000000000, -1.000000000000000000 ) ) ;
#10588 = DIRECTION ( 'NONE',  ( 1.000000000000000000, -0.000000000000000000, -0.000000000000000000 ) ) ;
#10590 = EDGE_CURVE ( 'NONE', #13375, #4510, #7475, .T. ) ;
#10591 = CARTESIAN_POINT ( 'NONE',  ( 762.1177392798416577, -42.55451811788057626, -309.8865473780659272 ) ) ;
#10592 = LINE ( 'NONE', #21445, #30012 ) ;
#10593 = DIRECTION ( 'NONE',  ( 0.000000000000000000, -0.000000000000000000, -1.000000000000000000 ) ) ;
#10594 = CARTESIAN_POINT ( 'NONE',  ( 755.3028492785439312, -255.2817908451526705, 335.9200461376539693 ) ) ;
#10595 = CARTESIAN_POINT ( 'NONE',  ( 774.6858677611749044, -129.7255117493292289, 315.5713283507209894 ) ) ;
#10596 = EDGE_LOOP ( 'NONE', ( #11366, #2720 ) ) ;
#10597 = CARTESIAN_POINT ( 'NONE',  ( 793.9708237608222134, -22.91815448151701062, -319.2295555964448681 ) ) ;
#10598 = AXIS2_PLACEMENT_3D ( 'NONE', #22183, #7025, #28033 ) ;
#10599 = CARTESIAN_POINT ( 'NONE',  ( 813.1304606946831655, -113.9073299311474585, -352.3570229623691716 ) ) ;
#10600 = AXIS2_PLACEMENT_3D ( 'NONE', #22623, #44100, #12464 ) ;
#10601 = CARTESIAN_POINT ( 'NONE',  ( 773.3843516231979720, -277.4419599262322436, 364.4086373105754433 ) ) ;
#10602 = FACE_OUTER_BOUND ( 'NONE', #657, .T. ) ;
#10603 = CARTESIAN_POINT ( 'NONE',  ( 802.2119215644370342, -30.00906357242607925, 367.5423716828165084 ) ) ;
#10604 = CARTESIAN_POINT ( 'NONE',  ( 787.5162901302840055, -251.3618753856923149, -305.4481719005792684 ) ) ;
#10605 = CARTESIAN_POINT ( 'NONE',  ( 771.2633955100217236, -95.90732993114751537, 363.4237431249939618 ) ) ;
#10606 = DIRECTION ( 'NONE',  ( 0.000000000000000000, 0.000000000000000000, 1.000000000000000000 ) ) ;
#10607 = EDGE_CURVE ( 'NONE', #9887, #27562, #28723, .T. ) ;
#10608 = CARTESIAN_POINT ( 'NONE',  ( 751.2241431872005251, -280.1692326535049347, -359.9636004259367610 ) ) ;
#10609 = EDGE_CURVE ( 'NONE', #14297, #16495, #39344, .T. ) ;
#10610 = CARTESIAN_POINT ( 'NONE',  ( 754.3581564841646241, -449.4636090269702322, 316.1443688327762516 ) ) ;
#10611 = CARTESIAN_POINT ( 'NONE',  ( 782.5225473063381969, -334.2709662947829656, -375.2698199232970637 ) ) ;
#10612 = FACE_BOUND ( 'NONE', #1586, .T. ) ;
#10613 = CARTESIAN_POINT ( 'NONE',  ( 790.8726784830453198, -346.7146871989592682, 362.5472867521010585 ) ) ;
#10614 = CARTESIAN_POINT ( 'NONE',  ( 751.6929314249750860, -30.99823902205680781, 318.8095938919659034 ) ) ;
#10615 = CARTESIAN_POINT ( 'NONE',  ( 805.1927285166397041, -376.8164208402375834, -341.8018195045277707 ) ) ;
#10616 = EDGE_CURVE ( 'NONE', #5298, #14461, #32639, .T. ) ;
#10617 = CARTESIAN_POINT ( 'NONE',  ( 760.5453621957607311, -45.07832356259660145, 323.8424801807151425 ) ) ;
#10618 = CARTESIAN_POINT ( 'NONE',  ( 774.6858677611749044, -201.7255117493290015, -315.5713283507209894 ) ) ;
#10619 = CARTESIAN_POINT ( 'NONE',  ( 795.6651683502461765, -34.71468719896025590, -371.3240766477733814 ) ) ;
#10620 = CARTESIAN_POINT ( 'NONE',  ( 749.8865473780648472, -212.5328690171415076, 322.1177392798429082 ) ) ;
#10621 = CARTESIAN_POINT ( 'NONE',  ( 781.8018195045267476, -22.27096629478410605, 365.1927285166407273 ) ) ;
#10622 = CARTESIAN_POINT ( 'NONE',  ( 780.5290396650775619, -372.3510508353228374, 365.2837595273619513 ) ) ;
#10623 = ORIENTED_EDGE ( 'NONE', *, *, #40528, .T. ) ;
#10624 = CARTESIAN_POINT ( 'NONE',  ( 794.1144889064781864, -202.1692326535051905, -360.9840315886528401 ) ) ;
#10625 = CARTESIAN_POINT ( 'NONE',  ( 804.9363028652555840, -184.2709662947835909, 338.2165204200192079 ) ) ;
#10626 = CARTESIAN_POINT ( 'NONE',  ( 759.8311093483677041, -46.16923265350568784, -310.9282345327691814 ) ) ;
#10627 = CARTESIAN_POINT ( 'NONE',  ( 788.8264449731201466, -333.1800572038740142, 363.6646147819170665 ) ) ;
#10628 = DIRECTION ( 'NONE',  ( -1.000000000000000000, -0.000000000000000000, 0.000000000000000000 ) ) ;
#10629 = AXIS2_PLACEMENT_3D ( 'NONE', #32436, #25492, #42820 ) ;
#10630 = EDGE_LOOP ( 'NONE', ( #39870, #1360, #22832, #19224 ) ) ;
#10631 = CARTESIAN_POINT ( 'NONE',  ( 754.9735926884551418, -42.35105083532388193, 340.5236548041000333 ) ) ;
#10632 = CARTESIAN_POINT ( 'NONE',  ( 745.1792804349281596, -302.1908817542433781, -343.7566961878542884 ) ) ;
#10633 = CARTESIAN_POINT ( 'NONE',  ( 801.1904061080338124, -260.0891481129650629, 368.3070685750236066 ) ) ;
#10634 = CARTESIAN_POINT ( 'NONE',  ( 761.9338519418445230, -14.53286901714214707, 370.4231160770881957 ) ) ;
#10635 = CARTESIAN_POINT ( 'NONE',  ( 754.7162404726377645, -158.7363362996984222, -339.4709603349214717 ) ) ;
#10636 = CARTESIAN_POINT ( 'NONE',  ( 785.3141322388236176, -141.7255117493291721, -364.4286716492789537 ) ) ;
#10637 = CARTESIAN_POINT ( 'NONE',  ( 758.0580252608178853, -342.4527844766013231, -328.0187753319985404 ) ) ;
#10638 = ORIENTED_EDGE ( 'NONE', *, *, #3597, .F. ) ;
#10639 = CARTESIAN_POINT ( 'NONE',  ( 792.2312462859673587, -275.9073299311469896, 307.2067596250082602 ) ) ;
#10640 = VECTOR ( 'NONE', #23044, 999.9999999999998863 ) ;
#10641 = CARTESIAN_POINT ( 'NONE',  ( -468.8365100919714337, 256.5000000000001705, -199.9999999999908766 ) ) ;
#10642 = CARTESIAN_POINT ( 'NONE',  ( 786.6156483768007774, -337.4419599262319593, 315.5913626894246136 ) ) ;
#10643 = CARTESIAN_POINT ( 'NONE',  ( 265.7583438952258916, 290.0000000000001137, -244.9999999999999716 ) ) ;
#10644 = AXIS2_PLACEMENT_3D ( 'NONE', #21127, #28512, #21351 ) ;
#10645 = CARTESIAN_POINT ( 'NONE',  ( 783.0745993439762742, -152.1908817542438612, 365.1016975059196739 ) ) ;
#10646 = CARTESIAN_POINT ( 'NONE',  ( 755.0636971347428243, -4.270966294784170003, 341.7834795799807353 ) ) ;
#10647 = ORIENTED_EDGE ( 'NONE', *, *, #12591, .F. ) ;
#10648 = CARTESIAN_POINT ( 'NONE',  ( 811.3240766477731540, -388.3726999360613945, -355.6651683502462902 ) ) ;
#10649 = CARTESIAN_POINT ( 'NONE',  ( 754.9967657858570647, -1.543693567511449594, -365.0032342141425943 ) ) ;
#10650 = CARTESIAN_POINT ( 'NONE',  ( 812.3518521366052028, -241.0999726633345119, 326.5853460496235243 ) ) ;
#10651 = CARTESIAN_POINT ( 'NONE',  ( 796.7845633553578182, -369.6237781080500895, 358.5707757039688204 ) ) ;
#10652 = CARTESIAN_POINT ( 'NONE',  ( 766.7756240680305382, -182.5328690171416497, 361.5560724626415663 ) ) ;
#10653 = CARTESIAN_POINT ( 'NONE',  ( 800.2193346964447755, -378.9982390220555999, -355.1360043628815788 ) ) ;
#10654 = CARTESIAN_POINT ( 'NONE',  ( 790.9844846989617508, -454.3726999360611103, 317.2208543904092721 ) ) ;
#10655 = CARTESIAN_POINT ( 'NONE',  ( 914.9999999999992042, 99.99999999999984368, -360.0000000000000000 ) ) ;
#10656 = CARTESIAN_POINT ( 'NONE',  ( 755.1538015810308480, -206.1908817542437191, -343.0433043558613804 ) ) ;
#10657 = VECTOR ( 'NONE', #43929, 1000.000000000000000 ) ;
#10658 = CARTESIAN_POINT ( 'NONE',  ( 805.0032342141412300, -13.54369356751140785, 314.9967657858571783 ) ) ;
#10659 = DIRECTION ( 'NONE',  ( -1.000000000000000000, -0.000000000000000000, 0.000000000000000000 ) ) ;
#10660 = CARTESIAN_POINT ( 'NONE',  ( 758.8095938919644823, -416.0891481129646650, -311.6929314249762797 ) ) ;
#10661 = VECTOR ( 'NONE', #11122, 1000.000000000000000 ) ;
#10662 = DIRECTION ( 'NONE',  ( 0.000000000000000000, 0.000000000000000000, -1.000000000000000000 ) ) ;
#10663 = CARTESIAN_POINT ( 'NONE',  ( 745.5313806188320314, -351.2817908451523294, 333.7943932421247268 ) ) ;
#10664 = CYLINDRICAL_SURFACE ( 'NONE', #10236, 12.00000000000001066 ) ;
#10665 = CARTESIAN_POINT ( 'NONE',  ( 754.9967657858570647, -313.5436935675102745, 365.0032342141425374 ) ) ;
#10666 = CARTESIAN_POINT ( 'NONE',  ( 767.7687537140311633, -47.90732993114767169, -372.7932403749916830 ) ) ;
#10667 = CARTESIAN_POINT ( 'NONE',  ( 795.1360043628807261, -284.0891481129650629, -360.2193346964456282 ) ) ;
#10668 = CARTESIAN_POINT ( 'NONE',  ( 51.16348990802859475, 260.0000000000000568, -199.9999999999945146 ) ) ;
#10669 = CARTESIAN_POINT ( 'NONE',  ( 768.0187753319979720, -416.6346026584192259, 318.0580252608186242 ) ) ;
#10670 = CARTESIAN_POINT ( 'NONE',  ( 801.5560724626406000, -168.5545181178802352, 326.7756240680316182 ) ) ;
#10671 = CARTESIAN_POINT ( 'NONE',  ( 748.6759233522253680, -16.37269993606248519, -324.3348316497537098 ) ) ;
#10672 = CARTESIAN_POINT ( 'NONE',  ( 783.0433043558608688, -72.89650538077830788, -315.1538015810313027 ) ) ;
#10673 = CARTESIAN_POINT ( 'NONE',  ( 746.7653713866222915, -113.2601417444145682, 351.0478386215610271 ) ) ;
#10674 = CARTESIAN_POINT ( 'NONE',  ( 767.8955696845334842, -408.4527844766009821, 362.1676090361161755 ) ) ;
#10675 = CIRCLE ( 'NONE', #31345, 30.00000000000008171 ) ;
#10676 = DIRECTION ( 'NONE',  ( 0.000000000000000000, -0.6594541114781790059, -0.7517448203044204691 ) ) ;
#10677 = CARTESIAN_POINT ( 'NONE',  ( 778.2165204200184689, 1.183579159761269040, -364.9363028652563230 ) ) ;
#10678 = ORIENTED_EDGE ( 'NONE', *, *, #41357, .T. ) ;
#10679 = CARTESIAN_POINT ( 'NONE',  ( 803.6646147819161570, -89.90732993114750116, -348.8264449731210561 ) ) ;
#10680 = VECTOR ( 'NONE', #24349, 1000.000000000000000 ) ;
#10681 = CARTESIAN_POINT ( 'NONE',  ( 795.9930595647434757, -411.0783235625954717, -320.7433823573372820 ) ) ;
#10683 = CARTESIAN_POINT ( 'NONE',  ( 759.9864689768902508, -218.0891481129653187, 354.9819416627836404 ) ) ;
#10682 = CARTESIAN_POINT ( 'NONE',  ( 755.3201227861273992, -219.7255117493289447, 345.3687786644892981 ) ) ;
#10684 = CARTESIAN_POINT ( 'NONE',  ( 798.0661480581538854, -386.5328690171409676, -309.5768839229118043 ) ) ;
#10685 = CARTESIAN_POINT ( 'NONE',  ( 763.0537975583475827, -0.4527844766023628176, 371.0346526505627480 ) ) ;
#10686 = DIRECTION ( 'NONE',  ( 1.000000000000000000, 0.000000000000000000, 0.000000000000000000 ) ) ;
#10687 = ORIENTED_EDGE ( 'NONE', *, *, #40248, .F. ) ;
#10688 = CARTESIAN_POINT ( 'NONE',  ( 759.7806653035534055, -438.9982390220553157, 324.8639956371180801 ) ) ;
#10689 = ORIENTED_EDGE ( 'NONE', *, *, #12306, .T. ) ;
#10690 = CARTESIAN_POINT ( 'NONE',  ( 767.6429770376289525, -249.1800572038742416, -306.8695393053162093 ) ) ;
#10691 = CARTESIAN_POINT ( 'NONE',  ( 814.9108240113580450, -160.2709662947836762, 337.5031285880265273 ) ) ;
#10692 = CLOSED_SHELL ( 'NONE', ( #34665, #21512, #44723, #9179, #42193, #24287, #26631, #36769, #45562, #33708, #10332, #36262, #26653, #15081, #14248, #31158, #29498, #21901, #11437, #38, #37254, #38506, #29769, #767, #5814, #28002, #21517, #39693, #15643, #42762, #39136, #19695, #17082, #31933, #32949, #37413, #12026, #41653, #26383, #45627, #26718, #40817, #29218, #1589, #38741, #15626, #15679, #45490, #913, #44503, #40448, #35661, #28676, #42262 ) ) ;
#10693 = CARTESIAN_POINT ( 'NONE',  ( 759.2295555964440155, -376.1692326535046504, 353.9708237608231229 ) ) ;
#10694 = VERTEX_POINT ( 'NONE', #15086 ) ;
#10695 = CARTESIAN_POINT ( 'NONE',  ( 768.0187753319979720, -248.6346026584197659, -318.0580252608186242 ) ) ;
#10696 = CIRCLE ( 'NONE', #18094, 10.00000000000000888 ) ;
#10697 = VERTEX_POINT ( 'NONE', #33099 ) ;
#10698 = CARTESIAN_POINT ( 'NONE',  ( 756.3353852180819104, -365.9073299311465917, -331.1735550268788302 ) ) ;
#10699 = CARTESIAN_POINT ( 'NONE',  ( 759.9864689768902508, -26.08914811296592262, -354.9819416627836404 ) ) ;
#10700 = VECTOR ( 'NONE', #35362, 1000.000000000000000 ) ;
#10701 = CARTESIAN_POINT ( 'NONE',  ( 772.3691319403857278, -239.2601417444141987, 315.8894580844506663 ) ) ;
#10702 = DIRECTION ( 'NONE',  ( 1.000000000000000000, -0.000000000000000000, -0.000000000000000000 ) ) ;
#10703 = CARTESIAN_POINT ( 'NONE',  ( 701.1634899080286232, 258.0939999999999372, -206.1189999999990334 ) ) ;
#10704 = ORIENTED_EDGE ( 'NONE', *, *, #21591, .F. ) ;
#10705 = CARTESIAN_POINT ( 'NONE',  ( 756.5762568750052424, -3.180057203875080063, -348.7366044899774238 ) ) ;
#10706 = PLANE ( 'NONE',  #42521 ) ;
#10707 = ORIENTED_EDGE ( 'NONE', *, *, #30371, .T. ) ;
#10708 = CARTESIAN_POINT ( 'NONE',  ( 744.6391490659812007, -278.7363362996980527, -338.7502325331110455 ) ) ;
#10709 = VECTOR ( 'NONE', #24852, 1000.000000000000000 ) ;
#10710 = CARTESIAN_POINT ( 'NONE',  ( 793.5525998758768083, -151.0999726633347677, 372.6845335610516941 ) ) ;
#10711 = CIRCLE ( 'NONE', #5554, 8.000000000000007105 ) ;
#10713 = CARTESIAN_POINT ( 'NONE',  ( 795.1360043628807261, -260.0891481129650060, -360.2193346964456282 ) ) ;
#10712 = LINE ( 'NONE', #38912, #34197 ) ;
#10714 = CARTESIAN_POINT ( 'NONE',  ( 786.6156483768007774, -409.4419599262317320, -315.5913626894246136 ) ) ;
#10715 = CARTESIAN_POINT ( 'NONE',  ( 1238.921997096861332, 430.0000000000002842, -320.0000000000000568 ) ) ;
#10716 = CARTESIAN_POINT ( 'NONE',  ( 757.0176451133909268, -109.0999726633349241, -349.9200121543848354 ) ) ;
#10717 = VECTOR ( 'NONE', #22924, 1000.000000000000000 ) ;
#10718 = AXIS2_PLACEMENT_3D ( 'NONE', #10416, #3263, #40751 ) ;
#10719 = CARTESIAN_POINT ( 'NONE',  ( 752.7379699480933368, -372.0090635724250205, 361.9858362298580232 ) ) ;
#10720 = CARTESIAN_POINT ( 'NONE',  ( 927.9999999999992042, 154.9999999999998863, -360.0000000000000000 ) ) ;
#10721 = CARTESIAN_POINT ( 'NONE',  ( 768.8385539511368734, 0.7398582555850804487, -306.4236121716840557 ) ) ;
#10722 = CARTESIAN_POINT ( 'NONE',  ( 808.3070685750232087, -306.9982390220558841, -361.1904061080339829 ) ) ;
#10723 = CARTESIAN_POINT ( 'NONE',  ( -26.63011601220122060, -512.9681489794448908, -350.0000000000000000 ) ) ;
#10724 = CARTESIAN_POINT ( 'NONE',  ( 774.6858677611749044, -9.725511749329603717, 315.5713283507209894 ) ) ;
#10725 = CARTESIAN_POINT ( 'NONE',  ( 774.6312213355099630, -95.36187538569294020, -364.6798772138717482 ) ) ;
#10726 = CARTESIAN_POINT ( 'NONE',  ( 814.8207195650702488, -266.1908817542435486, 336.2433038121456548 ) ) ;
#10727 = CARTESIAN_POINT ( 'NONE',  ( 771.2368401574024119, -205.4419599262324425, -374.2805881961240857 ) ) ;
#10728 = CARTESIAN_POINT ( 'NONE',  ( 813.1304606946830518, -209.9073299311470748, 352.3570229623690580 ) ) ;
#10729 = CARTESIAN_POINT ( 'NONE',  ( 791.0478386215596629, 2.172754609392001601, -306.7653713866226326 ) ) ;
#10730 = FACE_OUTER_BOUND ( 'NONE', #45277, .T. ) ;
#10731 = CARTESIAN_POINT ( 'NONE',  ( 778.2165204200184689, -286.8164208402378677, 364.9363028652563230 ) ) ;
#10732 = EDGE_CURVE ( 'NONE', #29534, #44896, #5643, .T. ) ;
#10733 = CARTESIAN_POINT ( 'NONE',  ( 801.5560724626406000, -96.55451811788039151, 326.7756240680316182 ) ) ;
#10734 = CARTESIAN_POINT ( 'NONE',  ( 784.0799538623451781, 12.19440371013049784, -364.6971507214555572 ) ) ;
#10735 = VECTOR ( 'NONE', #27395, 1000.000000000000000 ) ;
#10736 = CARTESIAN_POINT ( 'NONE',  ( -786.4999999999993179, -513.1383975375929367, -349.9999999999999432 ) ) ;
#10737 = CARTESIAN_POINT ( 'NONE',  ( -468.8365100919714337, 258.0940000000001646, -206.1189999999908764 ) ) ;
#10739 = CARTESIAN_POINT ( 'NONE',  ( 803.4237431249931660, -375.1800572038739574, 331.2633955100225194 ) ) ;
#10738 = CARTESIAN_POINT ( 'NONE',  ( 772.3691319403857278, -119.2601417444145397, 315.8894580844506663 ) ) ;
#10740 = VERTEX_POINT ( 'NONE', #22225 ) ;
#10741 = CARTESIAN_POINT ( 'NONE',  ( 755.0488828828309806, -281.8055962898686175, -344.1219089521771934 ) ) ;
#10742 = CARTESIAN_POINT ( 'NONE',  ( 781.7834795799800531, -82.81642084023846451, 315.0636971347436202 ) ) ;
#10743 = CARTESIAN_POINT ( 'NONE',  ( 752.7379699480933368, -396.0090635724249637, 361.9858362298580232 ) ) ;
#10744 = CARTESIAN_POINT ( 'NONE',  ( 801.9858362298568863, -291.0783235625957559, -312.7379699480935642 ) ) ;
#10745 = PLANE ( 'NONE',  #42291 ) ;
#10746 = CARTESIAN_POINT ( 'NONE',  ( 791.1614460488616487, -419.2601417444136587, 373.5763878283158874 ) ) ;
#10747 = ORIENTED_EDGE ( 'NONE', *, *, #40559, .F. ) ;
#10748 = CARTESIAN_POINT ( 'NONE',  ( 754.8072714833581358, -340.8164208402376971, 338.1981804954720587 ) ) ;
#10749 = CIRCLE ( 'NONE', #26991, 10.00000000000000888 ) ;
#10750 = CARTESIAN_POINT ( 'NONE',  ( 757.2208543904082489, -40.71468719896024879, -350.9844846989624330 ) ) ;
#10751 = CARTESIAN_POINT ( 'NONE',  ( 792.1044303154645831, -156.4527844766018916, -317.8323909638837677 ) ) ;
#10752 = CARTESIAN_POINT ( 'NONE',  ( 755.0636971347428243, -220.2709662947834772, -341.7834795799807353 ) ) ;
#10753 = CARTESIAN_POINT ( 'NONE',  ( 800.0135310231082713, -398.0891481129647218, 325.0180583372163028 ) ) ;
#10754 = CIRCLE ( 'NONE', #11553, 2.749999999999919176 ) ;
#10755 = CARTESIAN_POINT ( 'NONE',  ( 813.1304606946830518, -161.9073299311472454, -352.3570229623690580 ) ) ;
#10756 = ORIENTED_EDGE ( 'NONE', *, *, #24413, .F. ) ;
#10757 = CARTESIAN_POINT ( 'NONE',  ( 800.0135310231082713, -134.0891481129655745, -325.0180583372163028 ) ) ;
#10758 = ORIENTED_EDGE ( 'NONE', *, *, #31393, .F. ) ;
#10759 = CARTESIAN_POINT ( 'NONE',  ( 757.0176451133909268, -397.0999726633340288, -349.9200121543848354 ) ) ;
#10761 = CARTESIAN_POINT ( 'NONE',  ( 779.4763451958990572, -440.7363362996975980, 365.0264073115438919 ) ) ;
#10760 = CARTESIAN_POINT ( 'NONE',  ( 802.1676090361156639, -134.6346026584201070, 327.8955696845344505 ) ) ;
#10762 = CARTESIAN_POINT ( 'NONE',  ( 754.9735926884551418, -114.3510508353236617, 340.5236548041000333 ) ) ;
#10765 = CARTESIAN_POINT ( 'NONE',  ( 752.4576283171824116, -381.0783235625954717, 317.7880784355627952 ) ) ;
#10764 = CARTESIAN_POINT ( 'NONE',  ( 949.5497976682736407, 229.9999999999998579, -2132.806278688367456 ) ) ;
#10763 = DIRECTION ( 'NONE',  ( 1.000000000000000000, 0.000000000000000000, 0.000000000000000000 ) ) ;
#10766 = VERTEX_POINT ( 'NONE', #30286 ) ;
#10767 = CARTESIAN_POINT ( 'NONE',  ( 796.9571628226829034, -407.4636090269703459, -321.2382568024804641 ) ) ;
#10768 = CARTESIAN_POINT ( 'NONE',  ( 803.6646147819161570, -353.9073299311467053, -348.8264449731210561 ) ) ;
#10769 = CARTESIAN_POINT ( 'NONE',  ( 812.3518521366052028, -169.0999726633347393, -326.5853460496235243 ) ) ;
#10770 = CARTESIAN_POINT ( 'NONE',  ( 773.7305795820266212, -33.28179084515333130, 374.8230680027170365 ) ) ;
#10771 = VECTOR ( 'NONE', #30569, 1000.000000000000000 ) ;
#10773 = DIRECTION ( 'NONE',  ( 0.000000000000000000, 0.000000000000000000, 1.000000000000000000 ) ) ;
#10772 = DIRECTION ( 'NONE',  ( 1.000000000000000000, 0.000000000000000000, 0.000000000000000000 ) ) ;
#10774 = CARTESIAN_POINT ( 'NONE',  ( 801.3366627262608972, -296.5328690171411949, -353.0897708529566899 ) ) ;
#10775 = CARTESIAN_POINT ( 'NONE',  ( 789.5670355615794733, -453.0432664090020012, -363.0970091259334822 ) ) ;
#10776 = CARTESIAN_POINT ( 'NONE',  ( 809.0717654672305343, -172.9181544815165239, -360.1688906516309885 ) ) ;
#10777 = DIRECTION ( 'NONE',  ( -1.084653538143406060E-16, 0.6594541114781790059, 0.7517448203044204691 ) ) ;
#10778 = DIRECTION ( 'NONE',  ( 0.000000000000000000, -0.000000000000000000, -1.000000000000000000 ) ) ;
#10779 = AXIS2_PLACEMENT_3D ( 'NONE', #607, #22072, #14708 ) ;
#10780 = CARTESIAN_POINT ( 'NONE',  ( 779.4763451958990572, -368.7363362996977685, 365.0264073115438919 ) ) ;
#10781 = CARTESIAN_POINT ( 'NONE',  ( 760.0363995740630116, -346.9181544815160123, 368.7758568127991907 ) ) ;
#10782 = CARTESIAN_POINT ( 'NONE',  ( 782.4968714119720516, -202.8164208402380950, -305.0891759886411023 ) ) ;
#10783 = ADVANCED_FACE ( 'NONE', ( #29841, #1214 ), #15322, .T. ) ;
#10784 = CYLINDRICAL_SURFACE ( 'NONE', #14299, 12.00000000000001066 ) ;
#10785 = CARTESIAN_POINT ( 'NONE',  ( 794.9819416627830151, 11.00176097794305541, -319.9864689768909898 ) ) ;
#10786 = VECTOR ( 'NONE', #33904, 1000.000000000000000 ) ;
#10787 = CARTESIAN_POINT ( 'NONE',  ( 748.6759233522253680, -160.3726999360620482, 324.3348316497537098 ) ) ;
#10788 = CARTESIAN_POINT ( 'NONE',  ( 759.8311093483677041, -94.16923265350555994, -310.9282345327691814 ) ) ;
#10789 = CARTESIAN_POINT ( 'NONE',  ( 767.7687537140311633, -119.9073299311474443, 372.7932403749916830 ) ) ;
#10790 = CARTESIAN_POINT ( 'NONE',  ( 792.2312462859673587, -347.9073299311467053, -307.2067596250082602 ) ) ;
#10791 = ADVANCED_FACE ( 'NONE', ( #5582 ), #8615, .F. ) ;
#10792 = VECTOR ( 'NONE', #35067, 1000.000000000000000 ) ;
#10793 = CARTESIAN_POINT ( 'NONE',  ( 799.9999999999993179, -512.9681489794448908, -339.9999999999999432 ) ) ;
#10794 = DIRECTION ( 'NONE',  ( 0.000000000000000000, 0.000000000000000000, 1.000000000000000000 ) ) ;
#10795 = CARTESIAN_POINT ( 'NONE',  ( 756.3353852180819104, -173.9073299311472169, 331.1735550268788302 ) ) ;
#10796 = CARTESIAN_POINT ( 'NONE',  ( 802.9823548866075953, -1.099972663335260226, 330.0799878456151077 ) ) ;
#10797 = CARTESIAN_POINT ( 'NONE',  ( 776.2433038121456548, -396.8965053807772847, -374.8207195650711014 ) ) ;
#10798 = CARTESIAN_POINT ( 'NONE',  ( 767.7687537140311633, -407.9073299311465348, -372.7932403749916830 ) ) ;
#10799 = LINE ( 'NONE', #32724, #27648 ) ;
#10800 = CARTESIAN_POINT ( 'NONE',  ( 747.3154664389472828, 4.012585528312341054, 326.4474001241230781 ) ) ;
#10801 = ORIENTED_EDGE ( 'NONE', *, *, #9941, .T. ) ;
#10802 = CARTESIAN_POINT ( 'NONE',  ( 759.8311093483677041, -190.1692326535052189, -310.9282345327691814 ) ) ;
#10803 = DIRECTION ( 'NONE',  ( 1.000000000000000000, 0.000000000000000000, 0.000000000000000000 ) ) ;
#10804 = CARTESIAN_POINT ( 'NONE',  ( 748.3538107759620743, -304.7146871989594388, 355.8262568251490165 ) ) ;
#10805 = CARTESIAN_POINT ( 'NONE',  ( 802.1676090361155502, -134.6346026584201070, 327.8955696845344505 ) ) ;
#10806 = VERTEX_POINT ( 'NONE', #15991 ) ;
#10807 = AXIS2_PLACEMENT_3D ( 'NONE', #22899, #43925, #40480 ) ;
#10808 = CARTESIAN_POINT ( 'NONE',  ( 758.0580252608178853, -294.4527844766013800, 328.0187753319985404 ) ) ;
#10809 = AXIS2_PLACEMENT_3D ( 'NONE', #5397, #34037, #36833 ) ;
#10810 = CARTESIAN_POINT ( 'NONE',  ( 751.6929314249748586, -30.99823902205680071, -318.8095938919659034 ) ) ;
#10811 = ADVANCED_FACE ( 'NONE', ( #19673, #29404, #15538 ), #19007, .F. ) ;
#10812 = CARTESIAN_POINT ( 'NONE',  ( 744.7301800767020268, -76.81642084023847872, 337.4774526936615189 ) ) ;
#10813 = ORIENTED_EDGE ( 'NONE', *, *, #11170, .F. ) ;
#10814 = CARTESIAN_POINT ( 'NONE',  ( 802.2119215644370342, -462.0090635724247932, -367.5423716828165084 ) ) ;
#10815 = VERTEX_POINT ( 'NONE', #43476 ) ;
#10816 = SHAPE_DEFINITION_REPRESENTATION ( #35485, #15645 ) ;
#10817 = CARTESIAN_POINT ( 'NONE',  ( 797.6776695296629214, -19.54369356751139364, 357.6776695296636603 ) ) ;
#10818 = CARTESIAN_POINT ( 'NONE',  ( 797.6776695296629214, -307.5436935675104451, -357.6776695296636603 ) ) ;
#10819 = VECTOR ( 'NONE', #25124, 1000.000000000000000 ) ;
#10821 = CARTESIAN_POINT ( 'NONE',  ( 807.5423716828161105, -297.0783235625957559, 362.2119215644372048 ) ) ;
#10820 = CARTESIAN_POINT ( 'NONE',  ( 777.4774526936600978, -394.2709662947829088, 304.7301800767028226 ) ) ;
#10822 = CARTESIAN_POINT ( 'NONE',  ( 776.2433038121456548, -84.89650538077830788, 374.8207195650711014 ) ) ;
#10823 = CARTESIAN_POINT ( 'NONE',  ( 758.4439275373578084, -276.5545181178798657, -353.2243759319684386 ) ) ;
#10824 = CARTESIAN_POINT ( 'NONE',  ( 756.3353852180819104, -245.9073299311469896, -331.1735550268788302 ) ) ;
#10825 = LINE ( 'NONE', #6887, #12792 ) ;
#10826 = CARTESIAN_POINT ( 'NONE',  ( 792.1044303154645831, -108.4527844766019911, -317.8323909638837677 ) ) ;
#10827 = FACE_BOUND ( 'NONE', #2163, .T. ) ;
#10828 = CARTESIAN_POINT ( 'NONE',  ( 815.2698199232961542, -400.8164208402373561, 342.5225473063383106 ) ) ;
#10830 = CARTESIAN_POINT ( 'NONE',  ( 799.9999999999993179, -462.9681489794448339, -309.9999999999998863 ) ) ;
#10829 = CARTESIAN_POINT ( 'NONE',  ( 175.6195620086261613, 290.0000000000001137, -320.0000000000000568 ) ) ;
#10831 = CARTESIAN_POINT ( 'NONE',  ( 812.3518521366052028, -49.09997266333511590, -326.5853460496235243 ) ) ;
#10832 = LINE ( 'NONE', #38542, #7155 ) ;
#10833 = DIRECTION ( 'NONE',  ( 0.000000000000000000, 0.000000000000000000, -1.000000000000000000 ) ) ;
#10834 = EDGE_CURVE ( 'NONE', #11865, #10866, #33673, .T. ) ;
#10835 = CARTESIAN_POINT ( 'NONE',  ( 793.0897708529556667, -270.5545181178798657, 361.3366627262616362 ) ) ;
#10836 = CARTESIAN_POINT ( 'NONE',  ( 755.5713283507202505, -125.3618753856928834, 334.6858677611754729 ) ) ;
#10837 = ORIENTED_EDGE ( 'NONE', *, *, #21886, .F. ) ;
#10838 = CARTESIAN_POINT ( 'NONE',  ( 801.5560724626406000, -0.5545181178807169209, -326.7756240680316182 ) ) ;
#10839 = CARTESIAN_POINT ( 'NONE',  ( 744.7301800767020268, -100.8164208402383935, -337.4774526936615189 ) ) ;
#10840 = CARTESIAN_POINT ( 'NONE',  ( 790.8726784830453198, -298.7146871989593251, 362.5472867521010585 ) ) ;
#10841 = CARTESIAN_POINT ( 'NONE',  ( 803.6646147819161570, -449.9073299311463643, -348.8264449731210561 ) ) ;
#10842 = CARTESIAN_POINT ( 'NONE',  ( 807.2620300519052989, -24.00906357242609346, 318.0141637701419768 ) ) ;
#10844 = AXIS2_PLACEMENT_3D ( 'NONE', #31613, #38784, #39240 ) ;
#10843 = CARTESIAN_POINT ( 'NONE',  ( 812.7932403749906598, -231.1800572038743553, -327.7687537140311633 ) ) ;
#10845 = EDGE_CURVE ( 'NONE', #1374, #34451, #44728, .T. ) ;
#10846 = CARTESIAN_POINT ( 'NONE',  ( 801.1904061080336987, -188.0891481129653187, 368.3070685750235498 ) ) ;
#10847 = CARTESIAN_POINT ( 'NONE',  ( 803.4237431249931660, -87.18005720387481006, 331.2633955100225194 ) ) ;
#10848 = VECTOR ( 'NONE', #34094, 1000.000000000000114 ) ;
#10849 = CARTESIAN_POINT ( 'NONE',  ( 181.1634899080285948, 240.0000000000000284, -199.9999999999953957 ) ) ;
#10850 = CARTESIAN_POINT ( 'NONE',  ( 745.1769319972822814, -305.8055962898684470, -346.2694204179732083 ) ) ;
#10851 = VECTOR ( 'NONE', #14648, 1000.000000000000000 ) ;
#10852 = CARTESIAN_POINT ( 'NONE',  ( 786.2694204179717872, -453.2817908451519315, 305.1769319972829067 ) ) ;
#10853 = CARTESIAN_POINT ( 'NONE',  ( 815.2698199232961542, -304.8164208402376403, -342.5225473063383106 ) ) ;
#10854 = CARTESIAN_POINT ( 'NONE',  ( 799.9999999999993179, 205.0000000000000568, -339.9999999999999432 ) ) ;
#10855 = CARTESIAN_POINT ( 'NONE',  ( 800.7704444035546203, -364.1692326535046504, 326.0291762391768771 ) ) ;
#10856 = CARTESIAN_POINT ( 'NONE',  ( 792.3570229623691148, -45.18005720387493795, 373.1304606946836770 ) ) ;
#10857 = CARTESIAN_POINT ( 'NONE',  ( 781.8018195045266339, -382.2709662947828519, -365.1927285166406705 ) ) ;
#10858 = AXIS2_PLACEMENT_3D ( 'NONE', #10529, #24605, #7084 ) ;
#10859 = CARTESIAN_POINT ( 'NONE',  ( 804.1601925771018387, -55.44195992623293989, 346.5483106153029098 ) ) ;
#10860 = CARTESIAN_POINT ( 'NONE',  ( 762.1405469898971887, -193.5436935675108714, -357.8594530101015607 ) ) ;
#10861 = CARTESIAN_POINT ( 'NONE',  ( 786.2056067578752163, -83.80559628986920018, -374.4686193811670023 ) ) ;
#10862 = EDGE_CURVE ( 'NONE', #2789, #8317, #11844, .T. ) ;
#10863 = CARTESIAN_POINT ( 'NONE',  ( 754.0944755984390895, -207.6237781080506295, 364.1009440267246760 ) ) ;
#10864 = CARTESIAN_POINT ( 'NONE',  ( 755.5713283507202505, -29.36187538569318178, 334.6858677611754729 ) ) ;
#10865 = EDGE_CURVE ( 'NONE', #41883, #30506, #11566, .T. ) ;
#10866 = VERTEX_POINT ( 'NONE', #44152 ) ;
#10867 = CARTESIAN_POINT ( 'NONE',  ( 763.2154366446407039, -213.6237781080506011, -321.4292242960311228 ) ) ;
#10868 = CARTESIAN_POINT ( 'NONE',  ( 781.8018195045266339, -214.2709662947834488, 365.1927285166406705 ) ) ;
#10869 = CARTESIAN_POINT ( 'NONE',  ( 764.3348316497523456, -22.71468719896029853, -308.6759233522265617 ) ) ;
#10870 = CARTESIAN_POINT ( 'NONE',  ( 800.2193346964446619, -330.9982390220558273, 355.1360043628816925 ) ) ;
#10871 = CARTESIAN_POINT ( 'NONE',  ( 808.6629988358042738, -452.9681489794447771, -336.2505073875255448 ) ) ;
#10872 = CARTESIAN_POINT ( 'NONE',  ( 939.9999999999993179, -422.8782571739196214, 207.4246812887968758 ) ) ;
#10873 = EDGE_LOOP ( 'NONE', ( #694, #12394, #3705, #1320 ) ) ;
#10874 = CARTESIAN_POINT ( 'NONE',  ( 794.1144889064781864, -58.16923265350564520, 360.9840315886528401 ) ) ;
#10875 = CARTESIAN_POINT ( 'NONE',  ( 791.0478386215596629, -357.8272453906068904, -306.7653713866226326 ) ) ;
#10876 = CARTESIAN_POINT ( 'NONE',  ( 810.7187646348534145, -258.4527844766016074, 356.7737145352016341 ) ) ;
#10877 = CARTESIAN_POINT ( 'NONE',  ( 754.0944755984390895, -15.62377810805123524, 364.1009440267246760 ) ) ;
#10878 = CARTESIAN_POINT ( 'NONE',  ( 763.0428371773158460, -155.4636090269711417, -358.7617431975195359 ) ) ;
#10879 = CARTESIAN_POINT ( 'NONE',  ( 754.8072714833581358, -148.8164208402382656, -338.1981804954720587 ) ) ;
#10880 = CARTESIAN_POINT ( 'NONE',  ( 759.9864689768902508, -338.0891481129649492, -354.9819416627836404 ) ) ;
#10881 = VERTEX_POINT ( 'NONE', #12735 ) ;
#10882 = AXIS2_PLACEMENT_3D ( 'NONE', #37780, #21140, #20219 ) ;
#10883 = CARTESIAN_POINT ( 'NONE',  ( 804.7487373415286811, -283.5436935675105019, 364.7487373415288516 ) ) ;
#10884 = EDGE_CURVE ( 'NONE', #1637, #45115, #8378, .T. ) ;
#10885 = PLANE ( 'NONE',  #40307 ) ;
#10886 = CARTESIAN_POINT ( 'NONE',  ( 803.2186876482843445, -343.9874144716865771, 350.0220218866286928 ) ) ;
#10887 = LINE ( 'NONE', #36050, #3208 ) ;
#10888 = EDGE_CURVE ( 'NONE', #28460, #5848, #40260, .T. ) ;
#10889 = CARTESIAN_POINT ( 'NONE',  ( 793.0897708529556667, -150.5545181178802352, 361.3366627262616362 ) ) ;
#10890 = CARTESIAN_POINT ( 'NONE',  ( 800.0135310231082713, -14.08914811296595460, 325.0180583372163028 ) ) ;
#10891 = VERTEX_POINT ( 'NONE', #1652 ) ;
#10892 = CARTESIAN_POINT ( 'NONE',  ( 760.0363995740630116, -370.9181544815159555, -368.7758568127991907 ) ) ;
#10893 = CARTESIAN_POINT ( 'NONE',  ( 805.0032342141413437, 10.45630643248851044, -314.9967657858572352 ) ) ;
#10894 = CARTESIAN_POINT ( 'NONE',  ( 781.2370466360911223, -284.7363362996979390, 304.9990715423533629 ) ) ;
#10895 = CARTESIAN_POINT ( 'NONE',  ( 784.0799538623451781, -203.8055962898688449, 364.6971507214555572 ) ) ;
#10896 = CARTESIAN_POINT ( 'NONE',  ( 759.9864689768902508, -362.0891481129648923, -354.9819416627836404 ) ) ;
#10897 = CARTESIAN_POINT ( 'NONE',  ( 795.1360043628807261, 3.910851887033985896, 360.2193346964456282 ) ) ;
#10898 = CARTESIAN_POINT ( 'NONE',  ( 1238.921997096861332, 240.0000000000000568, -244.9999999999999716 ) ) ;
#10899 = CARTESIAN_POINT ( 'NONE',  ( 790.0220218866281812, -223.0999726633346256, -363.2186876482849129 ) ) ;
#10900 = EDGE_CURVE ( 'NONE', #14035, #14853, #18778, .T. ) ;
#10901 = ADVANCED_FACE ( 'NONE', ( #36552 ), #19220, .T. ) ;
#10902 = CARTESIAN_POINT ( 'NONE',  ( 801.1904061080336987, -20.08914811296592973, 368.3070685750235498 ) ) ;
#10903 = CARTESIAN_POINT ( 'NONE',  ( 808.0189434323515343, -86.08914811296573077, 319.0252816721025511 ) ) ;
#10904 = DIRECTION ( 'NONE',  ( 1.000000000000000000, -0.000000000000000000, -0.000000000000000000 ) ) ;
#10905 = CARTESIAN_POINT ( 'NONE',  ( 801.1904061080338124, -428.0891481129645513, -368.3070685750236066 ) ) ;
#10906 = DIRECTION ( 'NONE',  ( 0.000000000000000000, 0.000000000000000000, -1.000000000000000000 ) ) ;
#10907 = CARTESIAN_POINT ( 'NONE',  ( 745.1792804349281596, -350.1908817542433212, 343.7566961878542884 ) ) ;
#10908 = CARTESIAN_POINT ( 'NONE',  ( -338.8365100919713200, 230.0000000000001137, -199.9999999999917861 ) ) ;
#10909 = CARTESIAN_POINT ( 'NONE',  ( 801.1904061080336987, -332.0891481129649492, 368.3070685750235498 ) ) ;
#10910 = CARTESIAN_POINT ( 'NONE',  ( 811.0346526505616112, -62.63460265842031305, -323.0537975583477532 ) ) ;
#10911 = CARTESIAN_POINT ( 'NONE',  ( 792.1044303154645831, -276.4527844766013800, -317.8323909638837677 ) ) ;
#10912 = FACE_BOUND ( 'NONE', #38183, .T. ) ;
#10913 = CARTESIAN_POINT ( 'NONE',  ( 754.8072714833581358, -436.8164208402372992, 338.1981804954720587 ) ) ;
#10914 = CARTESIAN_POINT ( 'NONE',  ( 787.5531968255692163, -189.8272453906073736, 316.1348686366205811 ) ) ;
#10915 = CARTESIAN_POINT ( 'NONE',  ( 805.6418435158337843, -77.46360902697138329, -363.8556311672236916 ) ) ;
#10916 = CARTESIAN_POINT ( 'NONE',  ( 805.1016975059191054, -78.89650538077832209, -343.0745993439771837 ) ) ;
#10917 = CARTESIAN_POINT ( 'NONE',  ( 746.7653713866222915, -89.26014174441463922, 351.0478386215610271 ) ) ;
#10918 = CARTESIAN_POINT ( 'NONE',  ( 755.0636971347428243, -388.2709662947829656, 341.7834795799807353 ) ) ;
#10919 = VECTOR ( 'NONE', #23561, 1000.000000000000000 ) ;
#10920 = CARTESIAN_POINT ( 'NONE',  ( 800.2193346964447755, -450.9982390220554294, 355.1360043628815788 ) ) ;
#10922 = ORIENTED_EDGE ( 'NONE', *, *, #34797, .T. ) ;
#10921 = CARTESIAN_POINT ( 'NONE',  ( 801.3366627262608972, -104.5328690171418913, -353.0897708529566899 ) ) ;
#10923 = CARTESIAN_POINT ( 'NONE',  ( 803.4237431249931660, -87.18005720387481006, -331.2633955100225194 ) ) ;
#10924 = CARTESIAN_POINT ( 'NONE',  ( 786.6156483768007774, -385.4419599262319593, -315.5913626894246136 ) ) ;
#10926 = CARTESIAN_POINT ( 'NONE',  ( 794.9819416627830151, -228.9982390220561683, 319.9864689768909898 ) ) ;
#10925 = CARTESIAN_POINT ( 'NONE',  ( 788.8264449731200330, -213.1800572038743553, 363.6646147819171233 ) ) ;
#10927 = EDGE_LOOP ( 'NONE', ( #1803, #1367, #20978, #45120 ) ) ;
#10928 = CARTESIAN_POINT ( 'NONE',  ( 813.2346286133761168, -413.2601417444136018, -328.9521613784389160 ) ) ;
#10929 = DIRECTION ( 'NONE',  ( -0.000000000000000000, 1.000000000000000000, -0.000000000000000000 ) ) ;
#10930 = VERTEX_POINT ( 'NONE', #12303 ) ;
#10931 = CARTESIAN_POINT ( 'NONE',  ( 764.8639956371174549, -416.0891481129645513, 319.7806653035542013 ) ) ;
#10932 = EDGE_LOOP ( 'NONE', ( #16729, #35225, #3892, #20497 ) ) ;
#10933 = CARTESIAN_POINT ( 'NONE',  ( 787.4397851343537695, -261.7255117493288026, -374.2001403089903988 ) ) ;
#10934 = CARTESIAN_POINT ( 'NONE',  ( 808.3070685750232087, -138.9982390220564241, 361.1904061080339829 ) ) ;
#10935 = CARTESIAN_POINT ( 'NONE',  ( 766.9102291470427417, -282.5545181178798657, 318.6633372737382501 ) ) ;
#10936 = ORIENTED_EDGE ( 'NONE', *, *, #20487, .T. ) ;
#10937 = CARTESIAN_POINT ( 'NONE',  ( 800.2193346964446619, -258.9982390220561115, -355.1360043628816925 ) ) ;
#10938 = ORIENTED_EDGE ( 'NONE', *, *, #27763, .F. ) ;
#10939 = CARTESIAN_POINT ( 'NONE',  ( 774.6312213355099630, -359.3618753856920875, -364.6798772138717482 ) ) ;
#10940 = CARTESIAN_POINT ( 'NONE',  ( 759.7806653035534055, -6.998239022056885972, -324.8639956371180801 ) ) ;
#10941 = SHAPE_REPRESENTATION ( 'Heavy Cast Iron Table Bed Base', ( #26858 ), #39435 ) ;
#10942 = EDGE_CURVE ( 'NONE', #32232, #4341, #17468, .T. ) ;
#10943 = CARTESIAN_POINT ( 'NONE',  ( 800.7704444035546203, -220.1692326535051052, 326.0291762391768771 ) ) ;
#10944 = CARTESIAN_POINT ( 'NONE',  ( 200.7583438952259485, 394.6698570112193920, -274.9999999999999432 ) ) ;
#10945 = LINE ( 'NONE', #21780, #7898 ) ;
#10946 = EDGE_LOOP ( 'NONE', ( #9036, #43240, #28492, #23204 ) ) ;
#10947 = CARTESIAN_POINT ( 'NONE',  ( 764.8639956371174549, -32.08914811296588709, -319.7806653035542013 ) ) ;
#10948 = CARTESIAN_POINT ( 'NONE',  ( 190.7583438952259485, 394.6698570112193920, -274.9999999999999432 ) ) ;
#10949 = DIRECTION ( 'NONE',  ( -0.000000000000000000, 1.000000000000000000, -0.000000000000000000 ) ) ;
#10950 = ORIENTED_EDGE ( 'NONE', *, *, #34864, .F. ) ;
#10951 = CARTESIAN_POINT ( 'NONE',  ( 760.0363995740630116, -274.9181544815161828, -368.7758568127991907 ) ) ;
#10952 = CARTESIAN_POINT ( 'NONE',  ( 750.9282345327678740, -136.9181544815166376, 319.8311093483690115 ) ) ;
#10953 = VECTOR ( 'NONE', #42422, 1000.000000000000000 ) ;
#10955 = CARTESIAN_POINT ( 'NONE',  ( 765.0180583372156207, -264.9982390220561115, -360.0135310231089534 ) ) ;
#10954 = CARTESIAN_POINT ( 'NONE',  ( -773.4999999999993179, -544.8427095258973623, -369.9999999999999432 ) ) ;
#10956 = DIRECTION ( 'NONE',  ( -0.000000000000000000, 1.000000000000000000, -0.000000000000000000 ) ) ;
#10957 = CARTESIAN_POINT ( 'NONE',  ( 755.5913626894240451, -133.6454272087893571, -346.6156483768012890 ) ) ;
#10958 = ADVANCED_FACE ( 'NONE', ( #19439, #12518 ), #26592, .F. ) ;
#10959 = CARTESIAN_POINT ( 'NONE',  ( 745.1792804349281596, -374.1908817542432075, 343.7566961878542884 ) ) ;
#10960 = DIRECTION ( 'NONE',  ( 0.000000000000000000, -1.000000000000000000, 1.672022627447524993E-16 ) ) ;
#10961 = CARTESIAN_POINT ( 'NONE',  ( 807.5423716828161105, 14.92167643740321381, -362.2119215644372048 ) ) ;
#10962 = CARTESIAN_POINT ( 'NONE',  ( 745.7998596910086917, -317.3618753856922581, -332.5602148656461168 ) ) ;
#10963 = DIRECTION ( 'NONE',  ( 0.000000000000000000, 0.000000000000000000, -1.000000000000000000 ) ) ;
#10964 = CARTESIAN_POINT ( 'NONE',  ( 778.2165204200184689, 1.183579159761269040, 364.9363028652563230 ) ) ;
#10965 = CARTESIAN_POINT ( 'NONE',  ( 810.4231160770870019, -240.5545181178798941, 321.9338519418446936 ) ) ;
#10966 = CARTESIAN_POINT ( 'NONE',  ( 745.1769319972822814, -185.8055962898689302, -346.2694204179732083 ) ) ;
#10967 = CARTESIAN_POINT ( 'NONE',  ( 805.0032342141412300, -229.5436935675106440, 314.9967657858571783 ) ) ;
#10968 = CARTESIAN_POINT ( 'NONE',  ( 796.7737145352015204, -452.6346026584191691, -370.7187646348536987 ) ) ;
#10969 = DIRECTION ( 'NONE',  ( -0.000000000000000000, 1.000000000000000000, -0.000000000000000000 ) ) ;
#10970 = CARTESIAN_POINT ( 'NONE',  ( 756.3353852180819104, -341.9073299311465917, 331.1735550268788302 ) ) ;
#10971 = CARTESIAN_POINT ( 'NONE',  ( 790.0220218866281812, -103.0999726633349525, 363.2186876482849129 ) ) ;
#10972 = CARTESIAN_POINT ( 'NONE',  ( 763.8424801807145741, -90.00906357242590161, 320.5453621957614700 ) ) ;
#10973 = CARTESIAN_POINT ( 'NONE',  ( 758.6633372737375112, 3.467130982857797417, -326.9102291470432533 ) ) ;
#10974 = CARTESIAN_POINT ( 'NONE',  ( -115.7583438952258774, 430.0000000000002842, -244.9999999999999716 ) ) ;
#10975 = FACE_OUTER_BOUND ( 'NONE', #39449, .T. ) ;
#10977 = CARTESIAN_POINT ( 'NONE',  ( 771.1735550268778070, -345.1800572038739006, 316.3353852180827630 ) ) ;
#10976 = CARTESIAN_POINT ( 'NONE',  ( 779.4709603349208464, -144.3510508353235764, 314.7162404726379918 ) ) ;
#10978 = ORIENTED_EDGE ( 'NONE', *, *, #1528, .F. ) ;
#10979 = CARTESIAN_POINT ( 'NONE',  ( 800.0135310231082713, -38.08914811296587999, -325.0180583372163028 ) ) ;
#10980 = CARTESIAN_POINT ( 'NONE',  ( 758.6633372737375112, -284.5328690171412518, -326.9102291470432533 ) ) ;
#10981 = CARTESIAN_POINT ( 'NONE',  ( 797.6776695296629214, -115.5436935675110988, 357.6776695296636603 ) ) ;
#10982 = CARTESIAN_POINT ( 'NONE',  ( 749.8865473780648472, -308.5328690171412518, -322.1177392798429082 ) ) ;
#10983 = CARTESIAN_POINT ( 'NONE',  ( -521.6730038022808458, 200.0000000000001421, 339.9999999999999432 ) ) ;
#10984 = CARTESIAN_POINT ( 'NONE',  ( 744.8212110874229666, -426.8965053807771142, 336.2046728542121627 ) ) ;
#10985 = VERTEX_POINT ( 'NONE', #44616 ) ;
#10986 = CARTESIAN_POINT ( 'NONE',  ( 797.8594530101008786, -325.5436935675105019, 322.1405469898980982 ) ) ;
#10987 = AXIS2_PLACEMENT_3D ( 'NONE', #30998, #1303, #16449 ) ;
#10988 = CARTESIAN_POINT ( 'NONE',  ( 805.1016975059191054, -78.89650538077832209, -343.0745993439771837 ) ) ;
#10989 = CARTESIAN_POINT ( 'NONE',  ( 802.1676090361156639, -158.6346026584199933, -327.8955696845344505 ) ) ;
#10990 = CARTESIAN_POINT ( 'NONE',  ( 754.8072714833581358, -220.8164208402379529, -338.1981804954720587 ) ) ;
#10991 = CARTESIAN_POINT ( 'NONE',  ( 804.6798772138708955, -399.7255117493283478, 334.6312213355107019 ) ) ;
#10992 = CARTESIAN_POINT ( 'NONE',  ( 808.3070685750230950, -162.9982390220563673, -361.1904061080339261 ) ) ;
#10993 = ORIENTED_EDGE ( 'NONE', *, *, #31782, .T. ) ;
#10994 = CARTESIAN_POINT ( 'NONE',  ( 804.6798772138710092, -135.7255117493291721, -334.6312213355106451 ) ) ;
#10995 = EDGE_LOOP ( 'NONE', ( #5619, #39126, #23938, #32115 ) ) ;
#10996 = CARTESIAN_POINT ( 'NONE',  ( 786.5483106153019435, -391.6454272087885897, -364.1601925771022366 ) ) ;
#10997 = CARTESIAN_POINT ( 'NONE',  ( 769.9779781133707957, -451.0999726633339151, 316.7813123517150871 ) ) ;
#10998 = CARTESIAN_POINT ( 'NONE',  ( 754.8983024940795303, -138.8965053807781374, 336.9254006560228163 ) ) ;
#11001 = CARTESIAN_POINT ( 'NONE',  ( 754.0944755984390895, -375.6237781080501463, 364.1009440267246760 ) ) ;
#11000 = DIRECTION ( 'NONE',  ( -1.000000000000000000, -0.000000000000000000, 0.000000000000000000 ) ) ;
#10999 = PLANE ( 'NONE',  #26242 ) ;
#11002 = EDGE_LOOP ( 'NONE', ( #22131, #4292, #35284, #29846 ) ) ;
#11003 = CARTESIAN_POINT ( 'NONE',  ( 804.8461984189677878, -386.1908817542432075, -336.9566956441385628 ) ) ;
#11004 = CARTESIAN_POINT ( 'NONE',  ( 999.9999999999992042, 239.9999999999998863, 209.9999999999999716 ) ) ;
#11005 = CARTESIAN_POINT ( 'NONE',  ( 783.7953271457878373, -152.1908817542438612, -375.1787889125761239 ) ) ;
#11006 = CARTESIAN_POINT ( 'NONE',  ( 799.9636004259356241, -22.91815448151701062, 311.2241431872006956 ) ) ;
#11008 = FACE_OUTER_BOUND ( 'NONE', #36046, .T. ) ;
#11007 = DIRECTION ( 'NONE',  ( -1.000000000000000000, 0.000000000000000000, 0.000000000000000000 ) ) ;
#11009 = CARTESIAN_POINT ( 'NONE',  ( 779.4709603349208464, -288.3510508353231216, -314.7162404726379918 ) ) ;
#11010 = CARTESIAN_POINT ( 'NONE',  ( 797.6776695296629214, -451.5436935675099903, -357.6776695296636603 ) ) ;
#11011 = CARTESIAN_POINT ( 'NONE',  ( 778.7629533639073998, -200.7363362996982801, -375.0009284576466371 ) ) ;
#11012 = CARTESIAN_POINT ( 'NONE',  ( 779.9999999999992042, 166.4563064324884465, -329.9999999999999432 ) ) ;
#11013 = DIRECTION ( 'NONE',  ( 1.000000000000000000, 0.000000000000000000, -0.000000000000000000 ) ) ;
#11014 = CARTESIAN_POINT ( 'NONE',  ( 780.5236548040995785, -356.7363362996978253, 314.9735926884559944 ) ) ;
#11015 = CARTESIAN_POINT ( 'NONE',  ( 773.7305795820266212, -345.2817908451523863, 374.8230680027170365 ) ) ;
#11016 = CARTESIAN_POINT ( 'NONE',  ( 751.9810565676468741, -194.0891481129654039, -360.9747183278973921 ) ) ;
#11017 = CARTESIAN_POINT ( 'NONE',  ( 769.9999999999992042, 240.0000000000000568, -319.9999999999999432 ) ) ;
#11018 = CARTESIAN_POINT ( 'NONE',  ( 792.1044303154645831, 11.54721552339760038, -317.8323909638837677 ) ) ;
#11019 = AXIS2_PLACEMENT_3D ( 'NONE', #20317, #43886, #2300 ) ;
#11020 = CARTESIAN_POINT ( 'NONE',  ( 795.8262568251477660, -142.3726999360620766, 308.3538107759623585 ) ) ;
#11021 = CARTESIAN_POINT ( 'NONE',  ( 807.5423716828161105, -81.07832356259649487, -362.2119215644372048 ) ) ;
#11022 = CARTESIAN_POINT ( 'NONE',  ( 763.0537975583475827, -120.4527844766019484, 371.0346526505627480 ) ) ;
#11023 = CARTESIAN_POINT ( 'NONE',  ( 808.3070685750230950, -354.9982390220557704, -361.1904061080339261 ) ) ;
#11024 = DIRECTION ( 'NONE',  ( 0.000000000000000000, 1.000000000000000000, 0.000000000000000000 ) ) ;
#11025 = DIRECTION ( 'NONE',  ( 0.7014439490181308967, -0.1263042864341425708, 0.7014439490181749726 ) ) ;
#11026 = CARTESIAN_POINT ( 'NONE',  ( 755.5713283507202505, -221.3618753856925707, 334.6858677611754729 ) ) ;
#11027 = CARTESIAN_POINT ( 'NONE',  ( 796.2681130854250569, -462.7578698805381237, 371.0719813302654870 ) ) ;
#11028 = CARTESIAN_POINT ( 'NONE',  ( 798.0661480581538854, -410.5328690171408539, -309.5768839229118043 ) ) ;
#11029 = CARTESIAN_POINT ( 'NONE',  ( 808.3070685750230950, -426.9982390220554862, -361.1904061080339261 ) ) ;
#11030 = DIRECTION ( 'NONE',  ( -0.000000000000000000, 1.000000000000000000, -0.000000000000000000 ) ) ;
#11031 = CARTESIAN_POINT ( 'NONE',  ( 798.0661480581538854, -2.532869017142183932, 309.5768839229118043 ) ) ;
#11032 = VERTEX_POINT ( 'NONE', #30514 ) ;
#11033 = CARTESIAN_POINT ( 'NONE',  ( 781.2497674668890113, -180.3510508353234343, -375.3608509340180603 ) ) ;
#11034 = SURFACE_STYLE_FILL_AREA ( #26000 ) ;
#11035 = CARTESIAN_POINT ( 'NONE',  ( 761.9338519418445230, -302.5328690171411949, 370.4231160770881957 ) ) ;
#11036 = CARTESIAN_POINT ( 'NONE',  ( 781.8018195045267476, -142.2709662947837330, 365.1927285166407273 ) ) ;
#11037 = ORIENTED_EDGE ( 'NONE', *, *, #20142, .F. ) ;
#11038 = CARTESIAN_POINT ( 'NONE',  ( 800.2193346964447755, -306.9982390220558273, 355.1360043628815788 ) ) ;
#11039 = CARTESIAN_POINT ( 'NONE',  ( 767.6429770376289525, -33.18005720387498769, -306.8695393053162093 ) ) ;
#11040 = CARTESIAN_POINT ( 'NONE',  ( 814.9108240113580450, -88.27096629478390355, 337.5031285880265273 ) ) ;
#11041 = EDGE_CURVE ( 'NONE', #42322, #23619, #16901, .T. ) ;
#11042 = ORIENTED_EDGE ( 'NONE', *, *, #36032, .T. ) ;
#11043 = CARTESIAN_POINT ( 'NONE',  ( 752.7379699480933368, -444.0090635724249069, -361.9858362298580232 ) ) ;
#11044 = AXIS2_PLACEMENT_3D ( 'NONE', #20406, #2628, #3319 ) ;
#11045 = ORIENTED_EDGE ( 'NONE', *, *, #2415, .T. ) ;
#11046 = SHAPE_DEFINITION_REPRESENTATION ( #20332, #27662 ) ;
#11047 = CARTESIAN_POINT ( 'NONE',  ( 792.1044303154645831, -36.45278447660223975, 317.8323909638837677 ) ) ;
#11048 = CARTESIAN_POINT ( 'NONE',  ( 755.0636971347428243, -292.2709662947831930, -341.7834795799807353 ) ) ;
#11050 = CARTESIAN_POINT ( 'NONE',  ( 807.5423716828161105, -273.0783235625958696, 362.2119215644372048 ) ) ;
#11049 = CARTESIAN_POINT ( 'NONE',  ( 796.7737145352015204, -404.6346026584193396, 370.7187646348536987 ) ) ;
#11051 = CARTESIAN_POINT ( 'NONE',  ( 756.1443688327750579, -69.62377810805107003, 314.3581564841659315 ) ) ;
#11052 = CARTESIAN_POINT ( 'NONE',  ( 755.1538015810308480, -278.1908817542434917, -343.0433043558613804 ) ) ;
#11053 = CARTESIAN_POINT ( 'NONE',  ( 800.0135310231082713, -302.0891481129650629, -325.0180583372163028 ) ) ;
#11054 = CARTESIAN_POINT ( 'NONE',  ( 571.1634899080285095, 259.9999999999999432, -202.7499999999980105 ) ) ;
#11055 = CARTESIAN_POINT ( 'NONE',  ( 785.3687786644884454, -131.3618753856928834, -315.3201227861279676 ) ) ;
#11056 = CARTESIAN_POINT ( 'NONE',  ( 745.0891759886404770, -388.2709662947829656, 342.4968714119734159 ) ) ;
#11058 = DIRECTION ( 'NONE',  ( 0.000000000000000000, -0.000000000000000000, 1.000000000000000000 ) ) ;
#11057 = DIRECTION ( 'NONE',  ( -0.000000000000000000, 1.000000000000000000, -0.000000000000000000 ) ) ;
#11059 = CARTESIAN_POINT ( 'NONE',  ( 812.3518521366052028, -73.09997266333502353, -326.5853460496235243 ) ) ;
#11060 = CARTESIAN_POINT ( 'NONE',  ( 939.9999999999992042, -185.0721577059061929, 75.19946970736496894 ) ) ;
#11061 = CARTESIAN_POINT ( 'NONE',  ( -468.8365100919714337, 256.5000000000001705, -197.2499999999909619 ) ) ;
#11062 = CARTESIAN_POINT ( 'NONE',  ( 758.4439275373578084, -276.5545181178798657, 353.2243759319684386 ) ) ;
#11063 = CARTESIAN_POINT ( 'NONE',  ( 802.1676090361156639, -158.6346026584199933, 327.8955696845344505 ) ) ;
#11064 = ORIENTED_EDGE ( 'NONE', *, *, #26420, .T. ) ;
#11065 = CARTESIAN_POINT ( 'NONE',  ( 754.7162404726377645, -38.73633629969877035, -339.4709603349214717 ) ) ;
#11066 = CARTESIAN_POINT ( 'NONE',  ( 814.9108240113580450, -112.2709662947838325, -337.5031285880265273 ) ) ;
#11067 = CARTESIAN_POINT ( 'NONE',  ( 804.1601925771018387, -319.4419599262320730, 346.5483106153029098 ) ) ;
#11068 = LINE ( 'NONE', #25135, #13039 ) ;
#11069 = CARTESIAN_POINT ( 'NONE',  ( 815.3608509340175488, -26.73633629969882008, 341.2497674668889545 ) ) ;
#11070 = CARTESIAN_POINT ( 'NONE',  ( 810.7187646348534145, -234.4527844766016358, -356.7737145352016341 ) ) ;
#11071 = CARTESIAN_POINT ( 'NONE',  ( 767.8955696845333705, -72.45278447660213317, 362.1676090361162323 ) ) ;
#11072 = CARTESIAN_POINT ( 'NONE',  ( 799.9999999999993179, -512.9681489794448908, -309.9999999999998863 ) ) ;
#11073 = CARTESIAN_POINT ( 'NONE',  ( 746.7653713866222915, -305.2601417444139429, -351.0478386215610271 ) ) ;
#11074 = CARTESIAN_POINT ( 'NONE',  ( 744.6391490659812007, -446.7363362996975980, 338.7502325331110455 ) ) ;
#11075 = CARTESIAN_POINT ( 'NONE',  ( 744.7301800767019131, -316.8164208402377540, -337.4774526936615757 ) ) ;
#11076 = CARTESIAN_POINT ( 'NONE',  ( 799.9999999999993179, 205.0000000000000568, 255.0000000000000000 ) ) ;
#11077 = CARTESIAN_POINT ( 'NONE',  ( 776.9566956441375396, -372.8965053807773415, 364.8461984189686405 ) ) ;
#11078 = CARTESIAN_POINT ( 'NONE',  ( 805.0032342141413437, -37.54369356751133324, 314.9967657858572352 ) ) ;
#11079 = CARTESIAN_POINT ( 'NONE',  ( 785.3141322388236176, -381.7255117493284615, -364.4286716492789537 ) ) ;
#11080 = CARTESIAN_POINT ( 'NONE',  ( 794.1144889064781864, -58.16923265350564520, 360.9840315886528401 ) ) ;
#11081 = CARTESIAN_POINT ( 'NONE',  ( 749.8865473780648472, -68.53286901714197654, -322.1177392798429082 ) ) ;
#11082 = CARTESIAN_POINT ( 'NONE',  ( 811.6461892240364477, -220.7146871989596661, 324.1737431748509835 ) ) ;
#11083 = CARTESIAN_POINT ( 'NONE',  ( 778.1981804954715471, -34.27096629478407408, 314.8072714833591021 ) ) ;
#11084 = ORIENTED_EDGE ( 'NONE', *, *, #31441, .F. ) ;
#11085 = CARTESIAN_POINT ( 'NONE',  ( 780.5290396650775619, -204.3510508353233774, -365.2837595273619513 ) ) ;
#11086 = CARTESIAN_POINT ( 'NONE',  ( 788.8264449731200330, -213.1800572038743553, 363.6646147819171233 ) ) ;
#11087 = EDGE_CURVE ( 'NONE', #3816, #40052, #1944, .T. ) ;
#11088 = CARTESIAN_POINT ( 'NONE',  ( 783.7566961878529810, -24.89650538077847486, -305.1792804349288417 ) ) ;
#11089 = CARTESIAN_POINT ( 'NONE',  ( 785.3687786644885591, -323.3618753856922581, 315.3201227861280813 ) ) ;
#11090 = CARTESIAN_POINT ( 'NONE',  ( 803.8904222555790966, -452.9681489794450044, -350.1048529224749473 ) ) ;
#11091 = CARTESIAN_POINT ( 'NONE',  ( 794.9999999999993179, 205.0000000000000568, -265.0000000000000000 ) ) ;
#11092 = ORIENTED_EDGE ( 'NONE', *, *, #22976, .T. ) ;
#11093 = CARTESIAN_POINT ( 'NONE',  ( 773.3843516231979720, -61.44195992623291147, 364.4086373105754433 ) ) ;
#11094 = CARTESIAN_POINT ( 'NONE',  ( 810.4231160770870019, -336.5545181178796952, -321.9338519418446936 ) ) ;
#11095 = ADVANCED_FACE ( 'NONE', ( #12980 ), #38782, .F. ) ;
#11096 = CARTESIAN_POINT ( 'NONE',  ( 746.8695393053151292, -293.9073299311468759, 327.6429770376306578 ) ) ;
#11097 = CARTESIAN_POINT ( 'NONE',  ( 812.6845335610512393, 16.01258552831230375, 353.5525998758768651 ) ) ;
#11098 = CARTESIAN_POINT ( 'NONE',  ( 804.6971507214547046, -171.2817908451529263, -344.0799538623459739 ) ) ;
#11099 = CARTESIAN_POINT ( 'NONE',  ( 797.6776695296629214, -163.5436935675109567, -357.6776695296636603 ) ) ;
#11100 = CARTESIAN_POINT ( 'NONE',  ( 754.8072714833583632, -364.8164208402375266, -338.1981804954721156 ) ) ;
#11101 = ORIENTED_EDGE ( 'NONE', *, *, #43788, .T. ) ;
#11102 = CARTESIAN_POINT ( 'NONE',  ( 766.7756240680305382, 9.467130982857780097, -361.5560724626415663 ) ) ;
#11103 = CARTESIAN_POINT ( 'NONE',  ( 751.6929314249748586, -294.9982390220560546, 318.8095938919659034 ) ) ;
#11104 = CARTESIAN_POINT ( 'NONE',  ( 989.9999999999992042, -422.8782571739196783, -207.4246812887968190 ) ) ;
#11105 = CARTESIAN_POINT ( 'NONE',  ( -728.8365100919714905, 258.0940000000001646, -206.1189999999890574 ) ) ;
#11106 = CARTESIAN_POINT ( 'NONE',  ( 800.9840315886518738, -172.9181544815165239, 354.1144889064786412 ) ) ;
#11107 = CARTESIAN_POINT ( 'NONE',  ( 765.0180583372156207, -48.99823902205675807, 360.0135310231089534 ) ) ;
#11108 = ORIENTED_EDGE ( 'NONE', *, *, #23827, .F. ) ;
#11109 = CARTESIAN_POINT ( 'NONE',  ( 773.7305795820266212, -417.2817908451522158, -374.8230680027170365 ) ) ;
#11110 = CARTESIAN_POINT ( 'NONE',  ( 748.9653473494365699, -2.634602658420536425, -356.9462024416520762 ) ) ;
#11111 = CARTESIAN_POINT ( 'NONE',  ( 764.1737431748507561, -274.3726999360617356, 371.6461892240376415 ) ) ;
#11112 = CARTESIAN_POINT ( 'NONE',  ( 784.0799538623451781, -227.8055962898687596, 364.6971507214555572 ) ) ;
#11113 = CARTESIAN_POINT ( 'NONE',  ( 764.8639956371174549, -368.0891481129647786, -319.7806653035542013 ) ) ;
#11114 = EDGE_CURVE ( 'NONE', #34493, #30414, #9551, .T. ) ;
#11115 = CARTESIAN_POINT ( 'NONE',  ( 759.9864689768902508, -2.089148112965993231, 354.9819416627836404 ) ) ;
#11116 = CARTESIAN_POINT ( 'NONE',  ( 799.9999999999993179, 212.6707680665973612, -236.5295014342203785 ) ) ;
#11117 = CARTESIAN_POINT ( 'NONE',  ( 786.5483106153019435, -223.6454272087891013, -364.1601925771022366 ) ) ;
#11118 = CARTESIAN_POINT ( 'NONE',  ( 787.4397851343537695, -21.72551174932956641, 374.2001403089903988 ) ) ;
#11119 = CARTESIAN_POINT ( 'NONE',  ( 746.8695393053150156, -125.9073299311474159, 327.6429770376306010 ) ) ;
#11120 = FACE_OUTER_BOUND ( 'NONE', #25006, .T. ) ;
#11121 = CARTESIAN_POINT ( 'NONE',  ( 811.0346526505617248, -446.6346026584191122, -323.0537975583478101 ) ) ;
#11122 = DIRECTION ( 'NONE',  ( 8.326672684688676025E-16, 1.000000000000000000, -0.000000000000000000 ) ) ;
#11123 = CARTESIAN_POINT ( 'NONE',  ( 754.3581564841646241, -353.4636090269705733, 316.1443688327762516 ) ) ;
#11124 = CARTESIAN_POINT ( 'NONE',  ( 779.9999999999992042, 126.4563064324884465, 370.0000000000000568 ) ) ;
#11125 = CARTESIAN_POINT ( 'NONE',  ( 754.9967657858570647, -337.5436935675102177, 365.0032342141425374 ) ) ;
#11126 = CARTESIAN_POINT ( 'NONE',  ( 796.7737145352015204, -44.63460265842040542, -370.7187646348536987 ) ) ;
#11127 = CARTESIAN_POINT ( 'NONE',  ( 759.7806653035534055, -294.9982390220560546, -324.8639956371180801 ) ) ;
#11128 = CARTESIAN_POINT ( 'NONE',  ( 787.4999999999992042, -512.9681489794448908, -329.9999999999999432 ) ) ;
#11129 = CARTESIAN_POINT ( 'NONE',  ( 771.1735550268778070, -441.1800572038735027, 316.3353852180827630 ) ) ;
#11130 = CARTESIAN_POINT ( 'NONE',  ( 805.2837595273609850, -194.7363362996982517, 340.5290396650784714 ) ) ;
#11131 = CARTESIAN_POINT ( 'NONE',  ( 795.8262568251477660, -70.37269993606230400, -308.3538107759623585 ) ) ;
#11132 = CARTESIAN_POINT ( 'NONE',  ( 758.6633372737375112, -92.53286901714190549, -326.9102291470432533 ) ) ;
#11133 = CARTESIAN_POINT ( 'NONE',  ( 800.1688906516307043, -106.1692326535054889, 369.0717654672308186 ) ) ;
#11134 = CARTESIAN_POINT ( 'NONE',  ( 762.3223304703356007, -415.5436935675102177, 322.3223304703362828 ) ) ;
#11135 = ADVANCED_FACE ( 'NONE', ( #20123 ), #24902, .T. ) ;
#11136 = CARTESIAN_POINT ( 'NONE',  ( 781.8018195045266339, 1.729033705215812011, -365.1927285166406705 ) ) ;
#11138 = EDGE_LOOP ( 'NONE', ( #25224, #19000 ) ) ;
#11137 = CARTESIAN_POINT ( 'NONE',  ( 805.0264073115434940, -102.3510508353236901, -339.4763451958999099 ) ) ;
#11139 = CARTESIAN_POINT ( 'NONE',  ( 774.6312213355099630, -95.36187538569294020, -364.6798772138717482 ) ) ;
#11140 = EDGE_CURVE ( 'NONE', #15121, #26522, #13214, .T. ) ;
#11141 = CARTESIAN_POINT ( 'NONE',  ( 763.2154366446407039, -405.6237781080500326, -321.4292242960311228 ) ) ;
#11143 = CARTESIAN_POINT ( 'NONE',  ( 767.8955696845334842, -216.4527844766016926, 362.1676090361161755 ) ) ;
#11142 = CARTESIAN_POINT ( 'NONE',  ( 774.6858677611749044, -225.7255117493289163, 315.5713283507209894 ) ) ;
#11144 = CARTESIAN_POINT ( 'NONE',  ( 744.9990715423526808, -402.3510508353228374, -341.2370466360926002 ) ) ;
#11145 = DIRECTION ( 'NONE',  ( 1.000000000000000000, 0.000000000000000000, 0.000000000000000000 ) ) ;
#11146 = EDGE_LOOP ( 'NONE', ( #30743, #44882, #5913, #30986 ) ) ;
#11147 = CARTESIAN_POINT ( 'NONE',  ( 781.8018195045266339, -430.2709662947827383, 365.1927285166406705 ) ) ;
#11148 = VERTEX_POINT ( 'NONE', #32060 ) ;
#11149 =( NAMED_UNIT ( * ) SI_UNIT ( $, .STERADIAN. ) SOLID_ANGLE_UNIT ( ) );
#11150 = EDGE_CURVE ( 'NONE', #14103, #7469, #9287, .T. ) ;
#11151 = CARTESIAN_POINT ( 'NONE',  ( 748.9653473494363425, -242.6346026584197659, -356.9462024416521331 ) ) ;
#11152 = CARTESIAN_POINT ( 'NONE',  ( 772.5602148656447525, -177.7255117493290868, 305.7998596910095443 ) ) ;
#11153 = CARTESIAN_POINT ( 'NONE',  ( 805.2837595273609850, -266.7363362996981095, 340.5290396650784714 ) ) ;
#11154 = VERTEX_POINT ( 'NONE', #42464 ) ;
#11155 = CARTESIAN_POINT ( 'NONE',  ( 775.8780910478218402, -81.28179084515319630, -364.9511171171680530 ) ) ;
#11156 = CARTESIAN_POINT ( 'NONE',  ( 815.0009284576459549, -198.3510508353234059, 338.7629533639073429 ) ) ;
#11157 = CARTESIAN_POINT ( 'NONE',  ( 803.4237431249931660, -255.1800572038742700, -331.2633955100225194 ) ) ;
#11158 = VERTEX_POINT ( 'NONE', #34446 ) ;
#11159 = CARTESIAN_POINT ( 'NONE',  ( 788.7366044899766848, -347.9073299311467053, -316.5762568750059813 ) ) ;
#11160 = CARTESIAN_POINT ( 'NONE',  ( 781.7834795799800531, -58.81642084023854267, -315.0636971347436202 ) ) ;
#11161 = CARTESIAN_POINT ( 'NONE',  ( 804.9511171171677688, -245.8055962898686460, 335.8780910478229202 ) ) ;
#11162 = CARTESIAN_POINT ( 'NONE',  ( 831.1634899080286232, 259.9999999999998863, -193.8809999999999718 ) ) ;
#11163 = DIRECTION ( 'NONE',  ( -0.000000000000000000, -0.6438296778008192334, -0.7651688349527135946 ) ) ;
#11164 = EDGE_LOOP ( 'NONE', ( #36484, #27374, #33300, #20784, #27661, #44663 ) ) ;
#11165 = CARTESIAN_POINT ( 'NONE',  ( 803.4237431249931660, -15.18005720387504631, -331.2633955100225194 ) ) ;
#11166 = CYLINDRICAL_SURFACE ( 'NONE', #38801, 30.00000000000002842 ) ;
#11167 = DIRECTION ( 'NONE',  ( -0.000000000000000000, -0.6438296778008192334, -0.7651688349527135946 ) ) ;
#11168 = ORIENTED_EDGE ( 'NONE', *, *, #10888, .F. ) ;
#11169 = CARTESIAN_POINT ( 'NONE',  ( 778.7629533639073998, -272.7363362996981095, -375.0009284576466371 ) ) ;
#11170 = EDGE_CURVE ( 'NONE', #38205, #20464, #41385, .T. ) ;
#11171 = CARTESIAN_POINT ( 'NONE',  ( 757.7880784355613741, -186.0090635724255890, 312.4576283171834916 ) ) ;
#11173 = CARTESIAN_POINT ( 'NONE',  ( 758.0580252608178853, -246.4527844766016074, -328.0187753319985404 ) ) ;
#11172 = CARTESIAN_POINT ( 'NONE',  ( -28.63011601220122415, -501.1515549466498669, -368.0974687824633520 ) ) ;
#11174 = EDGE_CURVE ( 'NONE', #16202, #22885, #23798, .T. ) ;
#11175 =( LENGTH_UNIT ( ) NAMED_UNIT ( * ) SI_UNIT ( .MILLI., .METRE. ) );
#11176 = CARTESIAN_POINT ( 'NONE',  ( 783.0745993439762742, -104.1908817542440175, -365.1016975059196739 ) ) ;
#11177 = EDGE_CURVE ( 'NONE', #1691, #38523, #23356, .T. ) ;
#11178 = CARTESIAN_POINT ( 'NONE',  ( 810.4231160770870019, -384.5545181178795247, 321.9338519418446936 ) ) ;
#11179 = CARTESIAN_POINT ( 'NONE',  ( 998.9999999999992042, -600.0000000000001137, 360.0000000000000000 ) ) ;
#11180 = CARTESIAN_POINT ( 'NONE',  ( 787.4397851343537695, -309.7255117493287457, -374.2001403089903988 ) ) ;
#11181 = DIRECTION ( 'NONE',  ( 0.000000000000000000, 0.000000000000000000, 1.000000000000000000 ) ) ;
#11182 = CARTESIAN_POINT ( 'NONE',  ( 804.9363028652555840, -16.27096629478413092, 338.2165204200192079 ) ) ;
#11183 = CARTESIAN_POINT ( 'NONE',  ( 805.6418435158337843, -245.4636090269709143, 363.8556311672236916 ) ) ;
#11184 = CARTESIAN_POINT ( 'NONE',  ( 768.8385539511368734, -191.2601417444143976, -306.4236121716840557 ) ) ;
#11185 = CARTESIAN_POINT ( 'NONE',  ( 792.2312462859673587, -227.9073299311471033, 307.2067596250082602 ) ) ;
#11186 = CARTESIAN_POINT ( 'NONE',  ( 796.9462024416508257, -444.4527844766009821, -308.9653473494370246 ) ) ;
#11187 = LINE ( 'NONE', #42362, #11413 ) ;
#11188 = CARTESIAN_POINT ( 'NONE',  ( 759.7806653035534055, -318.9982390220557704, 324.8639956371180801 ) ) ;
#11189 = CARTESIAN_POINT ( 'NONE',  ( 757.4527132478984868, -88.37269993606226137, 329.1273215169538844 ) ) ;
#11190 = CARTESIAN_POINT ( 'NONE',  ( 776.9254006560222479, -92.19088175424406018, 314.8983024940802125 ) ) ;
#11191 = CARTESIAN_POINT ( 'NONE',  ( 766.7756240680305382, 9.467130982857780097, -361.5560724626415663 ) ) ;
#11192 = DIRECTION ( 'NONE',  ( -1.880165489482579047E-16, -1.000000000000000000, 0.000000000000000000 ) ) ;
#11193 = EDGE_CURVE ( 'NONE', #43717, #40029, #30982, .T. ) ;
#11194 = DIRECTION ( 'NONE',  ( -1.000000000000000000, -0.000000000000000000, 0.000000000000000000 ) ) ;
#11196 = CARTESIAN_POINT ( 'NONE',  ( 768.0187753319979720, -344.6346026584195101, 318.0580252608186242 ) ) ;
#11195 = CARTESIAN_POINT ( 'NONE',  ( 756.7813123517142913, -163.9874144716871456, 329.9779781133712504 ) ) ;
#11197 = VERTEX_POINT ( 'NONE', #37458 ) ;
#11198 = EDGE_CURVE ( 'NONE', #36235, #16032, #28514, .T. ) ;
#11199 = CARTESIAN_POINT ( 'NONE',  ( 763.2154366446407039, -285.6237781080502600, -321.4292242960311228 ) ) ;
#11200 = UNCERTAINTY_MEASURE_WITH_UNIT (LENGTH_MEASURE( 1.000000000000000082E-05 ), #7908, 'distance_accuracy_value', 'NONE');
#11201 = CARTESIAN_POINT ( 'NONE',  ( 791.9812246680005501, -116.6346026584201780, 361.9419747391813189 ) ) ;
#11202 = CARTESIAN_POINT ( 'NONE',  ( 744.9990715423526808, -306.3510508353230648, -341.2370466360926002 ) ) ;
#11203 = DIRECTION ( 'NONE',  ( -1.880165489482579047E-16, -1.000000000000000000, -0.000000000000000000 ) ) ;
#11204 = CARTESIAN_POINT ( 'NONE',  ( 808.3070685750230950, 5.001760977943074948, 361.1904061080339261 ) ) ;
#11205 = ORIENTED_EDGE ( 'NONE', *, *, #34603, .F. ) ;
#11206 = CARTESIAN_POINT ( 'NONE',  ( 795.1360043628807261, -308.0891481129650629, 360.2193346964456282 ) ) ;
#11207 = CARTESIAN_POINT ( 'NONE',  ( 761.2382568024794409, -63.62377810805107714, -356.9571628226838129 ) ) ;
#11208 = CARTESIAN_POINT ( 'NONE',  ( 801.9419747391806368, -162.4527844766018632, -351.9812246680014027 ) ) ;
#11209 = CARTESIAN_POINT ( 'NONE',  ( 768.0187753319979720, -440.6346026584191122, 318.0580252608186242 ) ) ;
#11210 = EDGE_CURVE ( 'NONE', #30506, #19677, #7139, .T. ) ;
#11211 = CARTESIAN_POINT ( 'NONE',  ( 811.0346526505616112, -134.6346026584201070, -323.0537975583477532 ) ) ;
#11212 = PRODUCT_RELATED_PRODUCT_CATEGORY ( 'part', '', ( #13724 ) ) ;
#11213 = EDGE_LOOP ( 'NONE', ( #3071, #12666, #34020, #1315 ) ) ;
#11214 = PRESENTATION_LAYER_ASSIGNMENT (  '', '', ( #42162 ) ) ;
#11215 = CARTESIAN_POINT ( 'NONE',  ( 788.7366044899766848, -155.9073299311473306, -316.5762568750059813 ) ) ;
#11216 = ORIENTED_EDGE ( 'NONE', *, *, #24165, .T. ) ;
#11217 = CARTESIAN_POINT ( 'NONE',  ( 776.9254006560222479, -380.1908817542431507, -314.8983024940802125 ) ) ;
#11218 = CARTESIAN_POINT ( 'NONE',  ( 771.1735550268778070, -9.180057203875058747, 316.3353852180827630 ) ) ;
#11219 = CARTESIAN_POINT ( 'NONE',  ( 759.2295555964440155, -136.1692326535053894, 353.9708237608231229 ) ) ;
#11222 = CARTESIAN_POINT ( 'NONE',  ( 759.8311093483677041, -406.1692326535045368, 310.9282345327691814 ) ) ;
#11221 = DIRECTION ( 'NONE',  ( -0.000000000000000000, 1.000000000000000000, -0.000000000000000000 ) ) ;
#11220 = FACE_OUTER_BOUND ( 'NONE', #29159, .T. ) ;
#11223 = VERTEX_POINT ( 'NONE', #35299 ) ;
#11224 = CARTESIAN_POINT ( 'NONE',  ( 804.4086373105744769, -385.6454272087888171, -333.3843516231986541 ) ) ;
#11225 = LINE ( 'NONE', #369, #17442 ) ;
#11226 = CARTESIAN_POINT ( 'NONE',  ( 797.8822607201568644, -174.5545181178801784, -370.1134526219340160 ) ) ;
#11227 = CARTESIAN_POINT ( 'NONE',  ( 771.3260364891663130, -67.64542720878958448, 306.0683387631859773 ) ) ;
#11229 = CARTESIAN_POINT ( 'NONE',  ( 799.9999999999993179, 205.0000000000000568, -339.9999999999999432 ) ) ;
#11228 = LINE ( 'NONE', #1282, #39660 ) ;
#11230 = CARTESIAN_POINT ( 'NONE',  ( 801.3366627262608972, -344.5328690171410813, -353.0897708529566899 ) ) ;
#11231 = CARTESIAN_POINT ( 'NONE',  ( 778.1981804954714335, -442.2709662947826814, -314.8072714833589885 ) ) ;
#11232 = CARTESIAN_POINT ( 'NONE',  ( 805.6418435158337843, -197.4636090269709996, -363.8556311672236916 ) ) ;
#11233 = DIRECTION ( 'NONE',  ( 1.000000000000000000, 0.000000000000000000, 0.000000000000000000 ) ) ;
#11234 = LINE ( 'NONE', #42185, #10557 ) ;
#11235 = CARTESIAN_POINT ( 'NONE',  ( 790.9844846989617508, -358.3726999360613945, 317.2208543904092721 ) ) ;
#11236 = CARTESIAN_POINT ( 'NONE',  ( 802.2119215644370342, -342.0090635724251342, 367.5423716828165084 ) ) ;
#11237 = CARTESIAN_POINT ( 'NONE',  ( 745.7998596910086917, -221.3618753856925707, -332.5602148656461168 ) ) ;
#11238 = FACE_OUTER_BOUND ( 'NONE', #27164, .T. ) ;
#11239 = CARTESIAN_POINT ( 'NONE',  ( 785.3141322388236176, 2.274488250670355871, -364.4286716492789537 ) ) ;
#11240 = CARTESIAN_POINT ( 'NONE',  ( 799.9636004259356241, -142.9181544815166376, 311.2241431872006956 ) ) ;
#11241 = CARTESIAN_POINT ( 'NONE',  ( 811.6461892240364477, -100.7146871989600356, -324.1737431748509835 ) ) ;
#11242 = CARTESIAN_POINT ( 'NONE',  ( 758.8095938919642549, -128.0891481129655176, 311.6929314249763365 ) ) ;
#11243 = CARTESIAN_POINT ( 'NONE',  ( 777.5031285880264704, -334.8164208402376403, -374.9108240113588408 ) ) ;
#11244 = CARTESIAN_POINT ( 'NONE',  ( 879.9999999999992042, 249.9999999999998295, 360.0000000000000000 ) ) ;
#11245 = CARTESIAN_POINT ( 'NONE',  ( -775.4999999999993179, -355.4967352946684969, -16.45562775363632113 ) ) ;
#11246 = CARTESIAN_POINT ( 'NONE',  ( 802.1676090361156639, -230.6346026584197659, 327.8955696845344505 ) ) ;
#11247 = AXIS2_PLACEMENT_3D ( 'NONE', #15159, #32481, #35701 ) ;
#11248 = CARTESIAN_POINT ( 'NONE',  ( 804.6971507214547046, -3.281790845153435221, 344.0799538623459739 ) ) ;
#11249 = CARTESIAN_POINT ( 'NONE',  ( 761.9338519418445230, -398.5328690171409107, -370.4231160770881957 ) ) ;
#11250 = CARTESIAN_POINT ( 'NONE',  ( 805.0032342141412300, -421.5436935675101040, -314.9967657858571783 ) ) ;
#11251 = DIRECTION ( 'NONE',  ( -1.000000000000000000, -0.000000000000000000, -0.000000000000000000 ) ) ;
#11252 = CARTESIAN_POINT ( 'NONE',  ( 798.0661480581538854, -26.53286901714210799, 309.5768839229118043 ) ) ;
#11253 = EDGE_LOOP ( 'NONE', ( #42446, #22998 ) ) ;
#11254 = CARTESIAN_POINT ( 'NONE',  ( 790.8726784830453198, -178.7146871989598083, -362.5472867521010585 ) ) ;
#11255 = CARTESIAN_POINT ( 'NONE',  ( 804.9363028652555840, -40.27096629478405987, 338.2165204200192079 ) ) ;
#11256 = CARTESIAN_POINT ( 'NONE',  ( 776.2433038121456548, -204.8965053807779100, -374.8207195650711014 ) ) ;
#11257 = CARTESIAN_POINT ( 'NONE',  ( 803.8556311672234642, -297.6237781080502600, 365.6418435158340117 ) ) ;
#11258 = CARTESIAN_POINT ( 'NONE',  ( 805.1927285166399315, -160.8164208402382371, 341.8018195045277707 ) ) ;
#11259 = EDGE_LOOP ( 'NONE', ( #10938, #17160, #3548, #39111 ) ) ;
#11260 = CARTESIAN_POINT ( 'NONE',  ( 792.1044303154645831, -324.4527844766013231, 317.8323909638837677 ) ) ;
#11261 = CARTESIAN_POINT ( 'NONE',  ( 782.5225473063381969, -46.27096629478404566, -375.2698199232970637 ) ) ;
#11262 = VECTOR ( 'NONE', #7323, 1000.000000000000000 ) ;
#11263 = CARTESIAN_POINT ( 'NONE',  ( 763.2262854647970016, -80.63460265842029173, 309.2812353651462445 ) ) ;
#11264 = ORIENTED_EDGE ( 'NONE', *, *, #988, .F. ) ;
#11265 = CARTESIAN_POINT ( 'NONE',  ( 794.5607502887775127, -462.9631818684622999, -371.8524697363486666 ) ) ;
#11266 = VERTEX_POINT ( 'NONE', #7367 ) ;
#11267 = PRODUCT_CONTEXT ( 'NONE', #19019, 'mechanical' ) ;
#11269 = CARTESIAN_POINT ( 'NONE',  ( 799.2566176426618085, -384.0090635724249637, 324.0069404352559559 ) ) ;
#11268 = CARTESIAN_POINT ( 'NONE',  ( 771.2633955100217236, -47.90732993114767169, 363.4237431249939618 ) ) ;
#11270 = CARTESIAN_POINT ( 'NONE',  ( 771.1735550268778070, -297.1800572038740711, -316.3353852180827630 ) ) ;
#11272 = CARTESIAN_POINT ( 'NONE',  ( 801.9858362298568863, -291.0783235625957559, 312.7379699480935642 ) ) ;
#11271 = CARTESIAN_POINT ( 'NONE',  ( 745.7998596910086917, -389.3618753856919739, 332.5602148656461168 ) ) ;
#11273 = CARTESIAN_POINT ( 'NONE',  ( 746.7653713866222915, -65.26014174441471027, 351.0478386215610271 ) ) ;
#11274 = CARTESIAN_POINT ( 'NONE',  ( 755.8894580844503253, -303.8272453906071178, -332.3691319403863531 ) ) ;
#11275 = CARTESIAN_POINT ( 'NONE',  ( 805.1927285166397041, -304.8164208402376403, -341.8018195045277707 ) ) ;
#11276 = CYLINDRICAL_SURFACE ( 'NONE', #18434, 9.999999999999980460 ) ;
#11277 = CARTESIAN_POINT ( 'NONE',  ( 757.8323909638827445, -122.6346026584201354, -352.1044303154654358 ) ) ;
#11278 = LINE ( 'NONE', #42460, #11468 ) ;
#11279 = CARTESIAN_POINT ( 'NONE',  ( 744.7301800767019131, -388.8164208402374129, 337.4774526936615757 ) ) ;
#11281 = DIRECTION ( 'NONE',  ( -1.000000000000000000, -0.000000000000000000, 0.000000000000000000 ) ) ;
#11280 = LINE ( 'NONE', #32305, #5665 ) ;
#11282 = CARTESIAN_POINT ( 'NONE',  ( 814.8207195650702488, -74.19088175424410281, -336.2433038121456548 ) ) ;
#11283 = CARTESIAN_POINT ( 'NONE',  ( -28.63011601220122415, -513.1383975375929367, -369.9999999999999432 ) ) ;
#11284 = LINE ( 'NONE', #3679, #4629 ) ;
#11285 = CARTESIAN_POINT ( 'NONE',  ( 804.6971507214547046, -267.2817908451526137, 344.0799538623459739 ) ) ;
#11286 = CARTESIAN_POINT ( 'NONE',  ( 803.4237431249931660, -159.1800572038746111, 331.2633955100225194 ) ) ;
#11287 = ORIENTED_EDGE ( 'NONE', *, *, #34190, .T. ) ;
#11288 = CARTESIAN_POINT ( 'NONE',  ( 763.0428371773158460, -59.46360902697142592, -358.7617431975195359 ) ) ;
#11289 = CARTESIAN_POINT ( 'NONE',  ( 758.8095938919644823, -104.0891481129656739, -311.6929314249762797 ) ) ;
#11290 = CARTESIAN_POINT ( 'NONE',  ( 761.2382568024794409, -327.6237781080502600, 356.9571628226838129 ) ) ;
#11291 = FACE_OUTER_BOUND ( 'NONE', #24582, .T. ) ;
#11292 = CARTESIAN_POINT ( 'NONE',  ( 807.2620300519052989, -48.00906357242602951, 318.0141637701419768 ) ) ;
#11293 = CARTESIAN_POINT ( 'NONE',  ( 767.7687537140311633, -239.9073299311470748, -372.7932403749916830 ) ) ;
#11294 = CARTESIAN_POINT ( 'NONE',  ( 746.8695393053150156, -197.9073299311472169, 327.6429770376306010 ) ) ;
#11295 = CARTESIAN_POINT ( 'NONE',  ( 764.8639956371174549, -104.0891481129656881, 319.7806653035542013 ) ) ;
#11296 = VECTOR ( 'NONE', #26217, 1000.000000000000000 ) ;
#11297 = DIRECTION ( 'NONE',  ( 0.000000000000000000, 0.000000000000000000, 1.000000000000000000 ) ) ;
#11298 = CARTESIAN_POINT ( 'NONE',  ( 815.0009284576459549, -294.3510508353230648, -338.7629533639073429 ) ) ;
#11299 = CARTESIAN_POINT ( 'NONE',  ( 796.7737145352015204, -332.6346026584195101, -370.7187646348536987 ) ) ;
#11300 = CARTESIAN_POINT ( 'NONE',  ( 746.4236121716829757, -447.8272453906067199, 328.8385539511384650 ) ) ;
#11301 = CARTESIAN_POINT ( 'NONE',  ( 801.1904061080336987, -332.0891481129649492, -368.3070685750235498 ) ) ;
#11302 = CARTESIAN_POINT ( 'NONE',  ( -78.83651009197140525, 240.0000000000000568, -202.7499999999934346 ) ) ;
#11303 = CARTESIAN_POINT ( 'NONE',  ( 761.2382568024794409, -351.6237781080502032, 356.9571628226838129 ) ) ;
#11304 = CARTESIAN_POINT ( 'NONE',  ( 815.2698199232962679, -64.81642084023852135, 342.5225473063383674 ) ) ;
#11305 = CARTESIAN_POINT ( 'NONE',  ( 762.3223304703356007, -415.5436935675102177, -322.3223304703362828 ) ) ;
#11306 = CARTESIAN_POINT ( 'NONE',  ( 754.9735926884551418, -42.35105083532388193, 340.5236548041000333 ) ) ;
#11307 = CARTESIAN_POINT ( 'NONE',  ( 759.7806653035534055, -198.9982390220562252, -324.8639956371180801 ) ) ;
#11308 = EDGE_CURVE ( 'NONE', #10247, #1373, #21443, .T. ) ;
#11309 = CARTESIAN_POINT ( 'NONE',  ( 764.3348316497523456, -94.71468719896007826, -308.6759233522265617 ) ) ;
#11310 = CARTESIAN_POINT ( 'NONE',  ( 756.1443688327750579, -189.6237781080507148, 314.3581564841659315 ) ) ;
#11311 = CARTESIAN_POINT ( 'NONE',  ( 758.0580252608178853, -54.45278447660219001, 328.0187753319985404 ) ) ;
#11312 = ORIENTED_EDGE ( 'NONE', *, *, #12291, .F. ) ;
#11313 = CARTESIAN_POINT ( 'NONE',  ( 783.0433043558608688, -240.8965053807777963, -315.1538015810313027 ) ) ;
#11314 = CARTESIAN_POINT ( 'NONE',  ( 803.4237431249931660, -183.1800572038744974, 331.2633955100225194 ) ) ;
#11315 = CARTESIAN_POINT ( 'NONE',  ( 795.6651683502461765, -34.71468719896025590, -371.3240766477733814 ) ) ;
#11316 = CARTESIAN_POINT ( 'NONE',  ( 788.7366044899766848, -347.9073299311467053, 316.5762568750059813 ) ) ;
#11317 = DIRECTION ( 'NONE',  ( 0.000000000000000000, -1.000000000000000000, 0.000000000000000000 ) ) ;
#11318 = LINE ( 'NONE', #25162, #7264 ) ;
#11319 = ORIENTED_EDGE ( 'NONE', *, *, #9197, .F. ) ;
#11320 = CARTESIAN_POINT ( 'NONE',  ( 770.0799878456142551, -37.98741447168752927, 362.9823548866085616 ) ) ;
#11321 = CARTESIAN_POINT ( 'NONE',  ( 788.6739635108323228, -343.6454272087887603, -373.9316612368139090 ) ) ;
#11322 = CARTESIAN_POINT ( 'NONE',  ( 801.1904061080338124, -308.0891481129650629, 368.3070685750236066 ) ) ;
#11323 = CARTESIAN_POINT ( 'NONE',  ( 781.2497674668890113, 11.64894916467595642, 375.3608509340180603 ) ) ;
#11324 = CARTESIAN_POINT ( 'NONE',  ( 786.5483106153019435, -199.6454272087891582, -364.1601925771022366 ) ) ;
#11325 = CARTESIAN_POINT ( 'NONE',  ( 800.2193346964447755, -186.9982390220563104, -355.1360043628815788 ) ) ;
#11326 = AXIS2_PLACEMENT_3D ( 'NONE', #2713, #13803, #20491 ) ;
#11327 = CARTESIAN_POINT ( 'NONE',  ( 759.7806653035535192, -366.9982390220557136, -324.8639956371181370 ) ) ;
#11328 = VERTEX_POINT ( 'NONE', #14980 ) ;
#11329 = CARTESIAN_POINT ( 'NONE',  ( 803.8651313633788504, 18.73985825558501972, -332.4468031744301015 ) ) ;
#11330 = CARTESIAN_POINT ( 'NONE',  ( 814.5518280994195948, -303.7255117493287457, 332.4837098697145734 ) ) ;
#11331 = DIRECTION ( 'NONE',  ( 0.000000000000000000, 0.000000000000000000, 1.000000000000000000 ) ) ;
#11332 = CARTESIAN_POINT ( 'NONE',  ( 786.6156483768007774, -361.4419599262319593, 315.5913626894246136 ) ) ;
#11333 = DIRECTION ( 'NONE',  ( 0.000000000000000000, 0.000000000000000000, 1.000000000000000000 ) ) ;
#11334 = CARTESIAN_POINT ( 'NONE',  ( 758.4439275373578084, -156.5545181178802636, 353.2243759319684386 ) ) ;
#11335 = CARTESIAN_POINT ( 'NONE',  ( 803.4237431249931660, -63.18005720387488822, 331.2633955100225194 ) ) ;
#11336 = ORIENTED_EDGE ( 'NONE', *, *, #44934, .F. ) ;
#11337 = CARTESIAN_POINT ( 'NONE',  ( 745.7194118038753459, -421.6454272087885329, -348.7631598425976449 ) ) ;
#11338 = CARTESIAN_POINT ( 'NONE',  ( 812.7932403749906598, 8.819942796124882634, -327.7687537140311633 ) ) ;
#11339 = CARTESIAN_POINT ( 'NONE',  ( 745.1792804349281596, -254.1908817542435770, 343.7566961878542884 ) ) ;
#11340 = CARTESIAN_POINT ( 'NONE',  ( 803.2186876482843445, -223.9874144716869182, 350.0220218866286928 ) ) ;
#11341 = CARTESIAN_POINT ( 'NONE',  ( 804.6798772138708955, -351.7255117493284047, -334.6312213355107019 ) ) ;
#11342 = CARTESIAN_POINT ( 'NONE',  ( 774.6858677611749044, 14.27448825067031812, -315.5713283507209894 ) ) ;
#11343 = CIRCLE ( 'NONE', #34901, 20.00000000000001776 ) ;
#11344 = CARTESIAN_POINT ( 'NONE',  ( 804.8461984189677878, -458.1908817542429802, 336.9566956441385628 ) ) ;
#11345 = DIRECTION ( 'NONE',  ( -1.058954862565134068E-16, 0.6438296778008191223, 0.7651688349527137056 ) ) ;
#11346 = CARTESIAN_POINT ( 'NONE',  ( 772.4468031744293057, -273.8272453906071746, -363.8651313633793620 ) ) ;
#11347 = CARTESIAN_POINT ( 'NONE',  ( 751.6929314249748586, -6.998239022056885972, 318.8095938919659034 ) ) ;
#11348 = CARTESIAN_POINT ( 'NONE',  ( 813.1304606946830518, -113.9073299311474301, 352.3570229623690580 ) ) ;
#11349 = FACE_OUTER_BOUND ( 'NONE', #36146, .T. ) ;
#11350 = DIRECTION ( 'NONE',  ( 0.000000000000000000, 0.000000000000000000, 1.000000000000000000 ) ) ;
#11351 = CARTESIAN_POINT ( 'NONE',  ( 750.9282345327678740, -376.9181544815159555, 319.8311093483690115 ) ) ;
#11352 = CARTESIAN_POINT ( 'NONE',  ( -775.4999999999993179, -544.8427095258973623, -350.0000000000000000 ) ) ;
#11353 = CARTESIAN_POINT ( 'NONE',  ( 758.8095938919642549, -344.0891481129647786, 311.6929314249763365 ) ) ;
#11354 = ADVANCED_FACE ( 'NONE', ( #22125 ), #36437, .F. ) ;
#11355 = CARTESIAN_POINT ( 'NONE',  ( 788.8264449731200330, -333.1800572038740142, -363.6646147819171233 ) ) ;
#11356 = CARTESIAN_POINT ( 'NONE',  ( 791.4716058693660443, -452.9681489794448339, -367.7200696026887954 ) ) ;
#11357 = CARTESIAN_POINT ( 'NONE',  ( 785.3687786644884454, -443.3618753856917465, 315.3201227861279676 ) ) ;
#11358 = VECTOR ( 'NONE', #40549, 1000.000000000000114 ) ;
#11359 = CIRCLE ( 'NONE', #23860, 2.749999999999863665 ) ;
#11360 = CARTESIAN_POINT ( 'NONE',  ( 801.5560724626406000, -192.5545181178801215, 326.7756240680316182 ) ) ;
#11361 = CARTESIAN_POINT ( 'NONE',  ( 810.4231160770870019, -72.55451811788049099, -321.9338519418446936 ) ) ;
#11362 = CARTESIAN_POINT ( 'NONE',  ( 787.6308680596127942, -83.26014174441466764, -364.1105419155492768 ) ) ;
#11363 = CARTESIAN_POINT ( 'NONE',  ( 811.6461892240364477, -100.7146871989600356, 324.1737431748509835 ) ) ;
#11364 = CARTESIAN_POINT ( 'NONE',  ( 755.0636971347428243, -436.2709662947827951, 341.7834795799807353 ) ) ;
#11365 = CARTESIAN_POINT ( 'NONE',  ( 759.7806653035534055, -6.998239022056885972, -324.8639956371180801 ) ) ;
#11366 = ORIENTED_EDGE ( 'NONE', *, *, #14813, .T. ) ;
#11367 = CARTESIAN_POINT ( 'NONE',  ( 771.1735550268778070, -105.1800572038747248, -316.3353852180827630 ) ) ;
#11368 = CARTESIAN_POINT ( 'NONE',  ( 789.9200121543843807, -409.9874144716863498, -317.0176451133914384 ) ) ;
#11370 = CARTESIAN_POINT ( 'NONE',  ( 759.9864689768902508, -242.0891481129652618, 354.9819416627836404 ) ) ;
#11369 = CARTESIAN_POINT ( 'NONE',  ( 802.1676090361156639, -278.6346026584196807, 327.8955696845344505 ) ) ;
#11371 = LINE ( 'NONE', #14388, #20500 ) ;
#11372 = VERTEX_POINT ( 'NONE', #8062 ) ;
#11373 = CARTESIAN_POINT ( 'NONE',  ( 755.5713283507202505, -437.3618753856919170, 334.6858677611754729 ) ) ;
#11374 = VECTOR ( 'NONE', #4689, 1000.000000000000000 ) ;
#11375 = ORIENTED_EDGE ( 'NONE', *, *, #6060, .F. ) ;
#11376 = CARTESIAN_POINT ( 'NONE',  ( 744.7301800767020268, -172.8164208402381519, 337.4774526936615189 ) ) ;
#11377 = CARTESIAN_POINT ( 'NONE',  ( 796.1575198192839480, -270.0090635724253048, 359.4546378042384163 ) ) ;
#11378 = EDGE_CURVE ( 'NONE', #17860, #2952, #5654, .T. ) ;
#11379 = ORIENTED_EDGE ( 'NONE', *, *, #27521, .T. ) ;
#11380 = CARTESIAN_POINT ( 'NONE',  ( 758.4439275373578084, -84.55451811788046257, -353.2243759319684386 ) ) ;
#11381 = CARTESIAN_POINT ( 'NONE',  ( 754.0944755984390895, -231.6237781080504874, 364.1009440267246760 ) ) ;
#11382 = CARTESIAN_POINT ( 'NONE',  ( 756.3353852180820240, -245.9073299311469896, -331.1735550268787733 ) ) ;
#11383 = ORIENTED_EDGE ( 'NONE', *, *, #44462, .T. ) ;
#11384 = CARTESIAN_POINT ( 'NONE',  ( 762.3223304703356007, -391.5436935675101608, -322.3223304703362828 ) ) ;
#11385 = CARTESIAN_POINT ( 'NONE',  ( 754.8072714833581358, -52.81642084023856398, -338.1981804954720587 ) ) ;
#11386 = CARTESIAN_POINT ( 'NONE',  ( 787.6308680596127942, -275.2601417444140566, 364.1105419155492768 ) ) ;
#11387 = CYLINDRICAL_SURFACE ( 'NONE', #1168, 2.749999999999863665 ) ;
#11388 = CARTESIAN_POINT ( 'NONE',  ( -468.8365100919714337, 260.0000000000001705, -199.9999999999908766 ) ) ;
#11389 = VECTOR ( 'NONE', #12073, 1000.000000000000000 ) ;
#11390 = CARTESIAN_POINT ( 'NONE',  ( 803.6646147819161570, -17.90732993114776406, -348.8264449731210561 ) ) ;
#11391 = DIRECTION ( 'NONE',  ( 0.000000000000000000, -0.000000000000000000, -1.000000000000000000 ) ) ;
#11392 = VERTEX_POINT ( 'NONE', #5034 ) ;
#11393 = CARTESIAN_POINT ( 'NONE',  ( 797.8822607201568644, -294.5545181178797520, -370.1134526219340160 ) ) ;
#11394 = CIRCLE ( 'NONE', #25396, 9.999999999999982236 ) ;
#11395 = CARTESIAN_POINT ( 'NONE',  ( 755.8990559732751535, -155.4636090269711417, 365.9055244015606831 ) ) ;
#11397 = CARTESIAN_POINT ( 'NONE',  ( 762.3223304703356007, -271.5436935675106156, -322.3223304703362828 ) ) ;
#11396 = DIRECTION ( 'NONE',  ( -1.000000000000000000, -0.000000000000000000, -0.000000000000000000 ) ) ;
#11398 = DIRECTION ( 'NONE',  ( -1.880165489482579047E-16, -1.000000000000000000, -0.000000000000000000 ) ) ;
#11399 = CARTESIAN_POINT ( 'NONE',  ( 766.9102291470427417, -138.5545181178802636, -318.6633372737382501 ) ) ;
#11400 = EDGE_CURVE ( 'NONE', #41469, #8307, #36213, .T. ) ;
#11401 = CARTESIAN_POINT ( 'NONE',  ( 746.4999999999993179, -365.3551492539851893, -28.13243251470704109 ) ) ;
#11402 = CARTESIAN_POINT ( 'NONE',  ( 781.2497674668890113, -12.35105083532396897, -375.3608509340180603 ) ) ;
#11403 = CARTESIAN_POINT ( 'NONE',  ( 782.4968714119720516, -346.8164208402376971, -305.0891759886411023 ) ) ;
#11404 = CARTESIAN_POINT ( 'NONE',  ( 521.6730038022808458, 230.0000000000002274, 339.9999999999999432 ) ) ;
#11405 = CARTESIAN_POINT ( 'NONE',  ( 758.0580252608178853, -6.452784476602343666, 328.0187753319985404 ) ) ;
#11406 = AXIS2_PLACEMENT_3D ( 'NONE', #40174, #12225, #1372 ) ;
#11407 = CARTESIAN_POINT ( 'NONE',  ( 766.4474001241216001, -283.0999726633344267, 307.3154664389482491 ) ) ;
#11408 = CARTESIAN_POINT ( 'NONE',  ( 759.8311093483677041, -214.1692326535052189, -310.9282345327691814 ) ) ;
#11409 = CARTESIAN_POINT ( 'NONE',  ( 792.3570229623688874, -237.1800572038742985, 373.1304606946836202 ) ) ;
#11410 = CARTESIAN_POINT ( 'NONE',  ( 759.0252816721024374, -0.9982390220569063999, -368.0189434323527280 ) ) ;
#11411 = EDGE_CURVE ( 'NONE', #36456, #8317, #43153, .T. ) ;
#11412 = DIRECTION ( 'NONE',  ( -0.000000000000000000, -0.000000000000000000, 1.000000000000000000 ) ) ;
#11413 = VECTOR ( 'NONE', #24810, 1000.000000000000000 ) ;
#11414 = DIRECTION ( 'NONE',  ( -1.000000000000000000, 0.000000000000000000, -0.000000000000000000 ) ) ;
#11415 = CARTESIAN_POINT ( 'NONE',  ( 758.0580252608178853, -318.4527844766014368, 328.0187753319985404 ) ) ;
#11416 = CARTESIAN_POINT ( 'NONE',  ( 793.9708237608222134, -94.91815448151677970, 319.2295555964448681 ) ) ;
#11417 = CARTESIAN_POINT ( 'NONE',  ( 797.8594530101008786, -445.5436935675098766, -322.1405469898980982 ) ) ;
#11418 = FACE_OUTER_BOUND ( 'NONE', #535, .T. ) ;
#11419 = DIRECTION ( 'NONE',  ( -1.000000000000000000, -4.625929269271485914E-16, 0.000000000000000000 ) ) ;
#11421 = CARTESIAN_POINT ( 'NONE',  ( 762.1405469898971887, -361.5436935675103882, 357.8594530101015607 ) ) ;
#11420 = CARTESIAN_POINT ( 'NONE',  ( 795.9930595647434757, -147.0783235625962959, 320.7433823573372820 ) ) ;
#11422 = VERTEX_POINT ( 'NONE', #28835 ) ;
#11423 = CLOSED_SHELL ( 'NONE', ( #6698, #36248, #20743, #36281, #34905, #27494, #43570, #9430, #15719, #9734, #10028, #3510, #44780, #457, #35494, #38156, #36856, #32036, #12495, #8943, #8544, #29549, #24076, #25232, #39746, #41925, #26692, #32290, #10791, #3858, #11998, #2695, #39368, #18093, #32108, #35370, #29138, #13392, #40304, #41964, #5431, #5761, #25253, #13139, #22387, #25015, #43003, #622, #39984, #5757, #35720, #41395, #4947, #30690, #31450, #24426, #44186, #20762, #18479, #22604, #24121, #28696, #26310, #38857, #11985, #746, #38787, #30113, #26143, #9468, #41041, #22772, #1338, #21364, #18251, #18816, #32321, #24106, #40782, #675, #44157, #10958, #30266, #38734, #19870, #40220, #970, #26097, #24052, #42532, #12826, #34846, #20643, #16806, #18789, #19029, #4670, #41534, #20975, #7699, #27691, #33164, #35703, #12565 ) ) ;
#11424 = CARTESIAN_POINT ( 'NONE',  ( 784.0799538623451781, -299.8055962898685038, -364.6971507214555572 ) ) ;
#11425=STYLED_ITEM('',(#45744),#2862);
#11426 = CARTESIAN_POINT ( 'NONE',  ( 771.2368401574024119, -277.4419599262322436, -374.2805881961240857 ) ) ;
#11427 = CARTESIAN_POINT ( 'NONE',  ( 786.4999999999993179, -544.8427095258973623, -350.0000000000000000 ) ) ;
#11428 = CARTESIAN_POINT ( 'NONE',  ( 813.1304606946830518, 6.092670068852159559, 352.3570229623690580 ) ) ;
#11429 = EDGE_CURVE ( 'NONE', #35816, #22547, #43380, .T. ) ;
#11430 = ORIENTED_EDGE ( 'NONE', *, *, #36217, .F. ) ;
#11431 = CARTESIAN_POINT ( 'NONE',  ( 797.6776695296629214, -307.5436935675104451, 357.6776695296636603 ) ) ;
#11432 = VECTOR ( 'NONE', #12992, 1000.000000000000000 ) ;
#11433 = EDGE_CURVE ( 'NONE', #23783, #22578, #7591, .T. ) ;
#11434 = CARTESIAN_POINT ( 'NONE',  ( 754.8983024940795303, -90.89650538077827946, -336.9254006560228163 ) ) ;
#11435 = CARTESIAN_POINT ( 'NONE',  ( 774.6858677611749044, -441.7255117493282910, 315.5713283507209894 ) ) ;
#11436 = CARTESIAN_POINT ( 'NONE',  ( 814.9108240113580450, -136.2709662947837330, -337.5031285880265273 ) ) ;
#11437 = ADVANCED_FACE ( 'NONE', ( #11518 ), #18230, .F. ) ;
#11438 = ORIENTED_EDGE ( 'NONE', *, *, #21258, .T. ) ;
#11439 = CARTESIAN_POINT ( 'NONE',  ( 788.8264449731201466, -141.1800572038746395, -363.6646147819170665 ) ) ;
#11440 = ORIENTED_EDGE ( 'NONE', *, *, #38278, .F. ) ;
#11441 = CARTESIAN_POINT ( 'NONE',  ( 804.6971507214547046, -411.2817908451521589, -344.0799538623459739 ) ) ;
#11442 = AXIS2_PLACEMENT_3D ( 'NONE', #26971, #36910, #41068 ) ;
#11443 = CARTESIAN_POINT ( 'NONE',  ( 796.9571628226829034, -455.4636090269701754, 321.2382568024804641 ) ) ;
#11444 = CARTESIAN_POINT ( 'NONE',  ( 763.2262854647970016, -224.6346026584198228, 309.2812353651462445 ) ) ;
#11445 = CARTESIAN_POINT ( 'NONE',  ( 798.7617431975189675, -147.6237781080508285, 323.0428371773161871 ) ) ;
#11448 = CARTESIAN_POINT ( 'NONE',  ( 814.8230680027162407, -389.8055962898682765, 333.7305795820267917 ) ) ;
#11447 = CARTESIAN_POINT ( 'NONE',  ( 949.5497976682736407, 239.9999999999998863, 339.9999999999998863 ) ) ;
#11446 = DIRECTION ( 'NONE',  ( -0.000000000000000000, 1.000000000000000000, -0.000000000000000000 ) ) ;
#11449 = AXIS2_PLACEMENT_3D ( 'NONE', #1730, #5899, #32552 ) ;
#11450 = AXIS2_PLACEMENT_3D ( 'NONE', #23179, #24036, #13897 ) ;
#11451 = ORIENTED_EDGE ( 'NONE', *, *, #27552, .F. ) ;
#11452 = CARTESIAN_POINT ( 'NONE',  ( 769.9779781133707957, -403.0999726633339719, -316.7813123517150871 ) ) ;
#11453 = CARTESIAN_POINT ( 'NONE',  ( 746.4999999999993179, -365.3551492539851893, -18.13243251470705886 ) ) ;
#11454 = CARTESIAN_POINT ( 'NONE',  ( 804.1009440267234822, -215.4636090269709712, -314.0944755984392600 ) ) ;
#11455 = CARTESIAN_POINT ( 'NONE',  ( 760.0363995740630116, -58.91815448151690759, 368.7758568127991907 ) ) ;
#11457 = CARTESIAN_POINT ( 'NONE',  ( 799.9999999999993179, 212.6707680665973612, 236.5295014342203785 ) ) ;
#11456 = FACE_OUTER_BOUND ( 'NONE', #16847, .T. ) ;
#11458 = EDGE_CURVE ( 'NONE', #31246, #35031, #18905, .T. ) ;
#11459 = CARTESIAN_POINT ( 'NONE',  ( 798.7617431975189675, -315.6237781080503169, -323.0428371773161871 ) ) ;
#11460 = DIRECTION ( 'NONE',  ( 0.000000000000000000, 0.000000000000000000, -1.000000000000000000 ) ) ;
#11461 = CARTESIAN_POINT ( 'NONE',  ( 814.8207195650702488, -194.1908817542437475, -336.2433038121456548 ) ) ;
#11462 = PLANE ( 'NONE',  #43670 ) ;
#11463 = FACE_BOUND ( 'NONE', #26064, .T. ) ;
#11464 = CARTESIAN_POINT ( 'NONE',  ( 769.0155153010367712, -394.3726999360613377, 362.7791456095907279 ) ) ;
#11465 = EDGE_CURVE ( 'NONE', #5169, #15565, #22629, .T. ) ;
#11466 = VECTOR ( 'NONE', #12373, 1000.000000000000000 ) ;
#11467 = CARTESIAN_POINT ( 'NONE',  ( 771.3260364891663130, -355.6454272087887603, 306.0683387631859773 ) ) ;
#11468 = VECTOR ( 'NONE', #11513, 1000.000000000000000 ) ;
#11469 = CARTESIAN_POINT ( 'NONE',  ( 745.4481719005789273, -243.7255117493288310, -347.5162901302853697 ) ) ;
#11470 = CYLINDRICAL_SURFACE ( 'NONE', #2475, 19.99999999999990763 ) ;
#11471 = CARTESIAN_POINT ( 'NONE',  ( 792.1044303154645831, -12.45278447660232146, -317.8323909638837677 ) ) ;
#11472 = CIRCLE ( 'NONE', #32828, 10.00000000000000888 ) ;
#11473 = CARTESIAN_POINT ( 'NONE',  ( 814.8207195650702488, -170.1908817542438328, 336.2433038121456548 ) ) ;
#11474 = CARTESIAN_POINT ( 'NONE',  ( 815.1787889125755555, -102.8965053807782368, -343.7953271457877804 ) ) ;
#11475 = CARTESIAN_POINT ( 'NONE',  ( 746.8695393053150156, -101.9073299311474727, 327.6429770376306010 ) ) ;
#11476 = CARTESIAN_POINT ( 'NONE',  ( 782.4968714119720516, -370.8164208402375834, -305.0891759886411023 ) ) ;
#11477 = EDGE_CURVE ( 'NONE', #33295, #44478, #39713, .T. ) ;
#11478 = DIRECTION ( 'NONE',  ( 0.000000000000000000, 0.000000000000000000, -1.000000000000000000 ) ) ;
#11479 = CARTESIAN_POINT ( 'NONE',  ( 799.9999999999993179, 197.3292319334027241, -273.4704985657796783 ) ) ;
#11480 = CARTESIAN_POINT ( 'NONE',  ( 803.4237431249931660, -231.1800572038743553, 331.2633955100225194 ) ) ;
#11481 = AXIS2_PLACEMENT_3D ( 'NONE', #15941, #44337, #12692 ) ;
#11482 = CARTESIAN_POINT ( 'NONE',  ( 810.4231160770870019, -456.5545181178792404, 321.9338519418446936 ) ) ;
#11483 = CARTESIAN_POINT ( 'NONE',  ( 766.5853460496234675, -421.9874144716863498, -372.3518521366060554 ) ) ;
#11484 = AXIS2_PLACEMENT_3D ( 'NONE', #45632, #38689, #31531 ) ;
#11485 = CARTESIAN_POINT ( 'NONE',  ( 762.1177392798416577, 5.445481882119263872, -309.8865473780659272 ) ) ;
#11486 = LINE ( 'NONE', #7339, #37978 ) ;
#11487 = CARTESIAN_POINT ( 'NONE',  ( 807.5423716828161105, -33.07832356259662987, 362.2119215644372048 ) ) ;
#11488 = ORIENTED_EDGE ( 'NONE', *, *, #6611, .F. ) ;
#11489 = CARTESIAN_POINT ( 'NONE',  ( 754.9735926884551418, -186.3510508353234343, -340.5236548041000333 ) ) ;
#11490 = CARTESIAN_POINT ( 'NONE',  ( 755.5713283507202505, -29.36187538569318178, 334.6858677611754729 ) ) ;
#11491 = CARTESIAN_POINT ( 'NONE',  ( 783.7566961878529810, -192.8965053807779668, -305.1792804349288417 ) ) ;
#11492 = CARTESIAN_POINT ( 'NONE',  ( -115.7583438952258774, 430.0000000000002842, -320.0000000000000568 ) ) ;
#11493 = CARTESIAN_POINT ( 'NONE',  ( 801.9858362298568863, -339.0783235625956422, 312.7379699480935642 ) ) ;
#11494 = CARTESIAN_POINT ( 'NONE',  ( 788.8264449731201466, -141.1800572038746395, 363.6646147819170665 ) ) ;
#11495 = EDGE_LOOP ( 'NONE', ( #26853, #37093 ) ) ;
#11496 = CARTESIAN_POINT ( 'NONE',  ( 755.0636971347428243, -148.2709662947837330, -341.7834795799807353 ) ) ;
#11497 = CARTESIAN_POINT ( 'NONE',  ( 768.0187753319979720, -344.6346026584195101, 318.0580252608186242 ) ) ;
#11498 = CARTESIAN_POINT ( 'NONE',  ( 782.4968714119720516, -34.81642084023861372, -305.0891759886411023 ) ) ;
#11499 = ORIENTED_EDGE ( 'NONE', *, *, #32094, .F. ) ;
#11500 = CARTESIAN_POINT ( 'NONE',  ( 814.4686193811664907, -435.2817908451521021, -346.2056067578752732 ) ) ;
#11501 = ORIENTED_EDGE ( 'NONE', *, *, #7185, .F. ) ;
#11502 = CARTESIAN_POINT ( 'NONE',  ( 804.4086373105744769, -337.6454272087888171, -333.3843516231986541 ) ) ;
#11504 = CARTESIAN_POINT ( 'NONE',  ( 773.4516893846965786, -355.6454272087887603, 315.8398074228977066 ) ) ;
#11503 = CARTESIAN_POINT ( 'NONE',  ( 797.8594530101008786, -61.54369356751124087, 322.1405469898980982 ) ) ;
#11505 = CARTESIAN_POINT ( 'NONE',  ( 804.4286716492782716, -281.3618753856923718, -345.3141322388244703 ) ) ;
#11506 = AXIS2_PLACEMENT_3D ( 'NONE', #3841, #8217, #28555 ) ;
#11508 = CARTESIAN_POINT ( 'NONE',  ( 754.0944755984390895, -303.6237781080503169, 364.1009440267246760 ) ) ;
#11507 = CARTESIAN_POINT ( 'NONE',  ( 804.7487373415286811, -403.5436935675101608, 364.7487373415288516 ) ) ;
#11509 = CARTESIAN_POINT ( 'NONE',  ( 786.5483106153019435, -295.6454272087888739, -364.1601925771022366 ) ) ;
#11510 = CARTESIAN_POINT ( 'NONE',  ( 792.1044303154645831, -276.4527844766013800, -317.8323909638837677 ) ) ;
#11511 = DIRECTION ( 'NONE',  ( -0.000000000000000000, -0.3826834323650836756, -0.9238795325112892920 ) ) ;
#11512 = CARTESIAN_POINT ( 'NONE',  ( 759.7806653035534055, -126.9982390220565094, -324.8639956371180801 ) ) ;
#11513 = DIRECTION ( 'NONE',  ( -1.000000000000000000, -0.000000000000000000, -0.000000000000000000 ) ) ;
#11514 = ORIENTED_EDGE ( 'NONE', *, *, #3815, .F. ) ;
#11515 = CARTESIAN_POINT ( 'NONE',  ( 745.4481719005789273, -435.7255117493282341, 347.5162901302853129 ) ) ;
#11516 = MECHANICAL_DESIGN_GEOMETRIC_PRESENTATION_REPRESENTATION (  '', ( #5588 ), #17411 ) ;
#11518 = FACE_OUTER_BOUND ( 'NONE', #30107, .T. ) ;
#11517 = DIRECTION ( 'NONE',  ( 0.000000000000000000, -0.6594541114781790059, 0.7517448203044204691 ) ) ;
#11519 = EDGE_CURVE ( 'NONE', #40621, #22833, #32207, .T. ) ;
#11520 = CARTESIAN_POINT ( 'NONE',  ( 788.6739635108323228, -79.64542720878957027, -373.9316612368139090 ) ) ;
#11521 = DIRECTION ( 'NONE',  ( -0.000000000000000000, 1.000000000000000000, -0.000000000000000000 ) ) ;
#11522 = LINE ( 'NONE', #36677, #29682 ) ;
#11523 = VECTOR ( 'NONE', #20908, 1000.000000000000000 ) ;
#11524 = CARTESIAN_POINT ( 'NONE',  ( 757.4527132478984868, -304.3726999360615082, 329.1273215169538844 ) ) ;
#11525 = CARTESIAN_POINT ( 'NONE',  ( 778.2165204200184689, -142.8164208402382656, 364.9363028652563230 ) ) ;
#11526 = VERTEX_POINT ( 'NONE', #42693 ) ;
#11527 = CARTESIAN_POINT ( 'NONE',  ( 772.5602148656447525, -105.7255117493293000, -305.7998596910095443 ) ) ;
#11528 = CARTESIAN_POINT ( 'NONE',  ( 756.1348686366196716, -329.2601417444138860, 347.5531968255698416 ) ) ;
#11529 = LINE ( 'NONE', #44690, #20457 ) ;
#11530 = CARTESIAN_POINT ( 'NONE',  ( 788.6739635108323228, -31.64542720878970883, 373.9316612368139090 ) ) ;
#11531 = CARTESIAN_POINT ( 'NONE',  ( 813.1304606946830518, -233.9073299311470180, -352.3570229623690580 ) ) ;
#11532 = ADVANCED_FACE ( 'NONE', ( #32999 ), #39927, .T. ) ;
#11533 = CARTESIAN_POINT ( 'NONE',  ( 796.9462024416508257, -204.4527844766016926, 308.9653473494370246 ) ) ;
#11534 = CARTESIAN_POINT ( 'NONE',  ( 781.8018195045266339, -118.2709662947837899, 365.1927285166406705 ) ) ;
#11535 = LINE ( 'NONE', #39033, #42442 ) ;
#11536 = CARTESIAN_POINT ( 'NONE',  ( 744.8212110874229666, -306.8965053807775689, -336.2046728542121627 ) ) ;
#11537 = VECTOR ( 'NONE', #4968, 999.9999999999998863 ) ;
#11538 = CARTESIAN_POINT ( 'NONE',  ( 776.9254006560222479, -20.19088175424429110, 314.8983024940802125 ) ) ;
#11539 = CARTESIAN_POINT ( 'NONE',  ( 751.9810565676468741, -314.0891481129650629, -360.9747183278973921 ) ) ;
#11540 = DIRECTION ( 'NONE',  ( 0.000000000000000000, 0.000000000000000000, 1.000000000000000000 ) ) ;
#11541 = CARTESIAN_POINT ( 'NONE',  ( 802.7791456095903868, -412.7146871989590409, 329.0155153010375102 ) ) ;
#11542 = VERTEX_POINT ( 'NONE', #11959 ) ;
#11543 = CARTESIAN_POINT ( 'NONE',  ( 805.1927285166397041, -424.8164208402372992, -341.8018195045277707 ) ) ;
#11544 = CARTESIAN_POINT ( 'NONE',  ( 781.7834795799800531, -226.8164208402380098, -315.0636971347436202 ) ) ;
#11545 = CARTESIAN_POINT ( 'NONE',  ( 773.7943932421234194, -95.80559628986917176, -305.5313806188329409 ) ) ;
#11546 = PLANE ( 'NONE',  #38780 ) ;
#11547 = CARTESIAN_POINT ( 'NONE',  ( 776.2433038121456548, -228.8965053807778816, 374.8207195650711014 ) ) ;
#11548 = CARTESIAN_POINT ( 'NONE',  ( 756.3353852180820240, -53.90732993114765037, 331.1735550268787733 ) ) ;
#11549 = CIRCLE ( 'NONE', #24782, 2.749999999999863665 ) ;
#11550 = EDGE_LOOP ( 'NONE', ( #28272, #17853, #45584, #72 ) ) ;
#11551 = CARTESIAN_POINT ( 'NONE',  ( 784.0799538623451781, -251.8055962898686744, -364.6971507214555572 ) ) ;
#11552 = CARTESIAN_POINT ( 'NONE',  ( 788.7366044899766848, -227.9073299311471033, 316.5762568750059813 ) ) ;
#11553 = AXIS2_PLACEMENT_3D ( 'NONE', #10641, #28187, #13262 ) ;
#11554 = CARTESIAN_POINT ( 'NONE',  ( 758.0141637701419768, -63.07832356259653750, -367.2620300519063790 ) ) ;
#11555 = LINE ( 'NONE', #4397, #17301 ) ;
#11556 = VERTEX_POINT ( 'NONE', #25358 ) ;
#11557 = CARTESIAN_POINT ( 'NONE',  ( 793.5525998758768083, -343.0999726633342561, -372.6845335610516941 ) ) ;
#11558 = CARTESIAN_POINT ( 'NONE',  ( 815.2698199232962679, -280.8164208402378108, 342.5225473063383674 ) ) ;
#11559 = CARTESIAN_POINT ( 'NONE',  ( 793.4146539503750546, -1.987414471687640294, 307.6481478633938877 ) ) ;
#11560 = CARTESIAN_POINT ( 'NONE',  ( 755.5913626894240451, -181.6454272087892434, -346.6156483768012890 ) ) ;
#11561 = CARTESIAN_POINT ( 'NONE',  ( 771.2633955100217236, -167.9073299311473022, -363.4237431249939618 ) ) ;
#11562 = CARTESIAN_POINT ( 'NONE',  ( 778.1981804954715471, -370.2709662947830793, -314.8072714833591021 ) ) ;
#11563 = ORIENTED_EDGE ( 'NONE', *, *, #12547, .F. ) ;
#11564 = CARTESIAN_POINT ( 'NONE',  ( 801.3366627262608972, 15.46713098285775878, -353.0897708529566899 ) ) ;
#11565 = ORIENTED_EDGE ( 'NONE', *, *, #2582, .F. ) ;
#11566 = CIRCLE ( 'NONE', #10807, 8.000000000000007105 ) ;
#11567 = CARTESIAN_POINT ( 'NONE',  ( 808.3070685750230950, -330.9982390220558273, 361.1904061080339261 ) ) ;
#11568 = DIRECTION ( 'NONE',  ( 0.000000000000000000, 0.000000000000000000, 1.000000000000000000 ) ) ;
#11569 = CARTESIAN_POINT ( 'NONE',  ( 776.9254006560222479, -212.1908817542436623, 314.8983024940802125 ) ) ;
#11570 = CIRCLE ( 'NONE', #43278, 9.999999999999980460 ) ;
#11571 = CARTESIAN_POINT ( 'NONE',  ( 911.9749999999993406, 154.9999999999998863, 360.0000000000000000 ) ) ;
#11572 = CARTESIAN_POINT ( 'NONE',  ( 796.1575198192839480, -150.0090635724257027, 359.4546378042384163 ) ) ;
#11573 = CARTESIAN_POINT ( 'NONE',  ( 755.5713283507202505, -53.36187538569310362, 334.6858677611754729 ) ) ;
#11574 = ORIENTED_EDGE ( 'NONE', *, *, #42141, .T. ) ;
#11575 = CARTESIAN_POINT ( 'NONE',  ( 750.9282345327678740, -400.9181544815159555, -319.8311093483690115 ) ) ;
#11576 = VECTOR ( 'NONE', #17763, 1000.000000000000000 ) ;
#11577 = CARTESIAN_POINT ( 'NONE',  ( 749.2812353651451076, -6.452784476602343666, -323.2262854647983090 ) ) ;
#11578 = CARTESIAN_POINT ( 'NONE',  ( 788.6739635108323228, -271.6454272087889876, 373.9316612368139090 ) ) ;
#11579 = CARTESIAN_POINT ( 'NONE',  ( 754.8983024940795303, -234.8965053807777963, 336.9254006560228163 ) ) ;
#11580 = VECTOR ( 'NONE', #16207, 1000.000000000000000 ) ;
#11581 = CARTESIAN_POINT ( 'NONE',  ( 778.2165204200184689, -358.8164208402375834, -364.9363028652563230 ) ) ;
#11582 = CARTESIAN_POINT ( 'NONE',  ( 788.7366044899766848, 12.09267006885214180, -316.5762568750059813 ) ) ;
#11583 = CARTESIAN_POINT ( 'NONE',  ( 756.3353852180819104, -5.907329931147798696, 331.1735550268788302 ) ) ;
#11584 = CARTESIAN_POINT ( 'NONE',  ( 998.9999999999992042, 74.99999999999984368, 359.0000000000000000 ) ) ;
#11585 = CARTESIAN_POINT ( 'NONE',  ( 766.9102291470427417, -258.5545181178799226, -318.6633372737382501 ) ) ;
#11586 = CIRCLE ( 'NONE', #44006, 6.118999999999985562 ) ;
#11587 = CARTESIAN_POINT ( 'NONE',  ( 813.1304606946830518, -41.90732993114767169, 352.3570229623690580 ) ) ;
#11588 = CARTESIAN_POINT ( 'NONE',  ( 777.5031285880264704, -118.8164208402383508, 374.9108240113588408 ) ) ;
#11589 = DIRECTION ( 'NONE',  ( 0.000000000000000000, 0.000000000000000000, -1.000000000000000000 ) ) ;
#11590 = DIRECTION ( 'NONE',  ( 0.000000000000000000, -0.000000000000000000, 1.000000000000000000 ) ) ;
#11591 = CARTESIAN_POINT ( 'NONE',  ( 815.3608509340175488, -386.7363362996977116, 341.2497674668889545 ) ) ;
#11592 = DIRECTION ( 'NONE',  ( 1.000000000000000000, -0.000000000000000000, -0.000000000000000000 ) ) ;
#11593 = CARTESIAN_POINT ( 'NONE',  ( 808.3070685750230950, -354.9982390220557704, 361.1904061080339261 ) ) ;
#11594 = CARTESIAN_POINT ( 'NONE',  ( 803.6646147819161570, -329.9073299311467053, -348.8264449731210561 ) ) ;
#11595 = CARTESIAN_POINT ( 'NONE',  ( 786.4999999999993179, -112.8054336623104348, 752.6593748957919843 ) ) ;
#11596 = CARTESIAN_POINT ( 'NONE',  ( 801.9419747391806368, -426.4527844766010389, 351.9812246680014027 ) ) ;
#11597 = CARTESIAN_POINT ( 'NONE',  ( 761.4292242960306112, -185.4636090269710280, 323.2154366446414429 ) ) ;
#11598 = CARTESIAN_POINT ( 'NONE',  ( 788.6739635108323228, -55.64542720878963422, -373.9316612368139090 ) ) ;
#11599 = CARTESIAN_POINT ( 'NONE',  ( 770.0799878456142551, -109.9874144716873019, -362.9823548866085616 ) ) ;
#11600 = CARTESIAN_POINT ( 'NONE',  ( 751.2241431872005251, -88.16923265350555994, 359.9636004259367610 ) ) ;
#11601 = CARTESIAN_POINT ( 'NONE',  ( 755.3201227861273992, -435.7255117493282341, 345.3687786644892981 ) ) ;
#11602 = CIRCLE ( 'NONE', #17504, 2.749999999999835687 ) ;
#11603 = CARTESIAN_POINT ( 'NONE',  ( 755.0636971347428243, -28.27096629478409540, -341.7834795799807353 ) ) ;
#11604 = CARTESIAN_POINT ( 'NONE',  ( 787.6308680596127942, -131.2601417444144829, -364.1105419155492768 ) ) ;
#11605 = CARTESIAN_POINT ( 'NONE',  ( 757.8323909638827445, -98.63460265842024910, -352.1044303154654358 ) ) ;
#11606 = VECTOR ( 'NONE', #19338, 1000.000000000000114 ) ;
#11607 = CARTESIAN_POINT ( 'NONE',  ( 759.2295555964440155, -424.1692326535044799, -353.9708237608231229 ) ) ;
#11609 = CARTESIAN_POINT ( 'NONE',  ( 797.8594530101009923, -277.5436935675105588, 322.1405469898982119 ) ) ;
#11608 = CARTESIAN_POINT ( 'NONE',  ( 765.0180583372156207, -264.9982390220561115, 360.0135310231089534 ) ) ;
#11610 = CARTESIAN_POINT ( 'NONE',  ( -208.8365100919714052, 256.5000000000001137, -199.9999999999926956 ) ) ;
#11611 = EDGE_LOOP ( 'NONE', ( #1157, #43247, #14322, #40627, #27114 ) ) ;
#11612 = CARTESIAN_POINT ( 'NONE',  ( 795.1360043628807261, -452.0891481129646650, 360.2193346964456282 ) ) ;
#11613 = CIRCLE ( 'NONE', #22667, 10.00000000000000888 ) ;
#11614 = EDGE_LOOP ( 'NONE', ( #37688, #10758 ) ) ;
#11615 = CIRCLE ( 'NONE', #41844, 7.999999999999896083 ) ;
#11616 = CARTESIAN_POINT ( 'NONE',  ( 810.7187646348534145, -186.4527844766017779, 356.7737145352016341 ) ) ;
#11617 = CARTESIAN_POINT ( 'NONE',  ( 793.9708237608222134, -262.9181544815162965, 319.2295555964448681 ) ) ;
#11618 = EDGE_LOOP ( 'NONE', ( #25727, #21084, #38889, #43403 ) ) ;
#11619 = CARTESIAN_POINT ( 'NONE',  ( 800.9840315886518738, -76.91815448151683654, -354.1144889064786412 ) ) ;
#11620 = CARTESIAN_POINT ( 'NONE',  ( 752.4576283171824116, -213.0783235625960401, 317.7880784355627952 ) ) ;
#11621 = CARTESIAN_POINT ( 'NONE',  ( 754.8072714833583632, -268.8164208402378677, -338.1981804954721156 ) ) ;
#11622 = ORIENTED_EDGE ( 'NONE', *, *, #10556, .F. ) ;
#11623 = CARTESIAN_POINT ( 'NONE',  ( 757.8323909638827445, -386.6346026584191691, -352.1044303154654358 ) ) ;
#11624 = CARTESIAN_POINT ( 'NONE',  ( 797.8594530101008786, -61.54369356751124087, -322.1405469898980982 ) ) ;
#11625 = CARTESIAN_POINT ( 'NONE',  ( 799.4546378042377910, -249.0783235625959549, 356.1575198192848006 ) ) ;
#11626 = CARTESIAN_POINT ( 'NONE',  ( 831.1634899080286232, 229.9999999999998863, -202.7499999999998295 ) ) ;
#11627 = DIRECTION ( 'NONE',  ( 1.000000000000000000, -5.551115123125783688E-16, 0.000000000000000000 ) ) ;
#11628 = CARTESIAN_POINT ( 'NONE',  ( 793.5525998758768083, -7.099972663335241130, -372.6845335610516941 ) ) ;
#11629 = CARTESIAN_POINT ( 'NONE',  ( 794.9999999999993179, -373.0259173205825505, 36.60293108048681887 ) ) ;
#11630 = EDGE_LOOP ( 'NONE', ( #305, #9936 ) ) ;
#11631 = CARTESIAN_POINT ( 'NONE',  ( 778.7629533639073998, -296.7363362996979390, -375.0009284576466371 ) ) ;
#11632 = EDGE_CURVE ( 'NONE', #19382, #37578, #26027, .T. ) ;
#11633 = CARTESIAN_POINT ( 'NONE',  ( 747.6481478633932056, -157.0999726633347962, 353.4146539503763620 ) ) ;
#11635 = CARTESIAN_POINT ( 'NONE',  ( 778.1981804954714335, -250.2709662947832783, -314.8072714833589885 ) ) ;
#11634 = CARTESIAN_POINT ( 'NONE',  ( 789.9999999999992042, 205.0000000000000568, -339.9999999999999432 ) ) ;
#11636 = CARTESIAN_POINT ( 'NONE',  ( 799.9999999999993179, -365.3551492539851893, 1.867567485292990437 ) ) ;
#11637 = CARTESIAN_POINT ( 'NONE',  ( 760.7433823573367135, -156.0090635724256742, -355.9930595647440441 ) ) ;
#11638 = VECTOR ( 'NONE', #377, 1000.000000000000000 ) ;
#11639 = CARTESIAN_POINT ( 'NONE',  ( 787.4397851343537695, -21.72551174932956641, 374.2001403089903988 ) ) ;
#11640 = CARTESIAN_POINT ( 'NONE',  ( 919.9999999999993179, 154.9999999999998863, -360.0000000000000000 ) ) ;
#11641 = CARTESIAN_POINT ( 'NONE',  ( 747.2067596250078623, -339.1800572038740142, -352.2312462859687230 ) ) ;
#11642 = LINE ( 'NONE', #8175, #8427 ) ;
#11643 = CARTESIAN_POINT ( 'NONE',  ( 756.5762568750052424, -27.18005720387500901, 348.7366044899774238 ) ) ;
#11644 = VECTOR ( 'NONE', #45117, 1000.000000000000000 ) ;
#11645 = CARTESIAN_POINT ( 'NONE',  ( 760.0363995740630116, -274.9181544815161828, 368.7758568127991907 ) ) ;
#11646 = CARTESIAN_POINT ( 'NONE',  ( 768.8385539511368734, -239.2601417444141987, -306.4236121716840557 ) ) ;
#11647 = CARTESIAN_POINT ( 'NONE',  ( 808.3070685750230950, -210.9982390220561967, 361.1904061080339261 ) ) ;
#11648 = CARTESIAN_POINT ( 'NONE',  ( 772.5602148656447525, 14.27448825067031812, -305.7998596910095443 ) ) ;
#11649 = CARTESIAN_POINT ( 'NONE',  ( 799.9999999999993179, -365.3551492539851893, 18.13243251470705886 ) ) ;
#11650 = EDGE_LOOP ( 'NONE', ( #28547, #3475 ) ) ;
#11651 = EDGE_CURVE ( 'NONE', #4463, #27157, #22571, .T. ) ;
#11652 = CARTESIAN_POINT ( 'NONE',  ( 771.2633955100217236, -335.9073299311468190, 363.4237431249939618 ) ) ;
#11653 = CARTESIAN_POINT ( 'NONE',  ( 790.9844846989617508, -70.37269993606230400, 317.2208543904092721 ) ) ;
#11654 = CARTESIAN_POINT ( 'NONE',  ( 783.0433043558608688, -24.89650538077847486, -315.1538015810313027 ) ) ;
#11655 = DIRECTION ( 'NONE',  ( 0.000000000000000000, 0.7372773368101421809, -0.6755902076156404812 ) ) ;
#11656 = DIRECTION ( 'NONE',  ( 0.000000000000000000, 0.000000000000000000, 1.000000000000000000 ) ) ;
#11658 = CARTESIAN_POINT ( 'NONE',  ( 754.8072714833581358, -364.8164208402374697, 338.1981804954720587 ) ) ;
#11657 = CARTESIAN_POINT ( 'NONE',  ( 763.2154366446407039, -165.6237781080507716, 321.4292242960311228 ) ) ;
#11659 = ORIENTED_EDGE ( 'NONE', *, *, #44442, .F. ) ;
#11660 = CARTESIAN_POINT ( 'NONE',  ( 766.7756240680305382, -302.5328690171411949, -361.5560724626415663 ) ) ;
#11661 = CARTESIAN_POINT ( 'NONE',  ( 794.9819416627830151, -156.9982390220564241, 319.9864689768909898 ) ) ;
#11662 = CARTESIAN_POINT ( 'NONE',  ( 800.1688906516307043, -322.1692326535048210, -369.0717654672308186 ) ) ;
#11663 = FACE_OUTER_BOUND ( 'NONE', #18420, .T. ) ;
#11664 = CARTESIAN_POINT ( 'NONE',  ( 758.8095938919642549, 15.91085188703394238, 311.6929314249763365 ) ) ;
#11665 = VERTEX_POINT ( 'NONE', #36674 ) ;
#11666 = CARTESIAN_POINT ( 'NONE',  ( 802.1676090361156639, -326.6346026584193396, 327.8955696845344505 ) ) ;
#11667 = CARTESIAN_POINT ( 'NONE',  ( 801.3366627262608972, -80.53286901714194812, -353.0897708529566899 ) ) ;
#11668 = ORIENTED_EDGE ( 'NONE', *, *, #23205, .F. ) ;
#11669 = CARTESIAN_POINT ( 'NONE',  ( 800.0135310231082713, -446.0891481129646081, 325.0180583372163028 ) ) ;
#11670 = ADVANCED_FACE ( 'NONE', ( #19125 ), #33213, .F. ) ;
#11671 = CARTESIAN_POINT ( 'NONE',  ( 755.2512626584698410, -199.5436935675108430, -315.2512626584710915 ) ) ;
#11672 = VERTEX_POINT ( 'NONE', #14762 ) ;
#11673 = CARTESIAN_POINT ( 'NONE',  ( 803.4237431249931660, -135.1800572038746679, -331.2633955100225194 ) ) ;
#11674 = ORIENTED_EDGE ( 'NONE', *, *, #22762, .F. ) ;
#11675 = VECTOR ( 'NONE', #20336, 1000.000000000000000 ) ;
#11676 = CARTESIAN_POINT ( 'NONE',  ( 759.0159684113467620, -424.9181544815158986, -325.8855110935213020 ) ) ;
#11677 = CARTESIAN_POINT ( 'NONE',  ( 762.1405469898971887, -1.543693567511449150, 357.8594530101015607 ) ) ;
#11678 = CARTESIAN_POINT ( 'NONE',  ( 812.7932403749906598, -231.1800572038743553, 327.7687537140311633 ) ) ;
#11679 = CARTESIAN_POINT ( 'NONE',  ( 761.2382568024794409, -159.6237781080508285, 356.9571628226838129 ) ) ;
#11682 = CARTESIAN_POINT ( 'NONE',  ( 815.1787889125755555, -414.8965053807771710, 343.7953271457877804 ) ) ;
#11681 = CARTESIAN_POINT ( 'NONE',  ( 786.4999999999993179, -512.9681489794448908, -329.9999999999999432 ) ) ;
#11680 = DIRECTION ( 'NONE',  ( 1.000000000000000000, 0.000000000000000000, -0.000000000000000000 ) ) ;
#11683 = EDGE_CURVE ( 'NONE', #24719, #16263, #35996, .T. ) ;
#11684 = ORIENTED_EDGE ( 'NONE', *, *, #18143, .T. ) ;
#11685 = EDGE_CURVE ( 'NONE', #23212, #32281, #41044, .T. ) ;
#11686 = CARTESIAN_POINT ( 'NONE',  ( 804.6971507214547046, -387.2817908451522726, -344.0799538623459739 ) ) ;
#11687 = DIRECTION ( 'NONE',  ( 1.000000000000000000, -0.000000000000000000, -0.000000000000000000 ) ) ;
#11688 = CARTESIAN_POINT ( 'NONE',  ( 815.3608509340175488, -194.7363362996982517, -341.2497674668889545 ) ) ;
#11689 = CARTESIAN_POINT ( 'NONE',  ( 762.1177392798416577, -66.55451811788050520, 309.8865473780659272 ) ) ;
#11691 = DIRECTION ( 'NONE',  ( -0.000000000000000000, -0.000000000000000000, 1.000000000000000000 ) ) ;
#11690 = DIRECTION ( 'NONE',  ( 0.000000000000000000, 0.000000000000000000, 1.000000000000000000 ) ) ;
#11692 = CARTESIAN_POINT ( 'NONE',  ( 773.3843516231979720, -325.4419599262320162, -364.4086373105754433 ) ) ;
#11693 = CARTESIAN_POINT ( 'NONE',  ( 831.1634899080286232, 259.9999999999998863, -197.2500000000000853 ) ) ;
#11694 = CARTESIAN_POINT ( 'NONE',  ( 776.2046728542105711, -188.1908817542437760, -304.8212110874238761 ) ) ;
#11695 = CARTESIAN_POINT ( 'NONE',  ( -746.4999999999993179, -365.3551492539851893, -8.132432514707076621 ) ) ;
#11696 = DIRECTION ( 'NONE',  ( 0.7014439490181308967, -0.1263042864341425708, 0.7014439490181749726 ) ) ;
#11697 = CARTESIAN_POINT ( 'NONE',  ( 763.0428371773158460, -395.4636090269705164, 358.7617431975195359 ) ) ;
#11698 = CARTESIAN_POINT ( 'NONE',  ( 772.5602148656447525, -225.7255117493289163, -305.7998596910095443 ) ) ;
#11699 = ADVANCED_FACE ( 'NONE', ( #1550, #16102 ), #2231, .F. ) ;
#11700 = CARTESIAN_POINT ( 'NONE',  ( 799.9999999999993179, 212.6707680665973612, 236.5295014342203785 ) ) ;
#11701 = CARTESIAN_POINT ( 'NONE',  ( 781.8018195045266339, 1.729033705215812011, -365.1927285166406705 ) ) ;
#11702 = CARTESIAN_POINT ( 'NONE',  ( 757.7880784355613741, -186.0090635724255890, 312.4576283171834916 ) ) ;
#11703 = EDGE_CURVE ( 'NONE', #17901, #23619, #37805, .T. ) ;
#11704 = CARTESIAN_POINT ( 'NONE',  ( 815.0009284576459549, -126.3510508353236048, -338.7629533639073429 ) ) ;
#11705 = CARTESIAN_POINT ( 'NONE',  ( 772.4837098697144029, -119.3618753856928691, 374.5518280994205611 ) ) ;
#11706 = CARTESIAN_POINT ( 'NONE',  ( 787.4397851343537695, -357.7255117493285184, -374.2001403089903988 ) ) ;
#11707 = CARTESIAN_POINT ( 'NONE',  ( -78.83651009197140525, 260.0000000000000568, -208.0249999999936108 ) ) ;
#11708 = LINE ( 'NONE', #624, #34579 ) ;
#11709 = CARTESIAN_POINT ( 'NONE',  ( 768.0187753319979720, -224.6346026584198228, 318.0580252608186242 ) ) ;
#11710 = CARTESIAN_POINT ( 'NONE',  ( 757.4527132478984868, -16.37269993606248519, 329.1273215169538844 ) ) ;
#11711 = CARTESIAN_POINT ( 'NONE',  ( 758.0141637701419768, -399.0783235625955285, -367.2620300519063790 ) ) ;
#11712 = CARTESIAN_POINT ( 'NONE',  ( 793.5525998758768083, -7.099972663335241130, -372.6845335610516941 ) ) ;
#11713 = DIRECTION ( 'NONE',  ( 1.000000000000000000, 0.000000000000000000, 0.000000000000000000 ) ) ;
#11714 = CARTESIAN_POINT ( 'NONE',  ( 764.3348316497523456, -22.71468719896029853, 308.6759233522265617 ) ) ;
#11715 = EDGE_LOOP ( 'NONE', ( #1556, #13243, #8639, #15571 ) ) ;
#11716 = CARTESIAN_POINT ( 'NONE',  ( 784.0799538623451781, -203.8055962898688449, -364.6971507214555572 ) ) ;
#11717 = CARTESIAN_POINT ( 'NONE',  ( 768.0187753319979720, -32.63460265842044095, 318.0580252608186242 ) ) ;
#11718 = CARTESIAN_POINT ( 'NONE',  ( 778.7502325331095108, -240.3510508353232069, -304.6391490659818828 ) ) ;
#11719 = SURFACE_STYLE_USAGE ( .BOTH. , #32504 ) ;
#11720 = CARTESIAN_POINT ( 'NONE',  ( 807.5423716828161105, -345.0783235625956991, 362.2119215644372048 ) ) ;
#11721 = CARTESIAN_POINT ( 'NONE',  ( 765.0180583372156207, -168.9982390220563673, 360.0135310231089534 ) ) ;
#11722 = ORIENTED_EDGE ( 'NONE', *, *, #34065, .F. ) ;
#11723 = CARTESIAN_POINT ( 'NONE',  ( 801.9858362298568863, -435.0783235625953580, 312.7379699480935642 ) ) ;
#11724 = EDGE_CURVE ( 'NONE', #25647, #30052, #30186, .T. ) ;
#11725 = CARTESIAN_POINT ( 'NONE',  ( 804.4286716492782716, -353.3618753856922012, 345.3141322388244703 ) ) ;
#11726 = EDGE_CURVE ( 'NONE', #43685, #21532, #44276, .T. ) ;
#11727 = CARTESIAN_POINT ( 'NONE',  ( 767.6429770376289525, -57.18005720387489532, -306.8695393053162093 ) ) ;
#11728 = EDGE_LOOP ( 'NONE', ( #37258, #29566, #5941, #33822 ) ) ;
#11729 = CARTESIAN_POINT ( 'NONE',  ( 807.2620300519052989, -456.0090635724247932, -318.0141637701419768 ) ) ;
#11730 = ORIENTED_EDGE ( 'NONE', *, *, #40850, .F. ) ;
#11731 = CARTESIAN_POINT ( 'NONE',  ( 755.1538015810308480, -326.1908817542433781, -343.0433043558613804 ) ) ;
#11733 = CARTESIAN_POINT ( 'NONE',  ( 757.0176451133909268, -373.0999726633340856, 349.9200121543848354 ) ) ;
#11732 = CARTESIAN_POINT ( 'NONE',  ( 767.8955696845333705, -72.45278447660213317, 362.1676090361162323 ) ) ;
#11734 = CARTESIAN_POINT ( 'NONE',  ( 774.6858677611749044, -297.7255117493286889, -315.5713283507209894 ) ) ;
#11735 = ADVANCED_FACE ( 'NONE', ( #5708 ), #19559, .F. ) ;
#11737 = CARTESIAN_POINT ( 'NONE',  ( 771.2368401574024119, -325.4419599262320162, 374.2805881961240857 ) ) ;
#11736 = CARTESIAN_POINT ( 'NONE',  ( 813.1304606946831655, -401.9073299311464211, 352.3570229623691716 ) ) ;
#11738 = EDGE_CURVE ( 'NONE', #40310, #29646, #2731, .T. ) ;
#11739 = CARTESIAN_POINT ( 'NONE',  ( 798.0661480581538854, -98.53286901714187707, 309.5768839229118043 ) ) ;
#11740 = CARTESIAN_POINT ( 'NONE',  ( 761.4292242960306112, -281.4636090269706870, -323.2154366446414429 ) ) ;
#11741 = CARTESIAN_POINT ( 'NONE',  ( 802.1676090361156639, -278.6346026584196807, -327.8955696845344505 ) ) ;
#11742 = FACE_OUTER_BOUND ( 'NONE', #22058, .T. ) ;
#11743 = CARTESIAN_POINT ( 'NONE',  ( 762.3223304703356007, -151.5436935675109851, -322.3223304703362828 ) ) ;
#11744 = LINE ( 'NONE', #36434, #40254 ) ;
#11745 = VECTOR ( 'NONE', #33495, 1000.000000000000000 ) ;
#11746 = CARTESIAN_POINT ( 'NONE',  ( 792.3570229623688874, -429.1800572038737869, 373.1304606946836202 ) ) ;
#11748 = DIRECTION ( 'NONE',  ( -1.000000000000000000, 0.000000000000000000, 0.000000000000000000 ) ) ;
#11747 = CARTESIAN_POINT ( 'NONE',  ( 774.2415430293718828, 19.23444159658009056, 310.5578503957772796 ) ) ;
#11749 = CARTESIAN_POINT ( 'NONE',  ( 809.0717654672305343, -100.9181544815167513, -360.1688906516309885 ) ) ;
#11750 = CARTESIAN_POINT ( 'NONE',  ( 879.9999999999992042, 469.9999999999998863, 360.0000000000000000 ) ) ;
#11751 = CARTESIAN_POINT ( 'NONE',  ( 911.9999999999992042, 154.9999999999998863, -359.9749999999999659 ) ) ;
#11752 = CARTESIAN_POINT ( 'NONE',  ( 776.9254006560222479, -308.1908817542434349, 314.8983024940802125 ) ) ;
#11753 = CARTESIAN_POINT ( 'NONE',  ( 759.9864689768902508, -146.0891481129655176, 354.9819416627836404 ) ) ;
#11754 = VERTEX_POINT ( 'NONE', #40595 ) ;
#11755 = CARTESIAN_POINT ( 'NONE',  ( 755.2512626584698410, -127.5436935675110561, -315.2512626584710915 ) ) ;
#11756 = CARTESIAN_POINT ( 'NONE',  ( 803.8651313633788504, -317.2601417444139429, 332.4468031744301015 ) ) ;
#11757 = DIRECTION ( 'NONE',  ( 0.000000000000000000, 0.000000000000000000, 1.000000000000000000 ) ) ;
#11758 = CARTESIAN_POINT ( 'NONE',  ( 800.7704444035546203, -436.1692326535044231, -326.0291762391768771 ) ) ;
#11759 = CARTESIAN_POINT ( 'NONE',  ( 797.8822607201568644, -78.55451811788046257, 370.1134526219340160 ) ) ;
#11760 = EDGE_CURVE ( 'NONE', #42322, #4785, #33420, .T. ) ;
#11761 = CARTESIAN_POINT ( 'NONE',  ( 814.5518280994195948, -255.7255117493287742, -332.4837098697145734 ) ) ;
#11762 = CARTESIAN_POINT ( 'NONE',  ( 777.4774526936600978, -202.2709662947834772, 304.7301800767027657 ) ) ;
#11763 = CARTESIAN_POINT ( 'NONE',  ( 759.9864689768902508, -98.08914811296568814, 354.9819416627836404 ) ) ;
#11764 = CARTESIAN_POINT ( 'NONE',  ( 764.3348316497523456, -310.7146871989593251, -308.6759233522265617 ) ) ;
#11765 = CARTESIAN_POINT ( 'NONE',  ( 802.9823548866075953, -1.099972663335260226, 330.0799878456151077 ) ) ;
#11766 = CARTESIAN_POINT ( 'NONE',  ( 801.1904061080336987, -356.0891481129647218, -368.3070685750235498 ) ) ;
#11767 = DIRECTION ( 'NONE',  ( -1.000000000000000000, -0.000000000000000000, 0.000000000000000000 ) ) ;
#11768 = CARTESIAN_POINT ( 'NONE',  ( 757.2208543904082489, -400.7146871989590977, 350.9844846989624330 ) ) ;
#11769 = ORIENTED_EDGE ( 'NONE', *, *, #18712, .T. ) ;
#11770 = CARTESIAN_POINT ( 'NONE',  ( 781.8018195045266339, -406.2709662947829088, -365.1927285166406705 ) ) ;
#11771 = CARTESIAN_POINT ( 'NONE',  ( 747.3154664389472828, -115.9874144716872877, -326.4474001241230781 ) ) ;
#11772 = CARTESIAN_POINT ( 'NONE',  ( 775.4999999999993179, -857.0166862835568509, -63.94525337997358605 ) ) ;
#11773 = CARTESIAN_POINT ( 'NONE',  ( 813.9316612368132837, -247.4419599262323004, 348.6739635108323228 ) ) ;
#11774 = CARTESIAN_POINT ( 'NONE',  ( 757.8323909638828582, -50.63460265842038410, 352.1044303154654358 ) ) ;
#11775 = AXIS2_PLACEMENT_3D ( 'NONE', #15213, #23167, #33817 ) ;
#11776 = EDGE_CURVE ( 'NONE', #34365, #14643, #44502, .T. ) ;
#11777 = CARTESIAN_POINT ( 'NONE',  ( 756.3353852180819104, -221.9073299311470464, 331.1735550268788302 ) ) ;
#11778 = EDGE_CURVE ( 'NONE', #16020, #37557, #2005, .T. ) ;
#11779 = CARTESIAN_POINT ( 'NONE',  ( 805.9055244015594326, -51.62377810805111267, -315.8990559732753240 ) ) ;
#11780 = CARTESIAN_POINT ( 'NONE',  ( 791.3800697268461590, -452.9681489794449476, -362.3092612109132915 ) ) ;
#11781 = ORIENTED_EDGE ( 'NONE', *, *, #2395, .T. ) ;
#11782 = EDGE_LOOP ( 'NONE', ( #12503, #43387, #23339, #34195 ) ) ;
#11783 = CARTESIAN_POINT ( 'NONE',  ( 764.1737431748507561, -346.3726999360614514, -371.6461892240376415 ) ) ;
#11784 = CARTESIAN_POINT ( 'NONE',  ( 796.9462024416508257, -300.4527844766013231, 308.9653473494370246 ) ) ;
#11785 = CARTESIAN_POINT ( 'NONE',  ( 756.1443688327750579, -21.62377810805121570, 314.3581564841659315 ) ) ;
#11786 = CARTESIAN_POINT ( 'NONE',  ( 802.5472867521000353, -172.3726999360619914, -350.8726784830461156 ) ) ;
#11787 = CARTESIAN_POINT ( 'NONE',  ( 778.2165204200184689, -190.8164208402381234, -364.9363028652563230 ) ) ;
#11788 = CARTESIAN_POINT ( 'NONE',  ( 755.0636971347428243, -388.2709662947829656, -341.7834795799807353 ) ) ;
#11789 = VERTEX_POINT ( 'NONE', #43806 ) ;
#11790 = CARTESIAN_POINT ( 'NONE',  ( 797.6776695296629214, -451.5436935675099903, -357.6776695296636603 ) ) ;
#11791 = VERTEX_POINT ( 'NONE', #2460 ) ;
#11792 = CARTESIAN_POINT ( 'NONE',  ( 792.2312462859673587, -323.9073299311468190, 307.2067596250082602 ) ) ;
#11793 = FACE_OUTER_BOUND ( 'NONE', #4727, .T. ) ;
#11794 = CARTESIAN_POINT ( 'NONE',  ( 754.8983024940795303, -354.8965053807774552, 336.9254006560228163 ) ) ;
#11795 = DIRECTION ( 'NONE',  ( -0.000000000000000000, -0.000000000000000000, 1.000000000000000000 ) ) ;
#11796 = CARTESIAN_POINT ( 'NONE',  ( 786.5483106153019435, -199.6454272087891582, 364.1601925771022366 ) ) ;
#11797 = CARTESIAN_POINT ( 'NONE',  ( 764.8639956371174549, -32.08914811296588709, 319.7806653035542013 ) ) ;
#11798 = ORIENTED_EDGE ( 'NONE', *, *, #36558, .F. ) ;
#11799 = CARTESIAN_POINT ( 'NONE',  ( 746.4236121716829757, -423.8272453906067199, -328.8385539511384650 ) ) ;
#11800 = CARTESIAN_POINT ( 'NONE',  ( 777.4774526936600978, -34.27096629478407408, -304.7301800767028226 ) ) ;
#11801 = CARTESIAN_POINT ( 'NONE',  ( 803.8651313633788504, -221.2601417444142271, 332.4468031744301015 ) ) ;
#11802 = CARTESIAN_POINT ( 'NONE',  ( 757.8323909638827445, -386.6346026584191691, -352.1044303154654358 ) ) ;
#11803 = CARTESIAN_POINT ( 'NONE',  ( 805.1927285166399315, 7.183579159761249500, -341.8018195045277707 ) ) ;
#11804 = CARTESIAN_POINT ( 'NONE',  ( 811.0346526505616112, -446.6346026584189985, 323.0537975583477532 ) ) ;
#11805 = CARTESIAN_POINT ( 'NONE',  ( -208.8365100919714052, 258.0940000000001078, -199.9999999999926956 ) ) ;
#11806 = CARTESIAN_POINT ( 'NONE',  ( 759.0159684113467620, -256.9181544815163534, -325.8855110935213020 ) ) ;
#11807 = CARTESIAN_POINT ( 'NONE',  ( 787.5162901302840055, -179.3618753856927128, -305.4481719005792684 ) ) ;
#11808 = CARTESIAN_POINT ( 'NONE',  ( 782.4968714119720516, -58.81642084023854267, 305.0891759886411023 ) ) ;
#11809 = CARTESIAN_POINT ( 'NONE',  ( 815.2698199232961542, -112.8164208402383508, 342.5225473063383106 ) ) ;
#11810 = PLANE ( 'NONE',  #17360 ) ;
#11811 = DIRECTION ( 'NONE',  ( 0.000000000000000000, 0.000000000000000000, 1.000000000000000000 ) ) ;
#11812 = CARTESIAN_POINT ( 'NONE',  ( 755.8990559732751535, -395.4636090269705164, 365.9055244015606831 ) ) ;
#11813 = DIRECTION ( 'NONE',  ( -1.000000000000000000, -4.625929269271485914E-16, 0.000000000000000000 ) ) ;
#11814 = CARTESIAN_POINT ( 'NONE',  ( 813.1304606946830518, -377.9073299311466485, 352.3570229623690580 ) ) ;
#11815 = CARTESIAN_POINT ( 'NONE',  ( 756.3353852180819104, -317.9073299311468190, -331.1735550268788302 ) ) ;
#11816 = CARTESIAN_POINT ( 'NONE',  ( 795.1360043628807261, -452.0891481129646650, 360.2193346964456282 ) ) ;
#11817 = CARTESIAN_POINT ( 'NONE',  ( 804.4086373105744769, -193.6454272087891582, 333.3843516231986541 ) ) ;
#11818 = CARTESIAN_POINT ( 'NONE',  ( 805.6418435158337843, -53.46360902697146855, -363.8556311672236916 ) ) ;
#11819 = CARTESIAN_POINT ( 'NONE',  ( 772.3691319403857278, -119.2601417444145397, -315.8894580844506663 ) ) ;
#11820 = CARTESIAN_POINT ( 'NONE',  ( 815.1787889125755555, -126.8965053807781516, 343.7953271457877804 ) ) ;
#11821 = CARTESIAN_POINT ( 'NONE',  ( 805.1927285166399315, -448.8164208402372424, 341.8018195045277707 ) ) ;
#11822 = CARTESIAN_POINT ( 'NONE',  ( 754.8072714833581358, -28.81642084023863148, -338.1981804954720587 ) ) ;
#11823 = CARTESIAN_POINT ( 'NONE',  ( 759.2295555964440155, -136.1692326535053894, -353.9708237608231229 ) ) ;
#11824 = CARTESIAN_POINT ( 'NONE',  ( 785.3141322388236176, -141.7255117493291721, -364.4286716492789537 ) ) ;
#11825 = CARTESIAN_POINT ( 'NONE',  ( 778.7502325331095108, 23.64894916467591912, -304.6391490659818828 ) ) ;
#11827 = CARTESIAN_POINT ( 'NONE',  ( 756.3353852180820240, -245.9073299311469896, 331.1735550268787733 ) ) ;
#11826 = CARTESIAN_POINT ( 'NONE',  ( 778.2165204200184689, -262.8164208402379245, 364.9363028652563230 ) ) ;
#11828 = CARTESIAN_POINT ( 'NONE',  ( 759.9999999999992042, 205.0000000000000568, 339.9999999999999432 ) ) ;
#11829 = VERTEX_POINT ( 'NONE', #12190 ) ;
#11830 = CARTESIAN_POINT ( 'NONE',  ( 757.2208543904082489, 7.285312801039605546, 350.9844846989624330 ) ) ;
#11831 = ORIENTED_EDGE ( 'NONE', *, *, #4114, .T. ) ;
#11832 =( LENGTH_UNIT ( ) NAMED_UNIT ( * ) SI_UNIT ( .MILLI., .METRE. ) );
#11833 = CARTESIAN_POINT ( 'NONE',  ( 749.2812353651451076, -174.4527844766018063, 323.2262854647983090 ) ) ;
#11834 = CARTESIAN_POINT ( 'NONE',  ( 754.7162404726377645, -278.7363362996980527, 339.4709603349214717 ) ) ;
#11835 = CARTESIAN_POINT ( 'NONE',  ( 805.1016975059191054, -390.8965053807772279, 343.0745993439771837 ) ) ;
#11836 = EDGE_LOOP ( 'NONE', ( #34716, #2943 ) ) ;
#11837 = CARTESIAN_POINT ( 'NONE',  ( 787.5531968255692163, -93.82724539060770041, -316.1348686366205811 ) ) ;
#11838 = CARTESIAN_POINT ( 'NONE',  ( 810.1134526219336749, -224.5328690171415076, 357.8822607201570349 ) ) ;
#11839 = CARTESIAN_POINT ( 'NONE',  ( 759.9864689768902508, -266.0891481129651197, -354.9819416627836404 ) ) ;
#11840 = VERTEX_POINT ( 'NONE', #26945 ) ;
#11841 = CARTESIAN_POINT ( 'NONE',  ( 771.1735550268778070, -393.1800572038737300, -316.3353852180827630 ) ) ;
#11842 = CARTESIAN_POINT ( 'NONE',  ( 800.2193346964447755, -42.99823902205675807, -355.1360043628815788 ) ) ;
#11843 = CARTESIAN_POINT ( 'NONE',  ( 804.9511171171677688, -269.8055962898686175, 335.8780910478229202 ) ) ;
#11844 = LINE ( 'NONE', #26145, #28506 ) ;
#11845 = CARTESIAN_POINT ( 'NONE',  ( -879.9999999999992042, 240.0000000000002274, -244.9999999999999716 ) ) ;
#11846 = CARTESIAN_POINT ( 'NONE',  ( 805.6418435158337843, -29.46360902697153250, -363.8556311672236916 ) ) ;
#11847 = CARTESIAN_POINT ( 'NONE',  ( -773.4999999999993179, -512.9681489794448908, -329.9999999999999432 ) ) ;
#11848 = ORIENTED_EDGE ( 'NONE', *, *, #4927, .F. ) ;
#11849 = CARTESIAN_POINT ( 'NONE',  ( 778.7629533639073998, -320.7363362996979390, -375.0009284576466371 ) ) ;
#11850 = CARTESIAN_POINT ( 'NONE',  ( 773.7305795820266212, -177.2817908451528695, 374.8230680027170365 ) ) ;
#11852 = CARTESIAN_POINT ( 'NONE',  ( 791.9812246680005501, -284.6346026584196807, -361.9419747391813189 ) ) ;
#11851 = DIRECTION ( 'NONE',  ( 0.000000000000000000, 0.000000000000000000, 1.000000000000000000 ) ) ;
#11853 = PLANE ( 'NONE',  #17166 ) ;
#11854 = CARTESIAN_POINT ( 'NONE',  ( 779.4763451958990572, -152.7363362996983938, -365.0264073115438919 ) ) ;
#11855 = CARTESIAN_POINT ( 'NONE',  ( 805.0032342141412300, -13.54369356751140785, 314.9967657858571783 ) ) ;
#11856 = CARTESIAN_POINT ( 'NONE',  ( 879.9999999999990905, 479.9999999999998863, -360.0000000000000000 ) ) ;
#11857 = CARTESIAN_POINT ( 'NONE',  ( 754.9967657858570647, -337.5436935675102745, -365.0032342141425943 ) ) ;
#11858 = CARTESIAN_POINT ( 'NONE',  ( 793.3938497862117174, -453.0432664090020580, -372.3358127763068524 ) ) ;
#11859 = CARTESIAN_POINT ( 'NONE',  ( 804.4286716492782716, -41.36187538569314626, 345.3141322388244703 ) ) ;
#11860 = CARTESIAN_POINT ( 'NONE',  ( 814.2805881961230625, -289.6454272087889308, 331.2368401574024119 ) ) ;
#11861 = CARTESIAN_POINT ( 'NONE',  ( 793.4146539503750546, -241.9874144716869182, -307.6481478633938877 ) ) ;
#11862 = CARTESIAN_POINT ( 'NONE',  ( 787.5162901302840055, -251.3618753856923149, 305.4481719005792684 ) ) ;
#11863 = CARTESIAN_POINT ( 'NONE',  ( 800.9747183278959710, 11.00176097794305541, -311.9810565676471583 ) ) ;
#11864 = DIRECTION ( 'NONE',  ( 0.000000000000000000, 0.000000000000000000, -1.000000000000000000 ) ) ;
#11865 = VERTEX_POINT ( 'NONE', #23471 ) ;
#11866 = CARTESIAN_POINT ( 'NONE',  ( 756.5762568750052424, -339.1800572038740142, 348.7366044899774238 ) ) ;
#11867 = CARTESIAN_POINT ( 'NONE',  ( 787.5531968255692163, -93.82724539060770041, 316.1348686366205811 ) ) ;
#11868 = CARTESIAN_POINT ( 'NONE',  ( 772.3691319403857278, 0.7398582555850804487, -315.8894580844506663 ) ) ;
#11869 = DIRECTION ( 'NONE',  ( 1.000000000000000000, 0.000000000000000000, 0.000000000000000000 ) ) ;
#11870 = LINE ( 'NONE', #16235, #30658 ) ;
#11871 = CARTESIAN_POINT ( 'NONE',  ( 786.2056067578752163, -131.8055962898690439, 374.4686193811670023 ) ) ;
#11872 = CARTESIAN_POINT ( 'NONE',  ( 771.2633955100217236, -407.9073299311465348, 363.4237431249939618 ) ) ;
#11873 = ORIENTED_EDGE ( 'NONE', *, *, #43315, .T. ) ;
#11874 = CARTESIAN_POINT ( 'NONE',  ( 803.2186876482843445, -343.9874144716865771, -350.0220218866286928 ) ) ;
#11875 = CARTESIAN_POINT ( 'NONE',  ( 765.0180583372156207, -144.9982390220564525, 360.0135310231089534 ) ) ;
#11876 = EDGE_CURVE ( 'NONE', #19577, #3612, #8734, .T. ) ;
#11877 = CARTESIAN_POINT ( 'NONE',  ( 813.2346286133761168, -317.2601417444139429, -328.9521613784389160 ) ) ;
#11878 = CARTESIAN_POINT ( 'NONE',  ( 571.1634899080285095, 258.0939999999999372, -206.1189999999981239 ) ) ;
#11879 = CARTESIAN_POINT ( 'NONE',  ( 814.2001403089898304, 6.638124614306706306, 347.4397851343538264 ) ) ;
#11880 = ORIENTED_EDGE ( 'NONE', *, *, #29475, .T. ) ;
#11881 = CARTESIAN_POINT ( 'NONE',  ( 764.8639956371174549, -368.0891481129647786, 319.7806653035542013 ) ) ;
#11882 = CARTESIAN_POINT ( 'NONE',  ( 804.1601925771018387, -79.44195992623286884, -346.5483106153029098 ) ) ;
#11883 = ORIENTED_EDGE ( 'NONE', *, *, #35064, .T. ) ;
#11884 = DIRECTION ( 'NONE',  ( -1.880165489482579047E-16, -1.000000000000000000, -0.000000000000000000 ) ) ;
#11885 = CARTESIAN_POINT ( 'NONE',  ( 763.0537975583475827, -168.4527844766018347, -371.0346526505627480 ) ) ;
#11886 = ORIENTED_EDGE ( 'NONE', *, *, #2160, .F. ) ;
#11887 = CARTESIAN_POINT ( 'NONE',  ( 805.1927285166399315, -160.8164208402382371, -341.8018195045277707 ) ) ;
#11888 = ORIENTED_EDGE ( 'NONE', *, *, #4624, .T. ) ;
#11889 = CARTESIAN_POINT ( 'NONE',  ( 793.0897708529556667, -438.5545181178793541, -361.3366627262616362 ) ) ;
#11890 = CARTESIAN_POINT ( 'NONE',  ( 800.0135310231082713, 9.910851887033969021, 325.0180583372163028 ) ) ;
#11891 = CARTESIAN_POINT ( 'NONE',  ( 764.0069404352550464, -159.0783235625962391, 359.2566176426627180 ) ) ;
#11893 = DIRECTION ( 'NONE',  ( 0.000000000000000000, -1.000000000000000000, 0.000000000000000000 ) ) ;
#11892 = CARTESIAN_POINT ( 'NONE',  ( 772.4999999999993179, -462.9681489794447202, -270.0000000000000568 ) ) ;
#11894 = ORIENTED_EDGE ( 'NONE', *, *, #18732, .F. ) ;
#11895 = EDGE_CURVE ( 'NONE', #38954, #14962, #23012, .T. ) ;
#11896 = CARTESIAN_POINT ( 'NONE',  ( 759.0159684113467620, -424.9181544815158986, -325.8855110935213020 ) ) ;
#11897 = LINE ( 'NONE', #25071, #21851 ) ;
#11898 = CARTESIAN_POINT ( 'NONE',  ( 788.6739635108323228, -199.6454272087891582, -373.9316612368139090 ) ) ;
#11899 = CIRCLE ( 'NONE', #31801, 2.749999999999863665 ) ;
#11900 = CARTESIAN_POINT ( 'NONE',  ( 805.6418435158337843, -77.46360902697138329, 363.8556311672236916 ) ) ;
#11902 = CARTESIAN_POINT ( 'NONE',  ( 779.9999999999992042, -462.9681489794448339, 339.9999999999999432 ) ) ;
#11901 = CARTESIAN_POINT ( 'NONE',  ( 794.9999999999993179, 205.0000000000000568, -265.0000000000000000 ) ) ;
#11903 = CARTESIAN_POINT ( 'NONE',  ( 772.3691319403857278, -335.2601417444137724, -315.8894580844506663 ) ) ;
#11904 = DIRECTION ( 'NONE',  ( 0.000000000000000000, -1.000000000000000000, 0.000000000000000000 ) ) ;
#11905 = CARTESIAN_POINT ( 'NONE',  ( 805.6418435158337843, -221.4636090269709428, -363.8556311672236916 ) ) ;
#11906 = CYLINDRICAL_SURFACE ( 'NONE', #12706, 50.00000000000004263 ) ;
#11907 = FACE_BOUND ( 'NONE', #15318, .T. ) ;
#11908 = CARTESIAN_POINT ( 'NONE',  ( 755.8894580844503253, -399.8272453906067767, 332.3691319403863531 ) ) ;
#11909 = CARTESIAN_POINT ( 'NONE',  ( 772.4837098697145166, -239.3618753856924855, -374.5518280994205611 ) ) ;
#11910 = CARTESIAN_POINT ( 'NONE',  ( 799.2566176426618085, -240.0090635724253900, 324.0069404352559559 ) ) ;
#11911 = LINE ( 'NONE', #19509, #17996 ) ;
#11912 = CARTESIAN_POINT ( 'NONE',  ( 759.9864689768902508, -26.08914811296592262, -354.9819416627836404 ) ) ;
#11913 = CARTESIAN_POINT ( 'NONE',  ( 776.2046728542105711, -188.1908817542437760, 304.8212110874238761 ) ) ;
#11914 = CARTESIAN_POINT ( 'NONE',  ( 791.1614460488616487, -131.2601417444144829, -373.5763878283158874 ) ) ;
#11915 = CARTESIAN_POINT ( 'NONE',  ( 745.0891759886404770, -148.2709662947837330, 342.4968714119734159 ) ) ;
#11916 = CARTESIAN_POINT ( 'NONE',  ( 801.1904061080336987, -380.0891481129646650, -368.3070685750235498 ) ) ;
#11917 = CARTESIAN_POINT ( 'NONE',  ( 911.9999999999994316, 219.9999999999998863, 360.0000000000000000 ) ) ;
#11918 = CARTESIAN_POINT ( 'NONE',  ( -468.8365100919714337, 260.0000000000001705, -208.0249999999908823 ) ) ;
#11919 = CARTESIAN_POINT ( 'NONE',  ( 797.8594530101008786, -229.5436935675106440, 322.1405469898980982 ) ) ;
#11920 = CARTESIAN_POINT ( 'NONE',  ( 757.4527132478984868, -40.37269993606240348, 329.1273215169538844 ) ) ;
#11921 = CARTESIAN_POINT ( 'NONE',  ( 781.8018195045266339, -382.2709662947828519, -365.1927285166406705 ) ) ;
#11922 = CARTESIAN_POINT ( 'NONE',  ( 807.2620300519052989, -0.009063572426172561425, -318.0141637701419768 ) ) ;
#11923 = LINE ( 'NONE', #15614, #2588 ) ;
#11924 = CARTESIAN_POINT ( 'NONE',  ( 744.9990715423526808, -18.35105083532395298, 341.2370466360926002 ) ) ;
#11925 = ORIENTED_EDGE ( 'NONE', *, *, #41944, .F. ) ;
#11926 = EDGE_CURVE ( 'NONE', #40161, #44892, #22800, .T. ) ;
#11927 = APPLICATION_CONTEXT ( 'automotive_design' ) ;
#11928 = CARTESIAN_POINT ( 'NONE',  ( 772.3691319403857278, -239.2601417444141987, -315.8894580844506663 ) ) ;
#11929 = CARTESIAN_POINT ( 'NONE',  ( 778.2165204200184689, -22.81642084023865280, 364.9363028652563230 ) ) ;
#11930 = CIRCLE ( 'NONE', #28149, 10.00000000000000888 ) ;
#11931 = EDGE_CURVE ( 'NONE', #11672, #8476, #30408, .T. ) ;
#11932 = CARTESIAN_POINT ( 'NONE',  ( 748.3538107759620743, -208.7146871989596946, -355.8262568251490165 ) ) ;
#11933 = CARTESIAN_POINT ( 'NONE',  ( -208.8365100919714052, 240.0000000000000853, -197.2499999999928377 ) ) ;
#11934 = CARTESIAN_POINT ( 'NONE',  ( 812.6845335610512393, -343.9874144716865771, 353.5525998758768651 ) ) ;
#11935 = ORIENTED_EDGE ( 'NONE', *, *, #26956, .F. ) ;
#11936 = CARTESIAN_POINT ( 'NONE',  ( 781.2497674668890113, -420.3510508353225532, 375.3608509340180603 ) ) ;
#11937 = CARTESIAN_POINT ( 'NONE',  ( 802.1676090361156639, -134.6346026584201070, -327.8955696845344505 ) ) ;
#11938 = CARTESIAN_POINT ( 'NONE',  ( 795.1360043628807261, -356.0891481129647218, 360.2193346964456282 ) ) ;
#11939 = CARTESIAN_POINT ( 'NONE',  ( 801.1904061080336987, -68.08914811296575920, -368.3070685750235498 ) ) ;
#11940 = CARTESIAN_POINT ( 'NONE',  ( 788.8264449731201466, -69.18005720387488111, -363.6646147819170665 ) ) ;
#11941 = ORIENTED_EDGE ( 'NONE', *, *, #15989, .T. ) ;
#11942 = CARTESIAN_POINT ( 'NONE',  ( 776.9254006560222479, 3.809118245755632959, -314.8983024940802125 ) ) ;
#11943 = ORIENTED_EDGE ( 'NONE', *, *, #6905, .T. ) ;
#11944 = CARTESIAN_POINT ( 'NONE',  ( 761.4292242960306112, -305.4636090269706870, -323.2154366446414429 ) ) ;
#11945 = CONTEXT_DEPENDENT_SHAPE_REPRESENTATION ( #44088, #13341 ) ;
#11947 = CARTESIAN_POINT ( 'NONE',  ( 773.4516893846965786, -379.6454272087886466, 315.8398074228977066 ) ) ;
#11946 = CARTESIAN_POINT ( 'NONE',  ( 788.8264449731200330, -45.18005720387493085, 363.6646147819171233 ) ) ;
#11948 = CARTESIAN_POINT ( 'NONE',  ( 755.3201227861273992, -315.7255117493286320, -345.3687786644892981 ) ) ;
#11950 = CARTESIAN_POINT ( 'NONE',  ( 811.6461892240364477, -316.7146871989593819, 324.1737431748509835 ) ) ;
#11949 = CARTESIAN_POINT ( 'NONE',  ( 754.9967657858570647, -433.5436935675100472, 365.0032342141425943 ) ) ;
#11951 = CARTESIAN_POINT ( 'NONE',  ( 810.1134526219336749, -104.5328690171418913, 357.8822607201570349 ) ) ;
#11952 = CARTESIAN_POINT ( 'NONE',  ( 763.8424801807145741, -330.0090635724251342, -320.5453621957614700 ) ) ;
#11953 = CARTESIAN_POINT ( 'NONE',  ( 791.9812246680005501, -284.6346026584196807, -361.9419747391813189 ) ) ;
#11954 = DIRECTION ( 'NONE',  ( 0.000000000000000000, 0.000000000000000000, 1.000000000000000000 ) ) ;
#11955 = CARTESIAN_POINT ( 'NONE',  ( 755.3201227861273992, -147.7255117493291152, -345.3687786644892981 ) ) ;
#11956 = CARTESIAN_POINT ( 'NONE',  ( 441.1634899080286232, 256.4999999999999432, -193.8809999999972433 ) ) ;
#11957 = CARTESIAN_POINT ( 'NONE',  ( 810.7187646348534145, -426.4527844766010389, 356.7737145352016341 ) ) ;
#11959 = CARTESIAN_POINT ( 'NONE',  ( 989.9999999999992042, -590.0000000000001137, -350.0000000000000000 ) ) ;
#11958 = CARTESIAN_POINT ( 'NONE',  ( -773.4999999999993179, -544.8427095258973623, -350.0000000000000000 ) ) ;
#11960 = CARTESIAN_POINT ( 'NONE',  ( 797.8822607201568644, -78.55451811788046257, -370.1134526219340160 ) ) ;
#11961 = CARTESIAN_POINT ( 'NONE',  ( -959.5497976682736407, 240.0000000000002274, -209.9999999999999716 ) ) ;
#11962 = CARTESIAN_POINT ( 'NONE',  ( -208.8365100919714052, 260.0000000000001137, -197.2499999999928377 ) ) ;
#11963 = CARTESIAN_POINT ( 'NONE',  ( 786.5483106153019435, -295.6454272087888739, 364.1601925771022366 ) ) ;
#11964 = CARTESIAN_POINT ( 'NONE',  ( 804.4286716492782716, -137.3618753856928265, 345.3141322388244703 ) ) ;
#11965 = EDGE_LOOP ( 'NONE', ( #5860, #24534, #32964, #33852 ) ) ;
#11966 = VECTOR ( 'NONE', #12368, 1000.000000000000114 ) ;
#11967 = CARTESIAN_POINT ( 'NONE',  ( 745.4481719005789273, -123.7255117493292289, -347.5162901302853697 ) ) ;
#11968 = CARTESIAN_POINT ( 'NONE',  ( 805.1016975059191054, -318.8965053807775121, 343.0745993439771837 ) ) ;
#11969 = LINE ( 'NONE', #1114, #32270 ) ;
#11970 = CARTESIAN_POINT ( 'NONE',  ( 781.2370466360911223, -68.73633629969867798, 304.9990715423533629 ) ) ;
#11971 = CARTESIAN_POINT ( 'NONE',  ( 758.8095938919642549, -272.0891481129651197, -311.6929314249763365 ) ) ;
#11972 = EDGE_CURVE ( 'NONE', #32155, #8476, #15873, .T. ) ;
#11973 = CARTESIAN_POINT ( 'NONE',  ( 814.2001403089898304, -209.3618753856926276, 347.4397851343538264 ) ) ;
#11974 = CARTESIAN_POINT ( 'NONE',  ( 804.6798772138708955, -111.7255117493293000, 334.6312213355107019 ) ) ;
#11975 = ORIENTED_EDGE ( 'NONE', *, *, #5499, .F. ) ;
#11976 = CARTESIAN_POINT ( 'NONE',  ( 764.3348316497523456, -358.7146871989592114, -308.6759233522265617 ) ) ;
#11977 = CARTESIAN_POINT ( 'NONE',  ( 767.7687537140311633, -95.90732993114751537, -372.7932403749916830 ) ) ;
#11978 = CARTESIAN_POINT ( 'NONE',  ( 763.8424801807145741, -18.00906357242611477, 320.5453621957614700 ) ) ;
#11979 = CARTESIAN_POINT ( 'NONE',  ( 767.7687537140311633, -359.9073299311467053, -372.7932403749916830 ) ) ;
#11980 = CARTESIAN_POINT ( 'NONE',  ( -115.7583438952258774, 290.0000000000001705, -244.9999999999999716 ) ) ;
#11981 = CARTESIAN_POINT ( 'NONE',  ( 758.6633372737375112, -404.5328690171409107, 326.9102291470432533 ) ) ;
#11982 = ORIENTED_EDGE ( 'NONE', *, *, #30859, .F. ) ;
#11983 = CARTESIAN_POINT ( 'NONE',  ( 770.0799878456142551, -85.98741447168738716, 362.9823548866085616 ) ) ;
#11984 = CARTESIAN_POINT ( 'NONE',  ( 767.8955696845333705, -408.4527844766009252, -362.1676090361162323 ) ) ;
#11985 = ADVANCED_FACE ( 'NONE', ( #13103 ), #26494, .F. ) ;
#11986 = CARTESIAN_POINT ( 'NONE',  ( 771.2633955100217236, -215.9073299311471317, -363.4237431249939618 ) ) ;
#11987 = AXIS2_PLACEMENT_3D ( 'NONE', #23697, #23475, #20021 ) ;
#11988 = CARTESIAN_POINT ( 'NONE',  ( 744.9990715423526808, -114.3510508353236617, -341.2370466360926002 ) ) ;
#11989 = DIRECTION ( 'NONE',  ( -1.880165489482579047E-16, -1.000000000000000000, -0.000000000000000000 ) ) ;
#11990 = CARTESIAN_POINT ( 'NONE',  ( 776.2433038121456548, -252.8965053807777394, 374.8207195650711014 ) ) ;
#11991 = CARTESIAN_POINT ( 'NONE',  ( 797.8594530101009923, -37.54369356751133324, 322.1405469898982119 ) ) ;
#11992 = ORIENTED_EDGE ( 'NONE', *, *, #35171, .F. ) ;
#11993 = CARTESIAN_POINT ( 'NONE',  ( 804.9511171171677688, -245.8055962898686460, -335.8780910478229202 ) ) ;
#11994 = CARTESIAN_POINT ( 'NONE',  ( 781.8018195045266339, -238.2709662947833920, 365.1927285166406705 ) ) ;
#11995 = CARTESIAN_POINT ( 'NONE',  ( 751.2241431872005251, -424.1692326535044799, -359.9636004259367610 ) ) ;
#11996 = CARTESIAN_POINT ( 'NONE',  ( 744.8212110874229666, -66.89650538077835051, -336.2046728542121627 ) ) ;
#11997 = CYLINDRICAL_SURFACE ( 'NONE', #27615, 1.000000000000000888 ) ;
#11998 = ADVANCED_FACE ( 'NONE', ( #42403 ), #8641, .F. ) ;
#11999 = ORIENTED_EDGE ( 'NONE', *, *, #2395, .F. ) ;
#12000 = ORIENTED_EDGE ( 'NONE', *, *, #18568, .T. ) ;
#12001 = CARTESIAN_POINT ( 'NONE',  ( 778.7629533639073998, -368.7363362996977685, -375.0009284576466371 ) ) ;
#12002 = ADVANCED_FACE ( 'NONE', ( #6399 ), #38723, .F. ) ;
#12003 = CARTESIAN_POINT ( 'NONE',  ( 744.7301800767020268, -292.8164208402378108, 337.4774526936615189 ) ) ;
#12004 = CARTESIAN_POINT ( 'NONE',  ( 813.9316612368132837, -31.44195992623299674, 348.6739635108323228 ) ) ;
#12005 = EDGE_CURVE ( 'NONE', #41282, #4399, #10310, .T. ) ;
#12006 = CARTESIAN_POINT ( 'NONE',  ( 796.1575198192839480, -174.0090635724256742, -359.4546378042384163 ) ) ;
#12007 = CARTESIAN_POINT ( 'NONE',  ( 778.1981804954714335, -178.2709662947835625, -314.8072714833589885 ) ) ;
#12008 = CARTESIAN_POINT ( 'NONE',  ( 797.6776695296629214, -379.5436935675102745, -357.6776695296636603 ) ) ;
#12009 = ORIENTED_EDGE ( 'NONE', *, *, #78, .T. ) ;
#12010 = CARTESIAN_POINT ( 'NONE',  ( 764.8639956371174549, -200.0891481129653187, 319.7806653035542013 ) ) ;
#12011 = CARTESIAN_POINT ( 'NONE',  ( 763.2154366446407039, 26.37622189194863509, -321.4292242960311228 ) ) ;
#12012 = ORIENTED_EDGE ( 'NONE', *, *, #22981, .T. ) ;
#12013 = CARTESIAN_POINT ( 'NONE',  ( 808.0189434323515343, -326.0891481129649492, 319.0252816721025511 ) ) ;
#12014 = CARTESIAN_POINT ( 'NONE',  ( 779.9999999999992042, 126.4563064324884465, 309.9999999999998863 ) ) ;
#12015 = LINE ( 'NONE', #36941, #27776 ) ;
#12016 = CARTESIAN_POINT ( 'NONE',  ( 914.9999999999992042, 99.99999999999984368, 350.0000000000000000 ) ) ;
#12017 = CARTESIAN_POINT ( 'NONE',  ( 787.5531968255692163, -189.8272453906073736, 316.1348686366205811 ) ) ;
#12018 = CARTESIAN_POINT ( 'NONE',  ( 762.3223304703356007, -55.54369356751127640, 322.3223304703362828 ) ) ;
#12019 = VERTEX_POINT ( 'NONE', #14015 ) ;
#12020 = CARTESIAN_POINT ( 'NONE',  ( 795.8262568251477660, -406.3726999360612808, -308.3538107759623585 ) ) ;
#12021 = CIRCLE ( 'NONE', #15706, 6.118999999999985562 ) ;
#12022 = CARTESIAN_POINT ( 'NONE',  ( 755.2512626584698410, -31.54369356751135456, -315.2512626584710915 ) ) ;
#12023 = CARTESIAN_POINT ( 'NONE',  ( 764.0069404352550464, -207.0783235625960685, 359.2566176426627180 ) ) ;
#12024 = CARTESIAN_POINT ( 'NONE',  ( 765.0180583372156207, -408.9982390220556567, -360.0135310231089534 ) ) ;
#12025 = CARTESIAN_POINT ( 'NONE',  ( 804.6798772138710092, -15.72551174932958951, -334.6312213355106451 ) ) ;
#12026 = ADVANCED_FACE ( 'NONE', ( #38043 ), #31564, .F. ) ;
#12027 = CARTESIAN_POINT ( 'NONE',  ( 782.4968714119720516, -418.8164208402374129, 305.0891759886411023 ) ) ;
#12028 = CARTESIAN_POINT ( 'NONE',  ( -468.8365100919714337, 256.5000000000001705, -199.9999999999908766 ) ) ;
#12029 = CARTESIAN_POINT ( 'NONE',  ( 755.1538015810308480, -254.1908817542435770, -343.0433043558613804 ) ) ;
#12030 = CARTESIAN_POINT ( 'NONE',  ( 800.9747183278959710, -156.9982390220564241, -311.9810565676471583 ) ) ;
#12031 = EDGE_CURVE ( 'NONE', #45689, #41099, #24850, .T. ) ;
#12032 = CARTESIAN_POINT ( 'NONE',  ( 811.0346526505616112, -38.63460265842041252, 323.0537975583477532 ) ) ;
#12033 = CARTESIAN_POINT ( 'NONE',  ( 782.5225473063381969, -118.2709662947837899, 375.2698199232970637 ) ) ;
#12034 = CARTESIAN_POINT ( 'NONE',  ( 51.16348990802859475, 256.5000000000000568, -193.8809999999945148 ) ) ;
#12035 = LINE ( 'NONE', #26103, #4041 ) ;
#12036 = CARTESIAN_POINT ( 'NONE',  ( 752.7379699480933368, -396.0090635724249637, 361.9858362298580232 ) ) ;
#12037 = DIRECTION ( 'NONE',  ( -1.000000000000000000, -0.000000000000000000, 0.000000000000000000 ) ) ;
#12038 = CARTESIAN_POINT ( 'NONE',  ( 792.3570229623688874, -357.1800572038739006, 373.1304606946836202 ) ) ;
#12039 = ADVANCED_FACE ( 'NONE', ( #42180 ), #20482, .T. ) ;
#12040 = CARTESIAN_POINT ( 'NONE',  ( 771.1735550268778070, -321.1800572038740142, -316.3353852180827630 ) ) ;
#12041 = CARTESIAN_POINT ( 'NONE',  ( 790.8050863131179540, -452.8379544210779954, 362.5841948692291226 ) ) ;
#12042 = CARTESIAN_POINT ( 'NONE',  ( 745.1792804349281596, -110.1908817542440033, -343.7566961878542884 ) ) ;
#12043 = CARTESIAN_POINT ( 'NONE',  ( 761.2382568024794409, -111.6237781080509279, -356.9571628226838129 ) ) ;
#12044 = CARTESIAN_POINT ( 'NONE',  ( 781.2497674668890113, -132.3510508353235764, 375.3608509340180603 ) ) ;
#12045 = CARTESIAN_POINT ( 'NONE',  ( 778.1981804954715471, -442.2709662947827383, 314.8072714833591021 ) ) ;
#12046 = CARTESIAN_POINT ( 'NONE',  ( 756.5762568750052424, -27.18005720387500901, -348.7366044899774238 ) ) ;
#12047 = CARTESIAN_POINT ( 'NONE',  ( 770.0799878456142551, -133.9874144716872024, -362.9823548866085616 ) ) ;
#12048 = CARTESIAN_POINT ( 'NONE',  ( 756.5762568750052424, -123.1800572038747106, -348.7366044899774238 ) ) ;
#12049 = CARTESIAN_POINT ( 'NONE',  ( 757.8323909638827445, -122.6346026584201354, 352.1044303154654358 ) ) ;
#12050 = CARTESIAN_POINT ( 'NONE',  ( 793.2243759319678702, -434.5328690171407970, -318.4439275373583200 ) ) ;
#12052 = CARTESIAN_POINT ( 'NONE',  ( 757.8323909638828582, -266.6346026584197375, 352.1044303154654358 ) ) ;
#12051 = CARTESIAN_POINT ( 'NONE',  ( 800.2193346964447755, -258.9982390220561115, 355.1360043628815788 ) ) ;
#12053 = DIRECTION ( 'NONE',  ( 0.000000000000000000, 0.000000000000000000, -1.000000000000000000 ) ) ;
#12054 = VERTEX_POINT ( 'NONE', #30875 ) ;
#12055 = CARTESIAN_POINT ( 'NONE',  ( 794.1144889064781864, 13.83076734649413098, 360.9840315886528401 ) ) ;
#12056 = PRODUCT_DEFINITION_FORMATION_WITH_SPECIFIED_SOURCE ( 'ANY', '', #21473, .NOT_KNOWN. ) ;
#12057 = EDGE_LOOP ( 'NONE', ( #43732, #14806, #1924, #36036 ) ) ;
#12058 = DIRECTION ( 'NONE',  ( 1.000000000000000000, 0.000000000000000000, 0.000000000000000000 ) ) ;
#12059 = CARTESIAN_POINT ( 'NONE',  ( 755.2512626584698410, -199.5436935675108430, 315.2512626584710915 ) ) ;
#12060 = CARTESIAN_POINT ( 'NONE',  ( 773.4516893846965786, -283.6454272087889308, 315.8398074228977066 ) ) ;
#12061 = CARTESIAN_POINT ( 'NONE',  ( 754.8983024940795303, -402.8965053807773415, 336.9254006560228163 ) ) ;
#12062 = ORIENTED_EDGE ( 'NONE', *, *, #18732, .T. ) ;
#12063 = CARTESIAN_POINT ( 'NONE',  ( 755.8894580844503253, -63.82724539060779279, -332.3691319403863531 ) ) ;
#12064 = CARTESIAN_POINT ( 'NONE',  ( 792.1044303154646968, -276.4527844766014368, -317.8323909638837677 ) ) ;
#12065 = ORIENTED_EDGE ( 'NONE', *, *, #17608, .T. ) ;
#12066 = CARTESIAN_POINT ( 'NONE',  ( 797.6776695296629214, -403.5436935675101608, -357.6776695296636603 ) ) ;
#12067 = CARTESIAN_POINT ( 'NONE',  ( 800.0135310231082713, -38.08914811296587999, -325.0180583372163028 ) ) ;
#12068 = MECHANICAL_DESIGN_GEOMETRIC_PRESENTATION_REPRESENTATION (  '', ( #20883 ), #41569 ) ;
#12069 = CARTESIAN_POINT ( 'NONE',  ( 803.8651313633788504, -269.2601417444139997, 332.4468031744301015 ) ) ;
#12070 = CARTESIAN_POINT ( 'NONE',  ( -789.9999999999992042, 240.0000000000000568, -319.9999999999999432 ) ) ;
#12071 = CARTESIAN_POINT ( 'NONE',  ( 759.9999999999992042, 166.4563064324884465, -360.0000000000000000 ) ) ;
#12072 = CARTESIAN_POINT ( 'NONE',  ( 807.2620300519052989, -24.00906357242609346, -318.0141637701419768 ) ) ;
#12073 = DIRECTION ( 'NONE',  ( 1.880165489482579047E-16, 1.000000000000000000, 0.000000000000000000 ) ) ;
#12074 = ORIENTED_EDGE ( 'NONE', *, *, #43019, .T. ) ;
#12075 = CARTESIAN_POINT ( 'NONE',  ( 795.8262568251477660, -310.3726999360616219, -308.3538107759623585 ) ) ;
#12076 = CARTESIAN_POINT ( 'NONE',  ( 764.1737431748507561, -154.3726999360620198, 371.6461892240376415 ) ) ;
#12078 = CARTESIAN_POINT ( 'NONE',  ( 805.1927285166397041, -280.8164208402378677, -341.8018195045277707 ) ) ;
#12077 = DIRECTION ( 'NONE',  ( 0.000000000000000000, -0.9238795325112892920, 0.3826834323650836756 ) ) ;
#12079 = EDGE_CURVE ( 'NONE', #38375, #637, #35247, .T. ) ;
#12080 = SURFACE_STYLE_FILL_AREA ( #33315 ) ;
#12081 = CARTESIAN_POINT ( 'NONE',  ( 773.4516893846965786, -163.6454272087893003, -315.8398074228977066 ) ) ;
#12082 = CARTESIAN_POINT ( 'NONE',  ( 792.3570229623688874, -21.18005720387502677, 373.1304606946836202 ) ) ;
#12083 = VECTOR ( 'NONE', #40338, 1000.000000000000000 ) ;
#12084 = CARTESIAN_POINT ( 'NONE',  ( 879.9999999999990905, -414.5899773927342835, 210.0000000000000000 ) ) ;
#12085 = CARTESIAN_POINT ( 'NONE',  ( 815.2698199232962679, -352.8164208402375266, -342.5225473063383674 ) ) ;
#12086 = AXIS2_PLACEMENT_3D ( 'NONE', #15102, #7715, #29192 ) ;
#12087 = DIRECTION ( 'NONE',  ( 0.000000000000000000, -0.9238795325112892920, 0.3826834323650836756 ) ) ;
#12088 = CARTESIAN_POINT ( 'NONE',  ( 756.3353852180819104, -29.90732993114771787, 331.1735550268788302 ) ) ;
#12089 = CARTESIAN_POINT ( 'NONE',  ( 749.5768839229115201, -276.5545181178798657, 358.0661480581553064 ) ) ;
#12090 = CARTESIAN_POINT ( 'NONE',  ( 749.2812353651451076, -270.4527844766014937, 323.2262854647983090 ) ) ;
#12091 = CARTESIAN_POINT ( 'NONE',  ( 749.8865473780648472, -428.5328690171409107, -322.1177392798429082 ) ) ;
#12092 = FACE_OUTER_BOUND ( 'NONE', #20619, .T. ) ;
#12093 = PLANE ( 'NONE',  #22449 ) ;
#12094 = CARTESIAN_POINT ( 'NONE',  ( 768.0187753319979720, -368.6346026584193964, 318.0580252608186242 ) ) ;
#12095 = CARTESIAN_POINT ( 'NONE',  ( 763.8424801807145741, -114.0090635724258163, 320.5453621957614700 ) ) ;
#12096 = CARTESIAN_POINT ( 'NONE',  ( 804.1601925771018387, -7.441959926233078448, -346.5483106153029098 ) ) ;
#12097 = DIRECTION ( 'NONE',  ( 0.000000000000000000, 0.000000000000000000, -1.000000000000000000 ) ) ;
#12098 = AXIS2_PLACEMENT_3D ( 'NONE', #2639, #28029, #42123 ) ;
#12099 = LINE ( 'NONE', #43723, #33619 ) ;
#12100 = CARTESIAN_POINT ( 'NONE',  ( 800.1688906516307043, -130.1692326535054463, 369.0717654672308186 ) ) ;
#12101 = CARTESIAN_POINT ( 'NONE',  ( 802.1676090361156639, -398.6346026584193396, 327.8955696845344505 ) ) ;
#12102 = ORIENTED_EDGE ( 'NONE', *, *, #39058, .T. ) ;
#12103 = CARTESIAN_POINT ( 'NONE',  ( 787.6308680596127942, -323.2601417444138860, -364.1105419155492768 ) ) ;
#12104 = CARTESIAN_POINT ( 'NONE',  ( 762.3223304703356007, -151.5436935675109851, 322.3223304703362828 ) ) ;
#12105 = UNCERTAINTY_MEASURE_WITH_UNIT (LENGTH_MEASURE( 1.000000000000000082E-05 ), #12261, 'distance_accuracy_value', 'NONE');
#12106 = CARTESIAN_POINT ( 'NONE',  ( 811.6461892240364477, -316.7146871989593819, -324.1737431748509835 ) ) ;
#12107 = LINE ( 'NONE', #26186, #20466 ) ;
#12108 = VERTEX_POINT ( 'NONE', #41967 ) ;
#12109 = CARTESIAN_POINT ( 'NONE',  ( 755.5713283507202505, -341.3618753856922012, 334.6858677611754729 ) ) ;
#12110 = EDGE_LOOP ( 'NONE', ( #44312, #2847, #235, #25524 ) ) ;
#12111 = CARTESIAN_POINT ( 'NONE',  ( 785.3141322388236176, -429.7255117493282910, 364.4286716492789537 ) ) ;
#12112 = CARTESIAN_POINT ( 'NONE',  ( 808.0189434323515343, -182.0891481129654323, -319.0252816721025511 ) ) ;
#12113 = CARTESIAN_POINT ( 'NONE',  ( 772.4837098697145166, -71.36187538569303968, 374.5518280994205611 ) ) ;
#12114 = VERTEX_POINT ( 'NONE', #27871 ) ;
#12115 = CARTESIAN_POINT ( 'NONE',  ( 785.3141322388236176, -165.7255117493291152, -364.4286716492789537 ) ) ;
#12116 = AXIS2_PLACEMENT_3D ( 'NONE', #11858, #4482, #25931 ) ;
#12117 = ORIENTED_EDGE ( 'NONE', *, *, #27763, .T. ) ;
#12118 = CARTESIAN_POINT ( 'NONE',  ( 804.6971507214547046, -435.2817908451521021, -344.0799538623459739 ) ) ;
#12119 = CARTESIAN_POINT ( 'NONE',  ( 794.9819416627830151, 11.00176097794305541, 319.9864689768909898 ) ) ;
#12120 = CARTESIAN_POINT ( 'NONE',  ( 800.7704444035546203, -148.1692326535053610, 326.0291762391768771 ) ) ;
#12122 = CARTESIAN_POINT ( 'NONE',  ( -728.8365100919714905, 260.0000000000001705, -191.9749999999891372 ) ) ;
#12121 = CARTESIAN_POINT ( 'NONE',  ( 57.28248990802860163, 256.5000000000000568, -199.9999999999945146 ) ) ;
#12123 = ORIENTED_EDGE ( 'NONE', *, *, #19325, .T. ) ;
#12124 = CARTESIAN_POINT ( 'NONE',  ( 766.0291762391763086, -418.9181544815157849, -360.7704444035551319 ) ) ;
#12125 = CARTESIAN_POINT ( 'NONE',  ( 786.4999999999993179, -513.1383975375929367, -369.9999999999999432 ) ) ;
#12126 = CARTESIAN_POINT ( 'NONE',  ( 812.3518521366052028, -193.0999726633346256, -326.5853460496235243 ) ) ;
#12127 = CARTESIAN_POINT ( 'NONE',  ( 760.0363995740630116, -82.91815448151682233, 368.7758568127991907 ) ) ;
#12128 = VECTOR ( 'NONE', #29085, 1000.000000000000000 ) ;
#12130 = CARTESIAN_POINT ( 'NONE',  ( 757.8323909638827445, -170.6346026584199649, -352.1044303154654358 ) ) ;
#12129 = CARTESIAN_POINT ( 'NONE',  ( -829.9999999999992042, 430.0000000000002842, -319.9999999999996021 ) ) ;
#12131 = CARTESIAN_POINT ( 'NONE',  ( 805.0264073115434940, -342.3510508353228943, -339.4763451958999099 ) ) ;
#12132 = DIRECTION ( 'NONE',  ( 0.000000000000000000, 0.000000000000000000, -1.000000000000000000 ) ) ;
#12133 = CARTESIAN_POINT ( 'NONE',  ( 809.0717654672305343, -220.9181544815164102, -360.1688906516309885 ) ) ;
#12134 = DIRECTION ( 'NONE',  ( 0.000000000000000000, -0.9235249282889854694, -0.3835384033298675499 ) ) ;
#12135 = CARTESIAN_POINT ( 'NONE',  ( -919.9999999999993179, 219.9999999999998863, 350.0000000000000000 ) ) ;
#12136 = CARTESIAN_POINT ( 'NONE',  ( 766.0291762391763086, -34.91815448151697154, -360.7704444035551319 ) ) ;
#12137 = CARTESIAN_POINT ( 'NONE',  ( 786.5483106153019435, -415.6454272087885897, 364.1601925771022366 ) ) ;
#12138 = CIRCLE ( 'NONE', #22432, 6.118999999999985562 ) ;
#12139 = CARTESIAN_POINT ( 'NONE',  ( 792.2312462859673587, -227.9073299311471033, -307.2067596250082602 ) ) ;
#12140 = CARTESIAN_POINT ( 'NONE',  ( 780.5236548040995785, -236.7363362996981380, 314.9735926884559944 ) ) ;
#12141 = LINE ( 'NONE', #19751, #37895 ) ;
#12142 = CARTESIAN_POINT ( 'NONE',  ( 756.3353852180819104, -5.907329931147798696, -331.1735550268788302 ) ) ;
#12143 = CARTESIAN_POINT ( 'NONE',  ( 810.4231160770870019, -192.5545181178801215, 321.9338519418446936 ) ) ;
#12144 = CARTESIAN_POINT ( 'NONE',  ( 783.7566961878529810, -120.8965053807781800, -305.1792804349288417 ) ) ;
#12145 = CARTESIAN_POINT ( 'NONE',  ( 805.0032342141412300, -157.5436935675108998, 314.9967657858571783 ) ) ;
#12146 = CARTESIAN_POINT ( 'NONE',  ( 745.4481719005789273, -363.7255117493284047, -347.5162901302853129 ) ) ;
#12147 = CARTESIAN_POINT ( 'NONE',  ( -338.8365100919713200, 230.0000000000001137, -199.9999999999917861 ) ) ;
#12148 = FACE_OUTER_BOUND ( 'NONE', #35052, .T. ) ;
#12149 = CARTESIAN_POINT ( 'NONE',  ( 788.8264449731200330, -261.1800572038741848, 363.6646147819171233 ) ) ;
#12150 = VECTOR ( 'NONE', #17827, 1000.000000000000000 ) ;
#12151 = CARTESIAN_POINT ( 'NONE',  ( 801.5560724626406000, -24.55451811788064020, 326.7756240680316182 ) ) ;
#12152 = CARTESIAN_POINT ( 'NONE',  ( 785.3687786644884454, -395.3618753856918602, -315.3201227861279676 ) ) ;
#12153 = VECTOR ( 'NONE', #14882, 1000.000000000000000 ) ;
#12154 = DIRECTION ( 'NONE',  ( 1.000000000000000000, 0.000000000000000000, 0.000000000000000000 ) ) ;
#12155 = CARTESIAN_POINT ( 'NONE',  ( 791.0478386215596629, 2.172754609392001601, -306.7653713866226326 ) ) ;
#12156 = CARTESIAN_POINT ( 'NONE',  ( 775.4999999999993179, -365.3551492539851893, -8.132432514707076621 ) ) ;
#12157 = CARTESIAN_POINT ( 'NONE',  ( 798.7617431975189675, -51.62377810805111267, 323.0428371773161871 ) ) ;
#12158 = ORIENTED_EDGE ( 'NONE', *, *, #37965, .T. ) ;
#12159 = CARTESIAN_POINT ( 'NONE',  ( 803.8651313633788504, -221.2601417444142271, -332.4468031744301015 ) ) ;
#12160 = CARTESIAN_POINT ( 'NONE',  ( 762.1405469898971887, -25.54369356751136877, 357.8594530101015607 ) ) ;
#12161 = CARTESIAN_POINT ( 'NONE',  ( 791.1614460488616487, -227.2601417444141987, -373.5763878283158874 ) ) ;
#12162 = CARTESIAN_POINT ( 'NONE',  ( 772.4999999999993179, -462.9681489794447202, -270.0000000000000568 ) ) ;
#12163 = CARTESIAN_POINT ( 'NONE',  ( 747.3154664389472828, -331.9874144716865203, 326.4474001241230781 ) ) ;
#12164 = EDGE_LOOP ( 'NONE', ( #43790, #21589, #34080, #36443 ) ) ;
#12165 = CIRCLE ( 'NONE', #6250, 20.00000000000001776 ) ;
#12166 = CARTESIAN_POINT ( 'NONE',  ( 768.0187753319979720, -152.6346026584200786, -318.0580252608186242 ) ) ;
#12167 = CARTESIAN_POINT ( 'NONE',  ( 803.4237431249931660, -327.1800572038741279, 331.2633955100225194 ) ) ;
#12168 = AXIS2_PLACEMENT_3D ( 'NONE', #17679, #17447, #27370 ) ;
#12169 = CARTESIAN_POINT ( 'NONE',  ( 792.2312462859673587, -83.90732993114754379, -307.2067596250082602 ) ) ;
#12170 = AXIS2_PLACEMENT_3D ( 'NONE', #36840, #26442, #22513 ) ;
#12171 = CARTESIAN_POINT ( 'NONE',  ( 755.5713283507202505, -77.36187538569302546, -334.6858677611754729 ) ) ;
#12172 = ORIENTED_EDGE ( 'NONE', *, *, #16501, .T. ) ;
#12173 = CARTESIAN_POINT ( 'NONE',  ( 796.9571628226829034, 0.5363909730283709099, -321.2382568024804641 ) ) ;
#12174 = VERTEX_POINT ( 'NONE', #35014 ) ;
#12175 = CARTESIAN_POINT ( 'NONE',  ( 787.5531968255692163, -309.8272453906070041, -316.1348686366205811 ) ) ;
#12177 = CARTESIAN_POINT ( 'NONE',  ( 763.8424801807145741, -354.0090635724250774, 320.5453621957614700 ) ) ;
#12176 = CARTESIAN_POINT ( 'NONE',  ( 791.9812246680005501, -68.63460265842033436, 361.9419747391813189 ) ) ;
#12180 = CARTESIAN_POINT ( 'NONE',  ( 808.7758568127978833, -316.1692326535048210, 320.0363995740631822 ) ) ;
#12179 = CARTESIAN_POINT ( 'NONE',  ( 1007.605605532488426, -292.9981031064102126, 121.3637880562633171 ) ) ;
#12178 = CARTESIAN_POINT ( 'NONE',  ( 804.7487373415286811, -427.5436935675101040, 364.7487373415288516 ) ) ;
#12181 = CIRCLE ( 'NONE', #23955, 6.119000000000013095 ) ;
#12182 = CARTESIAN_POINT ( 'NONE',  ( 749.8865473780648472, -92.53286901714190549, 322.1177392798429082 ) ) ;
#12183 = CARTESIAN_POINT ( 'NONE',  ( 776.9254006560222479, -332.1908817542433781, -314.8983024940802125 ) ) ;
#12184 = CARTESIAN_POINT ( 'NONE',  ( 768.0187753319979720, -320.6346026584195670, -318.0580252608186242 ) ) ;
#12185 = CARTESIAN_POINT ( 'NONE',  ( 795.1360043628807261, -140.0891481129654892, -360.2193346964456282 ) ) ;
#12186 = PRESENTATION_LAYER_ASSIGNMENT (  '', '', ( #15125 ) ) ;
#12187 = CARTESIAN_POINT ( 'NONE',  ( 787.5162901302840055, -419.3618753856918033, 305.4481719005792684 ) ) ;
#12188 = CIRCLE ( 'NONE', #1103, 12.00000000000001066 ) ;
#12190 = CARTESIAN_POINT ( 'NONE',  ( 701.1634899080286232, 256.4999999999999432, -193.8809999999990623 ) ) ;
#12189 = DIRECTION ( 'NONE',  ( 1.337618101958019798E-16, -1.000000000000000000, 0.000000000000000000 ) ) ;
#12191 = CARTESIAN_POINT ( 'NONE',  ( 807.2620300519052989, -120.0090635724258021, -318.0141637701419768 ) ) ;
#12192 = DIRECTION ( 'NONE',  ( -1.000000000000000000, 0.000000000000000000, 0.000000000000000000 ) ) ;
#12193 = DIRECTION ( 'NONE',  ( -0.000000000000000000, 1.000000000000000000, -0.000000000000000000 ) ) ;
#12194 = ADVANCED_FACE ( 'NONE', ( #13794 ), #31093, .F. ) ;
#12195 = CARTESIAN_POINT ( 'NONE',  ( 796.9571628226829034, -311.4636090269706870, 321.2382568024804641 ) ) ;
#12196 = CARTESIAN_POINT ( 'NONE',  ( 755.3201227861273992, -171.7255117493291152, 345.3687786644892981 ) ) ;
#12197 = VERTEX_POINT ( 'NONE', #17485 ) ;
#12198 = CARTESIAN_POINT ( 'NONE',  ( 747.2067596250078623, -123.1800572038747106, -352.2312462859687230 ) ) ;
#12199 = DIRECTION ( 'NONE',  ( 0.000000000000000000, 0.000000000000000000, 1.000000000000000000 ) ) ;
#12200 = AXIS2_PLACEMENT_3D ( 'NONE', #27371, #10497, #38236 ) ;
#12201 = CARTESIAN_POINT ( 'NONE',  ( 771.3260364891663130, -67.64542720878958448, 306.0683387631859773 ) ) ;
#12202 = CARTESIAN_POINT ( 'NONE',  ( 782.5225473063381969, -262.2709662947831930, -375.2698199232970637 ) ) ;
#12203 = AXIS2_PLACEMENT_3D ( 'NONE', #22039, #35659, #17896 ) ;
#12204 = CARTESIAN_POINT ( 'NONE',  ( 792.2312462859673587, -443.9073299311464780, -307.2067596250082602 ) ) ;
#12205 = CARTESIAN_POINT ( 'NONE',  ( 800.2193346964447755, -162.9982390220563673, 355.1360043628815788 ) ) ;
#12206 = CARTESIAN_POINT ( 'NONE',  ( 793.4146539503750546, -337.9874144716865771, -307.6481478633938877 ) ) ;
#12207 = CARTESIAN_POINT ( 'NONE',  ( 745.4481719005789273, -75.72551174932937101, -347.5162901302853129 ) ) ;
#12208 = CARTESIAN_POINT ( 'NONE',  ( 796.1575198192839480, -30.00906357242607925, 359.4546378042384163 ) ) ;
#12209 = CARTESIAN_POINT ( 'NONE',  ( 746.8695393053150156, -341.9073299311465917, -327.6429770376306010 ) ) ;
#12210 = DIRECTION ( 'NONE',  ( 0.000000000000000000, -1.000000000000000000, 0.000000000000000000 ) ) ;
#12211 = CARTESIAN_POINT ( 'NONE',  ( 794.1144889064781864, -394.1692326535045368, 360.9840315886528401 ) ) ;
#12212 = ORIENTED_EDGE ( 'NONE', *, *, #30317, .T. ) ;
#12213 = CARTESIAN_POINT ( 'NONE',  ( 771.1735550268778070, -225.1800572038743269, -316.3353852180827630 ) ) ;
#12214 = VECTOR ( 'NONE', #2393, 1000.000000000000000 ) ;
#12215 = CARTESIAN_POINT ( 'NONE',  ( 745.1769319972822814, -113.8055962898691149, -346.2694204179732083 ) ) ;
#12216 = CARTESIAN_POINT ( 'NONE',  ( 787.4999999999992042, -512.9681489794448908, 309.9999999999998863 ) ) ;
#12217 = CARTESIAN_POINT ( 'NONE',  ( 748.3538107759620743, -256.7146871989595525, 355.8262568251490165 ) ) ;
#12218 = CARTESIAN_POINT ( 'NONE',  ( 792.1044303154646968, -60.45278447660216159, 317.8323909638837677 ) ) ;
#12219 = VERTEX_POINT ( 'NONE', #2928 ) ;
#12220 = VECTOR ( 'NONE', #15862, 1000.000000000000000 ) ;
#12221 = CARTESIAN_POINT ( 'NONE',  ( 780.5290396650775619, -228.3510508353232922, -365.2837595273619513 ) ) ;
#12222 = CARTESIAN_POINT ( 'NONE',  ( 805.1927285166397041, -232.8164208402379245, 341.8018195045277707 ) ) ;
#12223 = CARTESIAN_POINT ( 'NONE',  ( 815.0009284576459549, -438.3510508353226669, -338.7629533639073429 ) ) ;
#12224 = CARTESIAN_POINT ( 'NONE',  ( 754.0944755984390895, -63.62377810805107714, -364.1009440267246760 ) ) ;
#12225 = DIRECTION ( 'NONE',  ( 1.000000000000000000, 0.000000000000000000, 0.000000000000000000 ) ) ;
#12226 = ORIENTED_EDGE ( 'NONE', *, *, #37930, .T. ) ;
#12227 = EDGE_LOOP ( 'NONE', ( #34181, #28538, #45472, #41876 ) ) ;
#12228 = CARTESIAN_POINT ( 'NONE',  ( 745.7194118038753459, -373.6454272087887034, -348.7631598425976449 ) ) ;
#12229 = AXIS2_PLACEMENT_3D ( 'NONE', #8858, #4709, #26177 ) ;
#12230 = AXIS2_PLACEMENT_3D ( 'NONE', #24153, #38262, #20684 ) ;
#12231 = CARTESIAN_POINT ( 'NONE',  ( 815.2698199232962679, -328.8164208402375834, 342.5225473063383674 ) ) ;
#12232 = ADVANCED_FACE ( 'NONE', ( #17238 ), #3625, .T. ) ;
#12233 = CARTESIAN_POINT ( 'NONE',  ( 744.9990715423526808, -42.35105083532388193, 341.2370466360926002 ) ) ;
#12234 = CARTESIAN_POINT ( 'NONE',  ( 757.0176451133909268, -229.0999726633345404, -349.9200121543848354 ) ) ;
#12235 = CARTESIAN_POINT ( 'NONE',  ( 802.1676090361156639, -182.6346026584199649, -327.8955696845344505 ) ) ;
#12236 = CARTESIAN_POINT ( 'NONE',  ( 795.1360043628808398, -380.0891481129647218, -360.2193346964456282 ) ) ;
#12237 = ORIENTED_EDGE ( 'NONE', *, *, #16989, .F. ) ;
#12238 = CARTESIAN_POINT ( 'NONE',  ( 791.9812246680005501, -212.6346026584198796, 361.9419747391813189 ) ) ;
#12239 = CARTESIAN_POINT ( 'NONE',  ( 785.3141322388236176, -117.7255117493292715, -364.4286716492789537 ) ) ;
#12240 = ORIENTED_EDGE ( 'NONE', *, *, #28933, .T. ) ;
#12241 = CARTESIAN_POINT ( 'NONE',  ( 782.5225473063381969, -310.2709662947832499, 375.2698199232970637 ) ) ;
#12242 = DIRECTION ( 'NONE',  ( 0.000000000000000000, 0.000000000000000000, 1.000000000000000000 ) ) ;
#12243 = FACE_OUTER_BOUND ( 'NONE', #23839, .T. ) ;
#12244 = DIRECTION ( 'NONE',  ( -0.7071067811857625340, 8.659560562345319848E-17, 0.7071067811873326114 ) ) ;
#12245 = EDGE_CURVE ( 'NONE', #41109, #23212, #41500, .T. ) ;
#12246 = CARTESIAN_POINT ( 'NONE',  ( 755.1538015810308480, -182.1908817542437760, 343.0433043558613804 ) ) ;
#12247 = CARTESIAN_POINT ( 'NONE',  ( 781.8018195045266339, -94.27096629478386092, 365.1927285166406705 ) ) ;
#12248 = ORIENTED_EDGE ( 'NONE', *, *, #18500, .F. ) ;
#12249 = CARTESIAN_POINT ( 'NONE',  ( 814.8207195650702488, -458.1908817542429802, -336.2433038121456548 ) ) ;
#12250 = CARTESIAN_POINT ( 'NONE',  ( 754.9967657858570647, -49.54369356751129772, -365.0032342141425943 ) ) ;
#12251 = CARTESIAN_POINT ( 'NONE',  ( 757.2208543904082489, -256.7146871989595525, 350.9844846989624330 ) ) ;
#12252 = CARTESIAN_POINT ( 'NONE',  ( 755.5713283507202505, -413.3618753856920307, -334.6858677611754729 ) ) ;
#12253 = CARTESIAN_POINT ( 'NONE',  ( 767.8955696845334842, -24.45278447660228949, -362.1676090361161755 ) ) ;
#12254 = CARTESIAN_POINT ( 'NONE',  ( 812.7932403749906598, -423.1800572038737300, 327.7687537140311633 ) ) ;
#12255 = FACE_OUTER_BOUND ( 'NONE', #8819, .T. ) ;
#12256 = CARTESIAN_POINT ( 'NONE',  ( 769.9779781133707957, -259.0999726633343698, -316.7813123517150871 ) ) ;
#12257 = CARTESIAN_POINT ( 'NONE',  ( 808.3070685750230950, -162.9982390220563673, -361.1904061080339261 ) ) ;
#12258 = CARTESIAN_POINT ( 'NONE',  ( 812.7932403749906598, -39.18005720387496638, 327.7687537140311633 ) ) ;
#12259 = CARTESIAN_POINT ( 'NONE',  ( 800.9747183278959710, -132.9982390220564810, 311.9810565676471583 ) ) ;
#12260 = CARTESIAN_POINT ( 'NONE',  ( 795.2725662613897839, 16.45630643248849267, -314.1785221222716586 ) ) ;
#12261 =( LENGTH_UNIT ( ) NAMED_UNIT ( * ) SI_UNIT ( .MILLI., .METRE. ) );
#12262 = EDGE_CURVE ( 'NONE', #19031, #19590, #42451, .T. ) ;
#12263 = VECTOR ( 'NONE', #15245, 1000.000000000000000 ) ;
#12264 = EDGE_CURVE ( 'NONE', #12399, #36235, #38968, .T. ) ;
#12265 = CARTESIAN_POINT ( 'NONE',  ( 879.9999999999992042, 579.9999999999998863, -320.0000000000000000 ) ) ;
#12266 = CARTESIAN_POINT ( 'NONE',  ( 801.1904061080336987, -356.0891481129647218, 368.3070685750235498 ) ) ;
#12267 = CARTESIAN_POINT ( 'NONE',  ( 803.6646147819161570, -305.9073299311467622, -348.8264449731210561 ) ) ;
#12268 = VECTOR ( 'NONE', #25409, 1000.000000000000000 ) ;
#12269 = CARTESIAN_POINT ( 'NONE',  ( 779.4709603349208464, 23.64894916467591912, 314.7162404726379918 ) ) ;
#12270 = EDGE_CURVE ( 'NONE', #41883, #28770, #31324, .T. ) ;
#12271 = CARTESIAN_POINT ( 'NONE',  ( 762.1177392798416577, -90.55451811788041994, -309.8865473780659272 ) ) ;
#12272 = CARTESIAN_POINT ( 'NONE',  ( 787.6308680596127942, -131.2601417444144829, -364.1105419155492768 ) ) ;
#12273 = CARTESIAN_POINT ( 'NONE',  ( 764.3348316497523456, -118.7146871989600072, 308.6759233522265617 ) ) ;
#12274 = CARTESIAN_POINT ( 'NONE',  ( 795.1360043628808398, -428.0891481129645513, 360.2193346964456282 ) ) ;
#12275 = CARTESIAN_POINT ( 'NONE',  ( 752.4576283171824116, -165.0783235625962391, 317.7880784355627952 ) ) ;
#12276 = CARTESIAN_POINT ( 'NONE',  ( 788.7366044899766848, -35.90732993114770011, -316.5762568750059813 ) ) ;
#12277 = CARTESIAN_POINT ( 'NONE',  ( 805.1016975059191054, -126.8965053807781516, -343.0745993439771837 ) ) ;
#12278 = CARTESIAN_POINT ( 'NONE',  ( 758.0580252608178853, -126.4527844766019626, -328.0187753319985404 ) ) ;
#12279 = CARTESIAN_POINT ( 'NONE',  ( 764.8639956371174549, -128.0891481129655176, 319.7806653035542013 ) ) ;
#12280 = CARTESIAN_POINT ( 'NONE',  ( 759.8311093483677041, 25.83076734649409545, -310.9282345327691814 ) ) ;
#12282 = CARTESIAN_POINT ( 'NONE',  ( 768.0187753319979720, -272.6346026584196807, 318.0580252608186242 ) ) ;
#12281 = CARTESIAN_POINT ( 'NONE',  ( 781.7834795799800531, -250.8164208402379245, 315.0636971347436202 ) ) ;
#12283 = FACE_BOUND ( 'NONE', #4776, .T. ) ;
#12284 = EDGE_LOOP ( 'NONE', ( #39000, #7644, #37494, #10105 ) ) ;
#12285 = CARTESIAN_POINT ( 'NONE',  ( 797.6776695296629214, -451.5436935675099903, 357.6776695296636603 ) ) ;
#12286 = CARTESIAN_POINT ( 'NONE',  ( 795.8262568251477660, -262.3726999360617924, -308.3538107759623585 ) ) ;
#12287 = EDGE_CURVE ( 'NONE', #33219, #32511, #2701, .T. ) ;
#12288 = EDGE_LOOP ( 'NONE', ( #4769, #3761, #2153, #27457 ) ) ;
#12289 = VECTOR ( 'NONE', #3324, 1000.000000000000000 ) ;
#12290 = CARTESIAN_POINT ( 'NONE',  ( 814.2001403089898304, -233.3618753856925423, 347.4397851343538264 ) ) ;
#12291 = EDGE_CURVE ( 'NONE', #20106, #6763, #45431, .T. ) ;
#12292 = CARTESIAN_POINT ( 'NONE',  ( 769.9779781133707957, -307.0999726633343130, 316.7813123517150871 ) ) ;
#12293 = CARTESIAN_POINT ( 'NONE',  ( 765.8855110935204493, -382.1692326535045936, 319.0159684113471599 ) ) ;
#12294 = ORIENTED_EDGE ( 'NONE', *, *, #44450, .T. ) ;
#12296 = VECTOR ( 'NONE', #7833, 1000.000000000000000 ) ;
#12295 = CARTESIAN_POINT ( 'NONE',  ( 776.9254006560222479, -116.1908817542440033, -314.8983024940802125 ) ) ;
#12297 = CARTESIAN_POINT ( 'NONE',  ( 764.8639956371174549, -296.0891481129650629, -319.7806653035542581 ) ) ;
#12298 = VERTEX_POINT ( 'NONE', #23921 ) ;
#12299 = CARTESIAN_POINT ( 'NONE',  ( 794.9819416627830151, -420.9982390220555999, -319.9864689768909898 ) ) ;
#12300 = CARTESIAN_POINT ( 'NONE',  ( 755.0636971347428243, -100.2709662947838609, -341.7834795799807353 ) ) ;
#12301 = CARTESIAN_POINT ( 'NONE',  ( 793.2243759319678702, -266.5328690171413655, 318.4439275373583200 ) ) ;
#12302 = ADVANCED_FACE ( 'NONE', ( #32248 ), #36382, .F. ) ;
#12303 = CARTESIAN_POINT ( 'NONE',  ( 998.9999999999992042, 479.9999999999999432, 199.9999999999999716 ) ) ;
#12304 = DIRECTION ( 'NONE',  ( 1.000000000000000000, 0.000000000000000000, 0.000000000000000000 ) ) ;
#12305 = VECTOR ( 'NONE', #12189, 1000.000000000000000 ) ;
#12306 = EDGE_CURVE ( 'NONE', #5691, #40848, #15155, .T. ) ;
#12307 = CARTESIAN_POINT ( 'NONE',  ( 745.7194118038753459, -13.64542720878976390, -348.7631598425976449 ) ) ;
#12308 = CARTESIAN_POINT ( 'NONE',  ( 797.6776695296629214, 4.456306432488530866, 357.6776695296636603 ) ) ;
#12309 = EDGE_LOOP ( 'NONE', ( #26291, #25022, #42835, #19145 ) ) ;
#12310 = CARTESIAN_POINT ( 'NONE',  ( 815.3608509340175488, -314.7363362996979959, -341.2497674668889545 ) ) ;
#12311 = CARTESIAN_POINT ( 'NONE',  ( 754.3581564841646241, -209.4636090269709996, 316.1443688327762516 ) ) ;
#12313 = CARTESIAN_POINT ( 'NONE',  ( 804.6798772138708955, -279.7255117493288026, -334.6312213355107019 ) ) ;
#12312 = DIRECTION ( 'NONE',  ( -1.000000000000000000, -0.000000000000000000, -0.000000000000000000 ) ) ;
#12314 = DIRECTION ( 'NONE',  ( 1.000000000000000000, 0.000000000000000000, 0.000000000000000000 ) ) ;
#12315 = CARTESIAN_POINT ( 'NONE',  ( 786.5483106153019435, -151.6454272087892718, -364.1601925771022366 ) ) ;
#12316 = LINE ( 'NONE', #22912, #5506 ) ;
#12317 = CARTESIAN_POINT ( 'NONE',  ( 751.9810565676468741, -362.0891481129648923, -360.9747183278973921 ) ) ;
#12318 = DIRECTION ( 'NONE',  ( 0.000000000000000000, 0.000000000000000000, 1.000000000000000000 ) ) ;
#12319 = CARTESIAN_POINT ( 'NONE',  ( 797.6776695296629214, -43.54369356751131903, 357.6776695296636603 ) ) ;
#12320 = VECTOR ( 'NONE', #3686, 1000.000000000000000 ) ;
#12321 = CARTESIAN_POINT ( 'NONE',  ( 811.3240766477731540, -268.3726999360616787, 355.6651683502462902 ) ) ;
#12322 = EDGE_CURVE ( 'NONE', #30229, #41166, #21812, .T. ) ;
#12323 = CARTESIAN_POINT ( 'NONE',  ( 792.2312462859673587, -275.9073299311469896, 307.2067596250082602 ) ) ;
#12324 = CARTESIAN_POINT ( 'NONE',  ( 815.0009284576459549, -438.3510508353226669, -338.7629533639073429 ) ) ;
#12325 = VECTOR ( 'NONE', #22573, 1000.000000000000000 ) ;
#12326 = PLANE ( 'NONE',  #32808 ) ;
#12327 = DIRECTION ( 'NONE',  ( -1.000000000000000000, 0.000000000000000000, 0.000000000000000000 ) ) ;
#12328 = CARTESIAN_POINT ( 'NONE',  ( 803.4237431249931660, -351.1800572038740142, 331.2633955100225194 ) ) ;
#12329 = CARTESIAN_POINT ( 'NONE',  ( 796.9571628226829034, -119.4636090269712554, 321.2382568024804641 ) ) ;
#12330 = CARTESIAN_POINT ( 'NONE',  ( 793.2243759319678702, -26.53286901714210799, -318.4439275373583200 ) ) ;
#12331 = AXIS2_PLACEMENT_3D ( 'NONE', #37217, #26593, #9046 ) ;
#12332 = CARTESIAN_POINT ( 'NONE',  ( 441.1634899080286232, 256.4999999999999432, -199.9999999999972431 ) ) ;
#12333 = LINE ( 'NONE', #19704, #31411 ) ;
#12334 = CARTESIAN_POINT ( 'NONE',  ( 781.7834795799800531, -394.8164208402374697, 315.0636971347436202 ) ) ;
#12335 = ORIENTED_EDGE ( 'NONE', *, *, #32641, .T. ) ;
#12336 = VECTOR ( 'NONE', #21613, 1000.000000000000000 ) ;
#12337 = CARTESIAN_POINT ( 'NONE',  ( 794.1144889064781864, -346.1692326535047641, -360.9840315886528401 ) ) ;
#12338 = CARTESIAN_POINT ( 'NONE',  ( 788.8264449731200330, -165.1800572038745258, 363.6646147819171233 ) ) ;
#12339 = CARTESIAN_POINT ( 'NONE',  ( 744.9990715423526808, -330.3510508353229511, -341.2370466360926002 ) ) ;
#12340 = PLANE ( 'NONE',  #4265 ) ;
#12341 = ORIENTED_EDGE ( 'NONE', *, *, #38798, .F. ) ;
#12342 = CARTESIAN_POINT ( 'NONE',  ( 774.6858677611749044, -369.7255117493284615, 315.5713283507209894 ) ) ;
#12343 = ADVANCED_FACE ( 'NONE', ( #11008 ), #18397, .T. ) ;
#12344 = ORIENTED_EDGE ( 'NONE', *, *, #2430, .T. ) ;
#12345 = CARTESIAN_POINT ( 'NONE',  ( 787.5162901302840055, -179.3618753856927128, -305.4481719005792684 ) ) ;
#12346 = CARTESIAN_POINT ( 'NONE',  ( 808.3070685750232087, -66.99823902205670834, 361.1904061080339829 ) ) ;
#12347 = VERTEX_POINT ( 'NONE', #28784 ) ;
#12348 = CARTESIAN_POINT ( 'NONE',  ( 788.8264449731201466, -189.1800572038744690, -363.6646147819170665 ) ) ;
#12349 = ORIENTED_EDGE ( 'NONE', *, *, #8285, .T. ) ;
#12350 = CARTESIAN_POINT ( 'NONE',  ( 791.9812246680005501, 3.365397341579444479, -361.9419747391813189 ) ) ;
#12351 = CARTESIAN_POINT ( 'NONE',  ( 812.7932403749906598, -255.1800572038742700, 327.7687537140311633 ) ) ;
#12352 = CARTESIAN_POINT ( 'NONE',  ( 798.7617431975189675, -171.6237781080507432, 323.0428371773161871 ) ) ;
#12353 = EDGE_CURVE ( 'NONE', #16040, #17907, #4834, .T. ) ;
#12355 = DIRECTION ( 'NONE',  ( -1.000000000000000000, 0.000000000000000000, 0.000000000000000000 ) ) ;
#12354 = DIRECTION ( 'NONE',  ( -0.000000000000000000, 1.000000000000000000, -0.000000000000000000 ) ) ;
#12356 = VERTEX_POINT ( 'NONE', #35468 ) ;
#12357 = CARTESIAN_POINT ( 'NONE',  ( 784.1219089521767955, -429.2817908451521021, -315.0488828828318333 ) ) ;
#12358 = DIRECTION ( 'NONE',  ( 0.000000000000000000, 0.000000000000000000, 1.000000000000000000 ) ) ;
#12359 = ORIENTED_EDGE ( 'NONE', *, *, #15433, .T. ) ;
#12360 = CARTESIAN_POINT ( 'NONE',  ( 797.8822607201568644, -198.5545181178800647, -370.1134526219340160 ) ) ;
#12361 = CARTESIAN_POINT ( 'NONE',  ( 814.2805881961230625, -97.64542720878949922, 331.2368401574024119 ) ) ;
#12362 = AXIS2_PLACEMENT_3D ( 'NONE', #15127, #4501, #28984 ) ;
#12364 = CARTESIAN_POINT ( 'NONE',  ( 781.7834795799800531, -178.8164208402381519, -315.0636971347436202 ) ) ;
#12363 = DIRECTION ( 'NONE',  ( 0.000000000000000000, 0.000000000000000000, 1.000000000000000000 ) ) ;
#12365 = CARTESIAN_POINT ( 'NONE',  ( 783.0433043558608688, -360.8965053807773984, -315.1538015810313027 ) ) ;
#12366 = CARTESIAN_POINT ( 'NONE',  ( 521.6730038022808458, -9.808315785437627339E-14, 350.0000000000000000 ) ) ;
#12367 = CARTESIAN_POINT ( 'NONE',  ( 807.2620300519052989, -216.0090635724255037, -318.0141637701419768 ) ) ;
#12368 = DIRECTION ( 'NONE',  ( -0.000000000000000000, 0.6755902076156502511, 0.7372773368101330771 ) ) ;
#12369 = DIRECTION ( 'NONE',  ( -0.000000000000000000, -0.000000000000000000, 1.000000000000000000 ) ) ;
#12370 = CARTESIAN_POINT ( 'NONE',  ( 760.7433823573367135, -36.00906357242605793, -355.9930595647440441 ) ) ;
#12371 = CARTESIAN_POINT ( 'NONE',  ( 802.5472867521000353, -388.3726999360613945, 350.8726784830461156 ) ) ;
#12372 = CARTESIAN_POINT ( 'NONE',  ( 811.0346526505617248, -230.6346026584197944, -323.0537975583478101 ) ) ;
#12373 = DIRECTION ( 'NONE',  ( 0.000000000000000000, 0.000000000000000000, 1.000000000000000000 ) ) ;
#12374 = CARTESIAN_POINT ( 'NONE',  ( 791.7608162188021197, 240.0000000000000853, 360.0000000000000000 ) ) ;
#12375 = CARTESIAN_POINT ( 'NONE',  ( 803.4237431249931660, -39.18005720387496638, -331.2633955100225194 ) ) ;
#12376 = CARTESIAN_POINT ( 'NONE',  ( 811.3240766477731540, -196.3726999360619061, 355.6651683502462902 ) ) ;
#12377 = CARTESIAN_POINT ( 'NONE',  ( 815.1787889125755555, -126.8965053807781516, -343.7953271457877804 ) ) ;
#12378 = CARTESIAN_POINT ( 'NONE',  ( 808.0189434323515343, -158.0891481129655176, 319.0252816721025511 ) ) ;
#12379 = CARTESIAN_POINT ( 'NONE',  ( 751.6929314249748586, -390.9982390220557136, -318.8095938919659034 ) ) ;
#12380 = FACE_BOUND ( 'NONE', #27839, .T. ) ;
#12381 = CARTESIAN_POINT ( 'NONE',  ( 759.9864689768902508, -242.0891481129652618, 354.9819416627836404 ) ) ;
#12382 = CARTESIAN_POINT ( 'NONE',  ( 755.3028492785439312, -15.28179084515340058, 335.9200461376539693 ) ) ;
#12383 = CARTESIAN_POINT ( 'NONE',  ( 801.9419747391806368, -402.4527844766010389, -351.9812246680014027 ) ) ;
#12384 = DIRECTION ( 'NONE',  ( 0.000000000000000000, 0.000000000000000000, -1.000000000000000000 ) ) ;
#12385 = CARTESIAN_POINT ( 'NONE',  ( 747.6481478633932056, -13.09997266333522248, -353.4146539503763620 ) ) ;
#12386 = CARTESIAN_POINT ( 'NONE',  ( 187.1337867209877857, 56.78581973499402835, -212.6378164459127049 ) ) ;
#12387 = CARTESIAN_POINT ( 'NONE',  ( 773.3843516231979720, -85.44195992623282621, 364.4086373105754433 ) ) ;
#12388 = EDGE_LOOP ( 'NONE', ( #6316, #12613, #26870, #29525 ) ) ;
#12389 = CARTESIAN_POINT ( 'NONE',  ( 800.7704444035546203, -220.1692326535051052, -326.0291762391768771 ) ) ;
#12390 = CARTESIAN_POINT ( 'NONE',  ( 771.2633955100217236, -71.90732993114760063, 363.4237431249939618 ) ) ;
#12391 = CARTESIAN_POINT ( 'NONE',  ( 745.1769319972822814, -233.8055962898687028, -346.2694204179732083 ) ) ;
#12392 = FILL_AREA_STYLE_COLOUR ( '', #18697 ) ;
#12393 = CARTESIAN_POINT ( 'NONE',  ( 744.9990715423526808, -330.3510508353229511, 341.2370466360926002 ) ) ;
#12394 = ORIENTED_EDGE ( 'NONE', *, *, #11458, .F. ) ;
#12395 = CARTESIAN_POINT ( 'NONE',  ( 783.7566961878529810, -432.8965053807771142, 305.1792804349288417 ) ) ;
#12396 = CARTESIAN_POINT ( 'NONE',  ( 768.0187753319979720, -368.6346026584193964, 318.0580252608186242 ) ) ;
#12397 = CARTESIAN_POINT ( 'NONE',  ( 814.2001403089898304, -89.36187538569299704, -347.4397851343538264 ) ) ;
#12398 = CARTESIAN_POINT ( 'NONE',  ( 762.3223304703356007, -55.54369356751127640, -322.3223304703362828 ) ) ;
#12399 = VERTEX_POINT ( 'NONE', #7539 ) ;
#12400 = CARTESIAN_POINT ( 'NONE',  ( 804.8461984189677878, -2.190881754244347945, -336.9566956441385628 ) ) ;
#12401 = ORIENTED_EDGE ( 'NONE', *, *, #31257, .F. ) ;
#12402 = CARTESIAN_POINT ( 'NONE',  ( 790.9844846989617508, -334.3726999360615082, -317.2208543904092721 ) ) ;
#12404 = CARTESIAN_POINT ( 'NONE',  ( 786.5483106153019435, -415.6454272087885897, 364.1601925771022366 ) ) ;
#12403 = CARTESIAN_POINT ( 'NONE',  ( 774.6858677611749044, -81.72551174932937101, 315.5713283507209894 ) ) ;
#12407 = CARTESIAN_POINT ( 'NONE',  ( 746.7653713866222915, -305.2601417444139429, 351.0478386215610271 ) ) ;
#12406 = DIRECTION ( 'NONE',  ( 1.880165489482579047E-16, 1.000000000000000000, -0.000000000000000000 ) ) ;
#12405 = CARTESIAN_POINT ( 'NONE',  ( 767.6429770376291799, -441.1800572038736163, 306.8695393053162093 ) ) ;
#12408 = CARTESIAN_POINT ( 'NONE',  ( 766.5853460496234675, -109.9874144716873019, 372.3518521366060554 ) ) ;
#12409 = CARTESIAN_POINT ( 'NONE',  ( 801.5560724626406000, -312.5545181178797520, -326.7756240680316182 ) ) ;
#12410 = CARTESIAN_POINT ( 'NONE',  ( 765.0180583372156207, -312.9982390220559409, -360.0135310231089534 ) ) ;
#12411 = CARTESIAN_POINT ( 'NONE',  ( 785.3687786644884454, -155.3618753856927128, -315.3201227861279676 ) ) ;
#12412 = CARTESIAN_POINT ( 'NONE',  ( 749.2812353651451076, -438.4527844766009821, 323.2262854647983090 ) ) ;
#12414 = CARTESIAN_POINT ( 'NONE',  ( -879.9999999999992042, 579.9999999999998863, -360.0000000000000000 ) ) ;
#12413 = FACE_OUTER_BOUND ( 'NONE', #9958, .T. ) ;
#12415 = CARTESIAN_POINT ( 'NONE',  ( 752.7379699480933368, -132.0090635724257595, -361.9858362298580232 ) ) ;
#12416 = DIRECTION ( 'NONE',  ( -0.000000000000000000, -0.000000000000000000, 1.000000000000000000 ) ) ;
#12417 = LINE ( 'NONE', #5249, #31882 ) ;
#12418 = CARTESIAN_POINT ( 'NONE',  ( 755.8894580844503253, -303.8272453906071178, 332.3691319403863531 ) ) ;
#12419 = EDGE_LOOP ( 'NONE', ( #26629, #7700, #39977, #33907, #33198, #9491 ) ) ;
#12420 = CARTESIAN_POINT ( 'NONE',  ( 754.3581564841646241, -281.4636090269706870, 316.1443688327762516 ) ) ;
#12421 = CARTESIAN_POINT ( 'NONE',  ( 805.0032342141413437, -133.5436935675110419, -314.9967657858572352 ) ) ;
#12422 = CARTESIAN_POINT ( 'NONE',  ( 190.7583438952258916, 294.6698570112193920, -274.9999999999999432 ) ) ;
#12423 = VECTOR ( 'NONE', #42662, 1000.000000000000000 ) ;
#12424 = CARTESIAN_POINT ( 'NONE',  ( 793.5525998758768083, -79.09997266333503774, 372.6845335610516941 ) ) ;
#12425 = CARTESIAN_POINT ( 'NONE',  ( 808.3070685750230950, -258.9982390220561115, -361.1904061080339261 ) ) ;
#12426 = CARTESIAN_POINT ( 'NONE',  ( 758.8095938919644823, -440.0891481129645513, -311.6929314249762797 ) ) ;
#12427 = CARTESIAN_POINT ( 'NONE',  ( 768.0187753319979720, -152.6346026584200786, 318.0580252608186242 ) ) ;
#12428 = ORIENTED_EDGE ( 'NONE', *, *, #43078, .T. ) ;
#12429 = CARTESIAN_POINT ( 'NONE',  ( 781.2497674668890113, -348.3510508353228943, -375.3608509340180603 ) ) ;
#12430 = CARTESIAN_POINT ( 'NONE',  ( 814.9108240113580450, -88.27096629478390355, -337.5031285880265273 ) ) ;
#12431 = CARTESIAN_POINT ( 'NONE',  ( 799.2566176426618085, -24.00906357242609346, 324.0069404352559559 ) ) ;
#12432 = CARTESIAN_POINT ( 'NONE',  ( 767.7687537140311633, -335.9073299311468190, -372.7932403749916830 ) ) ;
#12433 = CARTESIAN_POINT ( 'NONE',  ( 759.9999999999992042, -512.9681489794448908, -350.0000000000000000 ) ) ;
#12434 = CARTESIAN_POINT ( 'NONE',  ( 776.9566956441375396, -396.8965053807772847, 364.8461984189686405 ) ) ;
#12435 = VERTEX_POINT ( 'NONE', #29462 ) ;
#12436 = CARTESIAN_POINT ( 'NONE',  ( 781.8018195045266339, -214.2709662947834488, -365.1927285166406705 ) ) ;
#12437 = CARTESIAN_POINT ( 'NONE',  ( 754.0944755984390895, -135.6237781080508853, -364.1009440267246760 ) ) ;
#12438 = CARTESIAN_POINT ( 'NONE',  ( 799.9999999999993179, -365.3551492539851893, -28.13243251470704109 ) ) ;
#12439 = CARTESIAN_POINT ( 'NONE',  ( 749.8865473780648472, -236.5328690171414792, 322.1177392798429082 ) ) ;
#12440 = CARTESIAN_POINT ( 'NONE',  ( 781.7834795799800531, -82.81642084023846451, 315.0636971347436202 ) ) ;
#12441 = ORIENTED_EDGE ( 'NONE', *, *, #14012, .T. ) ;
#12442 = ORIENTED_EDGE ( 'NONE', *, *, #9964, .T. ) ;
#12443 = CARTESIAN_POINT ( 'NONE',  ( 773.3843516231979720, -13.44195992623305713, -364.4086373105754433 ) ) ;
#12444 = CARTESIAN_POINT ( 'NONE',  ( 755.5713283507202505, -245.3618753856925139, 334.6858677611754729 ) ) ;
#12445 = CARTESIAN_POINT ( 'NONE',  ( 758.8095938919642549, 15.91085188703394238, -311.6929314249763365 ) ) ;
#12446 = CARTESIAN_POINT ( 'NONE',  ( -462.7175100919714055, 256.5000000000001705, -199.9999999999908766 ) ) ;
#12447 = VERTEX_POINT ( 'NONE', #25973 ) ;
#12448 = ORIENTED_EDGE ( 'NONE', *, *, #33669, .F. ) ;
#12449 = CARTESIAN_POINT ( 'NONE',  ( 810.4231160770870019, -384.5545181178795247, -321.9338519418446936 ) ) ;
#12450 = VECTOR ( 'NONE', #43768, 1000.000000000000000 ) ;
#12451 = CARTESIAN_POINT ( 'NONE',  ( 803.6646147819161570, -233.9073299311470180, -348.8264449731210561 ) ) ;
#12452 = CARTESIAN_POINT ( 'NONE',  ( 749.2812353651451076, -342.4527844766013231, 323.2262854647983090 ) ) ;
#12453 = CARTESIAN_POINT ( 'NONE',  ( 783.7566961878529810, -48.89650538077840025, 305.1792804349288417 ) ) ;
#12454 = CARTESIAN_POINT ( 'NONE',  ( 755.8894580844503253, -231.8272453906072315, -332.3691319403863531 ) ) ;
#12455 = CARTESIAN_POINT ( 'NONE',  ( 803.4237431249931660, -207.1800572038744406, -331.2633955100225194 ) ) ;
#12456 = CARTESIAN_POINT ( 'NONE',  ( 801.9419747391806368, -378.4527844766011526, -351.9812246680014027 ) ) ;
#12457 = ORIENTED_EDGE ( 'NONE', *, *, #16521, .T. ) ;
#12458 = CARTESIAN_POINT ( 'NONE',  ( 759.7806653035534055, -198.9982390220562252, 324.8639956371180801 ) ) ;
#12459 = CARTESIAN_POINT ( 'NONE',  ( 792.1044303154645831, -108.4527844766019911, -317.8323909638837677 ) ) ;
#12460 = VERTEX_POINT ( 'NONE', #17933 ) ;
#12461 = CARTESIAN_POINT ( 'NONE',  ( 814.2001403089898304, -329.3618753856922581, 347.4397851343538264 ) ) ;
#12462 = CARTESIAN_POINT ( 'NONE',  ( 989.9999999999992042, -590.0000000000001137, -209.9999999999999716 ) ) ;
#12463 = CARTESIAN_POINT ( 'NONE',  ( 879.9999999999992042, 579.9999999999998863, -360.0000000000000000 ) ) ;
#12464 = DIRECTION ( 'NONE',  ( 0.000000000000000000, 0.000000000000000000, 1.000000000000000000 ) ) ;
#12465 = CARTESIAN_POINT ( 'NONE',  ( 755.5913626894240451, -205.6454272087891297, 346.6156483768012890 ) ) ;
#12466 = CARTESIAN_POINT ( 'NONE',  ( 754.8072714833581358, -76.81642084023845030, 338.1981804954720587 ) ) ;
#12467 = ORIENTED_EDGE ( 'NONE', *, *, #37644, .F. ) ;
#12468 = CARTESIAN_POINT ( 'NONE',  ( 795.8262568251477660, -454.3726999360611103, -308.3538107759623585 ) ) ;
#12469 = CARTESIAN_POINT ( 'NONE',  ( 808.0189434323515343, -38.08914811296587999, -319.0252816721025511 ) ) ;
#12470 = CARTESIAN_POINT ( 'NONE',  ( 793.2243759319678702, -266.5328690171413655, 318.4439275373583200 ) ) ;
#12471 = CARTESIAN_POINT ( 'NONE',  ( 771.2633955100217236, -383.9073299311466485, -363.4237431249939618 ) ) ;
#12472 = CARTESIAN_POINT ( 'NONE',  ( 758.0580252608178853, -6.452784476602343666, -328.0187753319985404 ) ) ;
#12473 = CARTESIAN_POINT ( 'NONE',  ( 792.2312462859673587, -443.9073299311464780, 307.2067596250082602 ) ) ;
#12474 = CARTESIAN_POINT ( 'NONE',  ( 355.8971257818259915, 290.0000000000001137, -244.9999999999999716 ) ) ;
#12475 = CARTESIAN_POINT ( 'NONE',  ( 759.0159684113467620, -280.9181544815162965, -325.8855110935213020 ) ) ;
#12476 = CARTESIAN_POINT ( 'NONE',  ( 811.0346526505616112, -158.6346026584199933, -323.0537975583477532 ) ) ;
#12477 = CARTESIAN_POINT ( 'NONE',  ( 782.5225473063381969, -94.27096629478386092, 375.2698199232970637 ) ) ;
#12478 = CARTESIAN_POINT ( 'NONE',  ( 796.9462024416508257, -132.4527844766018916, 308.9653473494370246 ) ) ;
#12479 = CARTESIAN_POINT ( 'NONE',  ( 785.1593951492109227, 16.45630643248848912, -313.8313994339321766 ) ) ;
#12480 = DIRECTION ( 'NONE',  ( -0.000000000000000000, 1.000000000000000000, -0.000000000000000000 ) ) ;
#12481 = AXIS2_PLACEMENT_3D ( 'NONE', #10854, #38344, #24235 ) ;
#12482 = LINE ( 'NONE', #16172, #39046 ) ;
#12483 = CARTESIAN_POINT ( 'NONE',  ( 767.7687537140311633, -359.9073299311467053, 372.7932403749916830 ) ) ;
#12484 = CARTESIAN_POINT ( 'NONE',  ( 755.0636971347428243, -364.2709662947830793, -341.7834795799807353 ) ) ;
#12485 = EDGE_CURVE ( 'NONE', #19801, #13016, #13709, .T. ) ;
#12486 = CARTESIAN_POINT ( 'NONE',  ( 805.1927285166397041, -448.8164208402371855, 341.8018195045277707 ) ) ;
#12487 = CARTESIAN_POINT ( 'NONE',  ( 797.8822607201568644, -102.5545181178804057, -370.1134526219340160 ) ) ;
#12488 = CARTESIAN_POINT ( 'NONE',  ( 803.2186876482843445, -103.9874144716873161, -350.0220218866286928 ) ) ;
#12489 = CARTESIAN_POINT ( 'NONE',  ( 773.7943932421234194, -119.8055962898690865, 305.5313806188329409 ) ) ;
#12490 = CYLINDRICAL_SURFACE ( 'NONE', #34328, 10.00000000000000888 ) ;
#12491 = CARTESIAN_POINT ( 'NONE',  ( 788.8264449731200330, -21.18005720387502677, -363.6646147819171233 ) ) ;
#12492 = CARTESIAN_POINT ( 'NONE',  ( 764.0069404352550464, -135.0783235625962959, -359.2566176426627180 ) ) ;
#12493 = CARTESIAN_POINT ( 'NONE',  ( 755.5713283507202505, -125.3618753856928834, -334.6858677611754729 ) ) ;
#12494 = CARTESIAN_POINT ( 'NONE',  ( 771.2633955100217236, -143.9073299311473590, 363.4237431249939618 ) ) ;
#12495 = ADVANCED_FACE ( 'NONE', ( #827 ), #45437, .F. ) ;
#12496 = CARTESIAN_POINT ( 'NONE',  ( 790.8726784830453198, -418.7146871989590409, -362.5472867521010585 ) ) ;
#12498 = CARTESIAN_POINT ( 'NONE',  ( 778.1981804954715471, -274.2709662947832499, 314.8072714833591021 ) ) ;
#12497 = CARTESIAN_POINT ( 'NONE',  ( 765.0180583372156207, -288.9982390220559978, 360.0135310231089534 ) ) ;
#12499 = DIRECTION ( 'NONE',  ( -1.000000000000000000, 0.000000000000000000, 0.000000000000000000 ) ) ;
#12500 = ORIENTED_EDGE ( 'NONE', *, *, #10302, .F. ) ;
#12501 = CARTESIAN_POINT ( 'NONE',  ( 794.9819416627830151, -444.9982390220554862, 319.9864689768909898 ) ) ;
#12502 = CARTESIAN_POINT ( 'NONE',  ( 809.0717654672305343, -268.9181544815162397, -360.1688906516309885 ) ) ;
#12503 = ORIENTED_EDGE ( 'NONE', *, *, #17293, .T. ) ;
#12504 = CARTESIAN_POINT ( 'NONE',  ( 0.000000000000000000, 0.000000000000000000, 0.000000000000000000 ) ) ;
#12505 = CARTESIAN_POINT ( 'NONE',  ( 796.9462024416508257, -204.4527844766016926, 308.9653473494370246 ) ) ;
#12506 = CARTESIAN_POINT ( 'NONE',  ( 802.9823548866075953, -313.0999726633342561, 330.0799878456151077 ) ) ;
#12507 = CARTESIAN_POINT ( 'NONE',  ( 804.1601925771018387, -391.4419599262317888, 346.5483106153029098 ) ) ;
#12508 = ORIENTED_EDGE ( 'NONE', *, *, #31927, .F. ) ;
#12509 = CARTESIAN_POINT ( 'NONE',  ( 766.0291762391763086, -130.9181544815166660, -360.7704444035551319 ) ) ;
#12510 = CARTESIAN_POINT ( 'NONE',  ( 800.0135310231082713, -110.0891481129656597, -325.0180583372163028 ) ) ;
#12511 = CARTESIAN_POINT ( 'NONE',  ( 762.1405469898973024, -289.5436935675105019, -357.8594530101016176 ) ) ;
#12512 = ORIENTED_EDGE ( 'NONE', *, *, #41538, .T. ) ;
#12513 = VECTOR ( 'NONE', #38424, 1000.000000000000000 ) ;
#12514 = CARTESIAN_POINT ( 'NONE',  ( 754.8072714833581358, -412.8164208402372992, -338.1981804954720587 ) ) ;
#12515 = CARTESIAN_POINT ( 'NONE',  ( 755.0636971347428243, -76.27096629478394618, -341.7834795799807353 ) ) ;
#12516 = EDGE_CURVE ( 'NONE', #36107, #25758, #25302, .T. ) ;
#12517 = CARTESIAN_POINT ( 'NONE',  ( 803.8651313633788504, -317.2601417444139429, 332.4468031744301015 ) ) ;
#12518 = FACE_OUTER_BOUND ( 'NONE', #11253, .T. ) ;
#12519 = CARTESIAN_POINT ( 'NONE',  ( 794.9999999999993179, 212.6707680665973612, 236.5295014342203785 ) ) ;
#12520 = DIRECTION ( 'NONE',  ( 1.000000000000000000, -1.892425610156518354E-16, 0.000000000000000000 ) ) ;
#12521 = EDGE_LOOP ( 'NONE', ( #9544, #26284 ) ) ;
#12522 = CARTESIAN_POINT ( 'NONE',  ( 762.1177392798416577, -354.5545181178796383, -309.8865473780659272 ) ) ;
#12523 = CARTESIAN_POINT ( 'NONE',  ( 786.2694204179717872, -213.2817908451527842, 305.1769319972829067 ) ) ;
#12525 = CARTESIAN_POINT ( 'NONE',  ( 804.4286716492782716, -281.3618753856923718, -345.3141322388244703 ) ) ;
#12524 = CARTESIAN_POINT ( 'NONE',  ( 51.16348990802859475, 258.0940000000000509, -193.8809999999945433 ) ) ;
#12526 = CARTESIAN_POINT ( 'NONE',  ( -858.8365100919713768, 260.0000000000002274, -199.9999999999881481 ) ) ;
#12527 = CARTESIAN_POINT ( 'NONE',  ( 763.8424801807145741, -186.0090635724255890, -320.5453621957614700 ) ) ;
#12528 =( REPRESENTATION_RELATIONSHIP ('NONE','NONE', #39835, #15645 ) REPRESENTATION_RELATIONSHIP_WITH_TRANSFORMATION ( #35285 )SHAPE_REPRESENTATION_RELATIONSHIP( ) );
#12529 = CARTESIAN_POINT ( 'NONE',  ( 749.2812353651451076, -30.45278447660226817, 323.2262854647983090 ) ) ;
#12530 = DIRECTION ( 'NONE',  ( -1.000000000000000000, -0.000000000000000000, -0.000000000000000000 ) ) ;
#12531 = CARTESIAN_POINT ( 'NONE',  ( 800.9747183278959710, -372.9982390220557704, -311.9810565676471583 ) ) ;
#12532 = CARTESIAN_POINT ( 'NONE',  ( 764.8639956371174549, -56.08914811296580893, 319.7806653035542013 ) ) ;
#12533 = EDGE_CURVE ( 'NONE', #37578, #41429, #39577, .T. ) ;
#12534 = CARTESIAN_POINT ( 'NONE',  ( 795.8262568251477660, -310.3726999360616219, 308.3538107759623585 ) ) ;
#12535 = CARTESIAN_POINT ( 'NONE',  ( 808.3070685750230950, -258.9982390220561115, 361.1904061080339261 ) ) ;
#12536 = CARTESIAN_POINT ( 'NONE',  ( 751.6929314249748586, -30.99823902205680071, -318.8095938919659034 ) ) ;
#12537 = CARTESIAN_POINT ( 'NONE',  ( 788.8264449731200330, -261.1800572038741848, -363.6646147819171233 ) ) ;
#12538 = EDGE_CURVE ( 'NONE', #9209, #9555, #40081, .T. ) ;
#12539 = CARTESIAN_POINT ( 'NONE',  ( -959.5497976682736407, 240.0000000000002274, -209.9999999999999716 ) ) ;
#12540 = CARTESIAN_POINT ( 'NONE',  ( 755.5713283507202505, -365.3618753856920875, 334.6858677611754729 ) ) ;
#12541 = CARTESIAN_POINT ( 'NONE',  ( 757.0176451133909268, -133.0999726633348246, 349.9200121543848354 ) ) ;
#12542 = CARTESIAN_POINT ( 'NONE',  ( 780.5290396650775619, -12.35105083532396897, -365.2837595273619513 ) ) ;
#12543 = CARTESIAN_POINT ( 'NONE',  ( 779.9911637788978851, -452.9681489794448339, -340.0036600600989232 ) ) ;
#12544 = DIRECTION ( 'NONE',  ( -0.000000000000000000, -0.000000000000000000, -1.000000000000000000 ) ) ;
#12545 = CARTESIAN_POINT ( 'NONE',  ( 755.3201227861273992, -411.7255117493282910, 345.3687786644892981 ) ) ;
#12546 = ORIENTED_EDGE ( 'NONE', *, *, #36083, .F. ) ;
#12547 = EDGE_CURVE ( 'NONE', #42970, #27381, #22286, .T. ) ;
#12548 = CARTESIAN_POINT ( 'NONE',  ( 780.5290396650775619, -324.3510508353229511, -365.2837595273619513 ) ) ;
#12550 = CARTESIAN_POINT ( 'NONE',  ( 800.0135310231082713, -158.0891481129655176, 325.0180583372163028 ) ) ;
#12549 = CARTESIAN_POINT ( 'NONE',  ( 774.6858677611749044, -201.7255117493290015, 315.5713283507209894 ) ) ;
#12551 = PRODUCT_DEFINITION_CONTEXT ( 'detailed design', #36407, 'design' ) ;
#12552 = CARTESIAN_POINT ( 'NONE',  ( 751.2241431872005251, -352.1692326535046504, -359.9636004259367610 ) ) ;
#12553 = CARTESIAN_POINT ( 'NONE',  ( -786.4999999999993179, -513.1383975375929367, -369.9999999999999432 ) ) ;
#12554 = ORIENTED_EDGE ( 'NONE', *, *, #5197, .F. ) ;
#12555 = CARTESIAN_POINT ( 'NONE',  ( 762.1405469898971887, -361.5436935675103882, 357.8594530101015607 ) ) ;
#12556 = VERTEX_POINT ( 'NONE', #43092 ) ;
#12557 = CARTESIAN_POINT ( 'NONE',  ( 775.4999999999993179, -512.9681489794448908, -352.0000000000000000 ) ) ;
#12558 = CARTESIAN_POINT ( 'NONE',  ( 792.3570229623688874, -189.1800572038744122, -373.1304606946836202 ) ) ;
#12559 = CARTESIAN_POINT ( 'NONE',  ( 758.8095938919644823, -104.0891481129656739, 311.6929314249762797 ) ) ;
#12560 = VERTEX_POINT ( 'NONE', #18172 ) ;
#12561 = CARTESIAN_POINT ( 'NONE',  ( 771.2633955100217236, -167.9073299311473022, -363.4237431249939618 ) ) ;
#12562 = VERTEX_POINT ( 'NONE', #42862 ) ;
#12563 = EDGE_CURVE ( 'NONE', #27073, #45131, #36588, .T. ) ;
#12564 = CARTESIAN_POINT ( 'NONE',  ( 793.0897708529556667, -462.5545181178792973, -361.3366627262616362 ) ) ;
#12565 = ADVANCED_FACE ( 'NONE', ( #43323 ), #37336, .F. ) ;
#12566 = CARTESIAN_POINT ( 'NONE',  ( 747.2067596250078623, -267.1800572038742985, 352.2312462859687230 ) ) ;
#12567 = CARTESIAN_POINT ( 'NONE',  ( 784.0799538623451781, -179.8055962898688733, 364.6971507214555572 ) ) ;
#12569 = FACE_OUTER_BOUND ( 'NONE', #14340, .T. ) ;
#12568 = CARTESIAN_POINT ( 'NONE',  ( 999.9999999999992042, -600.0000000000001137, 360.0000000000000000 ) ) ;
#12570 = ORIENTED_EDGE ( 'NONE', *, *, #25566, .F. ) ;
#12571 = CARTESIAN_POINT ( 'NONE',  ( 796.9571628226829034, -431.4636090269702322, -321.2382568024804641 ) ) ;
#12572 = DIRECTION ( 'NONE',  ( -0.000000000000000000, 1.000000000000000000, -0.000000000000000000 ) ) ;
#12573 = CARTESIAN_POINT ( 'NONE',  ( 786.2694204179717872, -237.2817908451526421, -305.1769319972829067 ) ) ;
#12574 = CARTESIAN_POINT ( 'NONE',  ( 804.1009440267234822, -119.4636090269712554, 314.0944755984392600 ) ) ;
#12576 = CARTESIAN_POINT ( 'NONE',  ( 804.4286716492782716, -185.3618753856926844, -345.3141322388244703 ) ) ;
#12575 = LINE ( 'NONE', #26879, #41120 ) ;
#12577 = CARTESIAN_POINT ( 'NONE',  ( 757.2208543904082489, -352.7146871989593251, -350.9844846989624330 ) ) ;
#12578 = CARTESIAN_POINT ( 'NONE',  ( 939.9999999999993179, -416.7569064942979935, 212.5753187112032947 ) ) ;
#12579 = CARTESIAN_POINT ( 'NONE',  ( 786.2694204179717872, -237.2817908451526421, -305.1769319972829067 ) ) ;
#12580 = CARTESIAN_POINT ( 'NONE',  ( 772.4999999999993179, -512.9681489794448908, -309.9999999999998863 ) ) ;
#12581 = CARTESIAN_POINT ( 'NONE',  ( 779.9999999999992042, -452.9681489794448339, -329.9999999999999432 ) ) ;
#12582 = CARTESIAN_POINT ( 'NONE',  ( 796.1575198192839480, -30.00906357242607925, -359.4546378042384163 ) ) ;
#12583 = CARTESIAN_POINT ( 'NONE',  ( 760.7433823573367135, -444.0090635724249069, 355.9930595647440441 ) ) ;
#12584 = CARTESIAN_POINT ( 'NONE',  ( 803.8651313633788504, -437.2601417444135450, -332.4468031744301015 ) ) ;
#12585 = CARTESIAN_POINT ( 'NONE',  ( 814.9108240113580450, -280.2709662947833067, -337.5031285880265273 ) ) ;
#12586 = CARTESIAN_POINT ( 'NONE',  ( 783.0745993439762742, -248.1908817542435202, 365.1016975059196739 ) ) ;
#12587 = EDGE_CURVE ( 'NONE', #44896, #31811, #18848, .T. ) ;
#12588 = LINE ( 'NONE', #22966, #37250 ) ;
#12589 = DIRECTION ( 'NONE',  ( 1.000000000000000000, -0.000000000000000000, 0.000000000000000000 ) ) ;
#12590 = CARTESIAN_POINT ( 'NONE',  ( 762.3223304703356007, -55.54369356751127640, -322.3223304703362828 ) ) ;
#12591 = EDGE_CURVE ( 'NONE', #32411, #45239, #21089, .T. ) ;
#12592 = CARTESIAN_POINT ( 'NONE',  ( 773.7305795820266212, -225.2817908451527273, 374.8230680027170365 ) ) ;
#12593 = CARTESIAN_POINT ( 'NONE',  ( 768.8385539511368734, -119.2601417444145397, -306.4236121716840557 ) ) ;
#12594 = CARTESIAN_POINT ( 'NONE',  ( 808.3070685750230950, -162.9982390220563673, 361.1904061080339261 ) ) ;
#12595 = CARTESIAN_POINT ( 'NONE',  ( 810.7187646348534145, -402.4527844766010389, -356.7737145352016341 ) ) ;
#12596 = DIRECTION ( 'NONE',  ( 8.659560562354900811E-17, 0.7071067811865501263, -0.7071067811865449082 ) ) ;
#12597 = ADVANCED_FACE ( 'NONE', ( #18616, #32938 ), #43535, .F. ) ;
#12598 = CARTESIAN_POINT ( 'NONE',  ( 802.1676090361156639, -254.6346026584196238, 327.8955696845344505 ) ) ;
#12599 = CARTESIAN_POINT ( 'NONE',  ( 783.0745993439762742, -8.190881754244330182, 365.1016975059196739 ) ) ;
#12600 = CARTESIAN_POINT ( 'NONE',  ( 788.7366044899766848, -395.9073299311465348, -316.5762568750059813 ) ) ;
#12601 = CARTESIAN_POINT ( 'NONE',  ( 779.9999999999992042, 166.4563064324884465, 350.0000000000000000 ) ) ;
#12602 = CARTESIAN_POINT ( 'NONE',  ( 757.7880784355613741, -42.00906357242603661, -312.4576283171834916 ) ) ;
#12603 = CARTESIAN_POINT ( 'NONE',  ( -208.8365100919714052, 260.0000000000001137, -208.0249999999927013 ) ) ;
#12605 = CARTESIAN_POINT ( 'NONE',  ( 797.6776695296629214, -307.5436935675104451, 357.6776695296636603 ) ) ;
#12604 = CARTESIAN_POINT ( 'NONE',  ( 786.6156483768007774, -97.44195992623281199, 315.5913626894246136 ) ) ;
#12606 = ORIENTED_EDGE ( 'NONE', *, *, #21615, .T. ) ;
#12607 = EDGE_CURVE ( 'NONE', #42944, #10806, #11897, .T. ) ;
#12608 = CARTESIAN_POINT ( 'NONE',  ( 755.8398074228967971, -235.4419599262323857, -333.4516893846970333 ) ) ;
#12609 = CARTESIAN_POINT ( 'NONE',  ( 758.0580252608178853, -126.4527844766019626, -328.0187753319985404 ) ) ;
#12610 = CARTESIAN_POINT ( 'NONE',  ( 755.0636971347428243, -52.27096629478401724, 341.7834795799807353 ) ) ;
#12611 = CARTESIAN_POINT ( 'NONE',  ( 752.4576283171824116, -237.0783235625960117, -317.7880784355627952 ) ) ;
#12612 = CARTESIAN_POINT ( 'NONE',  ( 815.0009284576459549, -390.3510508353227237, 338.7629533639073429 ) ) ;
#12613 = ORIENTED_EDGE ( 'NONE', *, *, #21855, .T. ) ;
#12614 = CARTESIAN_POINT ( 'NONE',  ( 745.0891759886404770, -4.270966294784170003, 342.4968714119734159 ) ) ;
#12615 = CARTESIAN_POINT ( 'NONE',  ( 762.3223304703356007, -175.5436935675108998, -322.3223304703362828 ) ) ;
#12616 = CARTESIAN_POINT ( 'NONE',  ( 774.6312213355099630, -383.3618753856921444, 364.6798772138717482 ) ) ;
#12617 = CARTESIAN_POINT ( 'NONE',  ( 758.8095938919642549, -80.08914811296574499, -311.6929314249763365 ) ) ;
#12618 = CARTESIAN_POINT ( 'NONE',  ( 756.5762568750052424, -75.18005720387485269, -348.7366044899774238 ) ) ;
#12619 = ORIENTED_EDGE ( 'NONE', *, *, #22408, .F. ) ;
#12620 = CARTESIAN_POINT ( 'NONE',  ( 783.0745993439762742, -8.190881754244330182, -365.1016975059196739 ) ) ;
#12621 = ORIENTED_EDGE ( 'NONE', *, *, #1578, .T. ) ;
#12622 = CARTESIAN_POINT ( 'NONE',  ( 760.7433823573367135, -348.0090635724251342, -355.9930595647440441 ) ) ;
#12624 = CARTESIAN_POINT ( 'NONE',  ( 766.9102291470427417, -402.5545181178795247, 318.6633372737382501 ) ) ;
#12623 = CARTESIAN_POINT ( 'NONE',  ( 755.5713283507202505, -77.36187538569302546, 334.6858677611754729 ) ) ;
#12627 = CARTESIAN_POINT ( 'NONE',  ( 801.9858362298568863, -339.0783235625956422, 312.7379699480935642 ) ) ;
#12626 = CARTESIAN_POINT ( 'NONE',  ( 919.9999999999993179, 154.9999999999998863, 360.0000000000000000 ) ) ;
#12625 = CARTESIAN_POINT ( 'NONE',  ( 792.3570229623691148, -429.1800572038737300, 373.1304606946836770 ) ) ;
#12628 = CARTESIAN_POINT ( 'NONE',  ( 802.5472867521000353, -340.3726999360615082, -350.8726784830461156 ) ) ;
#12629 = CARTESIAN_POINT ( 'NONE',  ( 778.1981804954714335, -322.2709662947830225, -314.8072714833589885 ) ) ;
#12630 = CARTESIAN_POINT ( 'NONE',  ( 778.2165204200184689, -166.8164208402382087, -364.9363028652563230 ) ) ;
#12631 = CARTESIAN_POINT ( 'NONE',  ( 814.2001403089898304, -449.3618753856918602, 347.4397851343538264 ) ) ;
#12633 = DIRECTION ( 'NONE',  ( 0.000000000000000000, -1.000000000000000000, 0.000000000000000000 ) ) ;
#12632 = DIRECTION ( 'NONE',  ( -0.7014439490181307857, 0.1263042864341424876, 0.7014439490181749726 ) ) ;
#12634 = CARTESIAN_POINT ( 'NONE',  ( 773.3843516231979720, -277.4419599262322436, -364.4086373105754433 ) ) ;
#12635 = CARTESIAN_POINT ( 'NONE',  ( 749.5768839229115201, -132.5545181178802920, -358.0661480581553064 ) ) ;
#12636 = CARTESIAN_POINT ( 'NONE',  ( -28.63011601220122415, -359.5698779088871788, -26.28906389436296109 ) ) ;
#12637 = LINE ( 'NONE', #44749, #9768 ) ;
#12638 = CARTESIAN_POINT ( 'NONE',  ( 793.0897708529556667, -318.5545181178796952, 361.3366627262616362 ) ) ;
#12639 = ORIENTED_EDGE ( 'NONE', *, *, #1776, .T. ) ;
#12640 = CARTESIAN_POINT ( 'NONE',  ( 768.9521613784389729, -297.8272453906070041, 373.2346286133773106 ) ) ;
#12641 = CARTESIAN_POINT ( 'NONE',  ( 744.7301800767020268, -124.8164208402383366, -337.4774526936615189 ) ) ;
#12642 = CARTESIAN_POINT ( 'NONE',  ( 949.5497976682736407, 229.9999999999998579, 339.9999999999999432 ) ) ;
#12643 = CARTESIAN_POINT ( 'NONE',  ( 773.7305795820266212, -81.28179084515319630, 374.8230680027170365 ) ) ;
#12644 = CARTESIAN_POINT ( 'NONE',  ( 808.0189434323515343, -278.0891481129651197, -319.0252816721025511 ) ) ;
#12645 = FACE_BOUND ( 'NONE', #7016, .T. ) ;
#12646 = CARTESIAN_POINT ( 'NONE',  ( 795.1360043628807261, -164.0891481129655176, 360.2193346964456282 ) ) ;
#12647 = ORIENTED_EDGE ( 'NONE', *, *, #24620, .T. ) ;
#12648 = CARTESIAN_POINT ( 'NONE',  ( 810.1134526219336749, -344.5328690171410813, -357.8822607201570349 ) ) ;
#12649 = CARTESIAN_POINT ( 'NONE',  ( 796.7737145352015204, -92.63460265842026331, -370.7187646348536987 ) ) ;
#12650 = CARTESIAN_POINT ( 'NONE',  ( 805.2837595273609850, -50.73633629969874193, 340.5290396650784714 ) ) ;
#12651 = CARTESIAN_POINT ( 'NONE',  ( 767.6429770376289525, -369.1800572038739574, -306.8695393053162093 ) ) ;
#12652 = DIRECTION ( 'NONE',  ( 0.000000000000000000, 0.000000000000000000, 1.000000000000000000 ) ) ;
#12653 = CARTESIAN_POINT ( 'NONE',  ( 755.8398074228967971, -427.4419599262317888, 333.4516893846970333 ) ) ;
#12654 = ORIENTED_EDGE ( 'NONE', *, *, #15853, .T. ) ;
#12655 = CARTESIAN_POINT ( 'NONE',  ( 783.0433043558608688, -72.89650538077830788, 315.1538015810313027 ) ) ;
#12656 = CARTESIAN_POINT ( 'NONE',  ( 803.8556311672234642, -129.6237781080508853, -365.6418435158340117 ) ) ;
#12657 = CARTESIAN_POINT ( 'NONE',  ( -928.0249999999991815, 219.9999999999998863, 350.0000000000000000 ) ) ;
#12658 = CARTESIAN_POINT ( 'NONE',  ( 744.8212110874229666, -258.8965053807777963, 336.2046728542121627 ) ) ;
#12659 = CARTESIAN_POINT ( 'NONE',  ( 785.3687786644885591, -83.36187538569299704, 315.3201227861280813 ) ) ;
#12660 = ORIENTED_EDGE ( 'NONE', *, *, #40248, .T. ) ;
#12661 = CARTESIAN_POINT ( 'NONE',  ( 754.8983024940795303, -18.89650538077849617, -336.9254006560228163 ) ) ;
#12662 = CARTESIAN_POINT ( 'NONE',  ( 804.9363028652555840, -280.2709662947833067, 338.2165204200192079 ) ) ;
#12663 = CARTESIAN_POINT ( 'NONE',  ( 783.7566961878529810, -432.8965053807771142, -305.1792804349288417 ) ) ;
#12664 = CARTESIAN_POINT ( 'NONE',  ( 799.9999999999993179, -462.9681489794448339, 309.9999999999998863 ) ) ;
#12665 = ORIENTED_EDGE ( 'NONE', *, *, #5460, .F. ) ;
#12666 = ORIENTED_EDGE ( 'NONE', *, *, #11308, .T. ) ;
#12667 = CARTESIAN_POINT ( 'NONE',  ( 773.7305795820266212, -369.2817908451523294, -374.8230680027170365 ) ) ;
#12668 = CARTESIAN_POINT ( 'NONE',  ( 788.7366044899766848, -227.9073299311471033, -316.5762568750059813 ) ) ;
#12670 = CARTESIAN_POINT ( 'NONE',  ( 768.8385539511368734, -215.2601417444141987, 306.4236121716840557 ) ) ;
#12669 = CARTESIAN_POINT ( 'NONE',  ( 808.0189434323515343, -326.0891481129649492, 319.0252816721025511 ) ) ;
#12671 = CARTESIAN_POINT ( 'NONE',  ( 744.8212110874229666, -42.89650538077842157, 336.2046728542121627 ) ) ;
#12672 = CARTESIAN_POINT ( 'NONE',  ( 787.5531968255692163, -213.8272453906073167, -316.1348686366205811 ) ) ;
#12673 = CARTESIAN_POINT ( 'NONE',  ( 756.5762568750052424, -219.1800572038744122, -348.7366044899774238 ) ) ;
#12674 = CARTESIAN_POINT ( 'NONE',  ( 803.6646147819162707, -425.9073299311463643, -348.8264449731211130 ) ) ;
#12675 = VERTEX_POINT ( 'NONE', #25969 ) ;
#12676 = CARTESIAN_POINT ( 'NONE',  ( 805.1927285166397041, -208.8164208402380666, 341.8018195045277707 ) ) ;
#12677 = CARTESIAN_POINT ( 'NONE',  ( 800.0135310231082713, -110.0891481129656597, -325.0180583372163028 ) ) ;
#12678 = ORIENTED_EDGE ( 'NONE', *, *, #40804, .T. ) ;
#12679 = CARTESIAN_POINT ( 'NONE',  ( 772.4837098697144029, -359.3618753856920875, 374.5518280994205611 ) ) ;
#12680 = DIRECTION ( 'NONE',  ( -0.000000000000000000, 1.000000000000000000, -0.000000000000000000 ) ) ;
#12681 = CARTESIAN_POINT ( 'NONE',  ( 793.5727445751998630, 16.45630643248830793, 314.6726781324130684 ) ) ;
#12682 = LINE ( 'NONE', #13605, #41557 ) ;
#12683 = CARTESIAN_POINT ( 'NONE',  ( 802.9823548866075953, -193.0999726633346256, 330.0799878456151077 ) ) ;
#12684 = CARTESIAN_POINT ( 'NONE',  ( 765.0180583372156207, -72.99823902205667991, 360.0135310231089534 ) ) ;
#12685 = ORIENTED_EDGE ( 'NONE', *, *, #39938, .F. ) ;
#12686 = CARTESIAN_POINT ( 'NONE',  ( 814.8207195650702488, -434.1908817542430370, -336.2433038121456548 ) ) ;
#12687 = CARTESIAN_POINT ( 'NONE',  ( 813.1304606946831655, -41.90732993114767879, -352.3570229623691716 ) ) ;
#12688 = CARTESIAN_POINT ( 'NONE',  ( 804.1601925771018387, -271.4419599262321867, 346.5483106153029098 ) ) ;
#12689 = CARTESIAN_POINT ( 'NONE',  ( 804.4286716492782716, -401.3618753856920307, -345.3141322388244703 ) ) ;
#12690 = CARTESIAN_POINT ( 'NONE',  ( 791.9812246680005501, -20.63460265842048003, -361.9419747391813189 ) ) ;
#12691 = CARTESIAN_POINT ( 'NONE',  ( 787.5162901302840055, -443.3618753856917465, 305.4481719005792684 ) ) ;
#12692 = DIRECTION ( 'NONE',  ( 0.000000000000000000, 0.000000000000000000, 1.000000000000000000 ) ) ;
#12693 = CARTESIAN_POINT ( 'NONE',  ( 798.5707757039680246, -293.4636090269707438, -356.7845633553585003 ) ) ;
#12694 = CARTESIAN_POINT ( 'NONE',  ( 751.9810565676468741, -170.0891481129654608, -360.9747183278973921 ) ) ;
#12695 = CARTESIAN_POINT ( 'NONE',  ( 763.2262854647970016, -80.63460265842029173, 309.2812353651462445 ) ) ;
#12696 = CARTESIAN_POINT ( 'NONE',  ( 748.9653473494363425, -146.6346026584200217, 356.9462024416521331 ) ) ;
#12697 = VECTOR ( 'NONE', #9678, 1000.000000000000000 ) ;
#12698 = DIRECTION ( 'NONE',  ( 0.000000000000000000, 0.000000000000000000, 1.000000000000000000 ) ) ;
#12699 = DIRECTION ( 'NONE',  ( -0.000000000000000000, -0.000000000000000000, 1.000000000000000000 ) ) ;
#12700 = CARTESIAN_POINT ( 'NONE',  ( 807.5423716828161105, -225.0783235625959833, -362.2119215644372048 ) ) ;
#12701 = DIRECTION ( 'NONE',  ( -0.000000000000000000, 1.000000000000000000, -0.000000000000000000 ) ) ;
#12702 = CARTESIAN_POINT ( 'NONE',  ( 749.2812353651451076, -390.4527844766011526, 323.2262854647983090 ) ) ;
#12703 = CARTESIAN_POINT ( 'NONE',  ( 754.9967657858570647, -1.543693567511449594, 365.0032342141425943 ) ) ;
#12704 = CARTESIAN_POINT ( 'NONE',  ( 757.8323909638827445, -362.6346026584194533, -352.1044303154654358 ) ) ;
#12705 = CARTESIAN_POINT ( 'NONE',  ( 761.2382568024794409, 8.376221891948691933, 356.9571628226838129 ) ) ;
#12706 = AXIS2_PLACEMENT_3D ( 'NONE', #1053, #25768, #21619 ) ;
#12707 = CARTESIAN_POINT ( 'NONE',  ( 771.3260364891663130, -115.6454272087894424, -306.0683387631859773 ) ) ;
#12708 = CARTESIAN_POINT ( 'NONE',  ( 775.9200461376533440, -143.8055962898690154, -315.3028492785443291 ) ) ;
#12709 = CARTESIAN_POINT ( 'NONE',  ( 810.1134526219336749, -152.5328690171416781, 357.8822607201570349 ) ) ;
#12710 = CARTESIAN_POINT ( 'NONE',  ( 911.9999999999993179, 219.9999999999998863, 350.0000000000000000 ) ) ;
#12711 = CARTESIAN_POINT ( 'NONE',  ( 768.0187753319979720, -56.63460265842036279, -318.0580252608186242 ) ) ;
#12712 = CARTESIAN_POINT ( 'NONE',  ( 756.1348686366196716, -161.2601417444143976, -347.5531968255698416 ) ) ;
#12713 = CARTESIAN_POINT ( 'NONE',  ( 754.8072714833581358, -172.8164208402381234, 338.1981804954720587 ) ) ;
#12714 = CARTESIAN_POINT ( 'NONE',  ( 805.9055244015594326, -3.623778108051270319, -315.8990559732753240 ) ) ;
#12716 = CARTESIAN_POINT ( 'NONE',  ( 797.6776695296629214, -307.5436935675104451, 357.6776695296636603 ) ) ;
#12715 = CARTESIAN_POINT ( 'NONE',  ( 778.2165204200184689, -286.8164208402378677, 364.9363028652563230 ) ) ;
#12717 = CARTESIAN_POINT ( 'NONE',  ( 939.9999999999993179, 62.79977829742944095, -207.3621835540873235 ) ) ;
#12718 = VERTEX_POINT ( 'NONE', #32697 ) ;
#12719 = CARTESIAN_POINT ( 'NONE',  ( 779.4709603349208464, -0.3510508353240099355, 314.7162404726379918 ) ) ;
#12720 = CARTESIAN_POINT ( 'NONE',  ( 746.4236121716829757, -255.8272453906072315, -328.8385539511384650 ) ) ;
#12721 = ORIENTED_EDGE ( 'NONE', *, *, #42537, .T. ) ;
#12722 = APPLICATION_PROTOCOL_DEFINITION ( 'draft international standard', 'automotive_design', 1998, #15185 ) ;
#12723 = CARTESIAN_POINT ( 'NONE',  ( 796.9462024416508257, -228.4527844766016074, 308.9653473494370246 ) ) ;
#12724 = CARTESIAN_POINT ( 'NONE',  ( 798.5707757039680246, -293.4636090269707438, 356.7845633553585003 ) ) ;
#12725 = CARTESIAN_POINT ( 'NONE',  ( 786.6156483768007774, -385.4419599262319593, 315.5913626894246136 ) ) ;
#12726 = VERTEX_POINT ( 'NONE', #1044 ) ;
#12727 = CARTESIAN_POINT ( 'NONE',  ( 790.0220218866281812, -103.0999726633349525, -363.2186876482849129 ) ) ;
#12728 = CARTESIAN_POINT ( 'NONE',  ( 803.6646147819161570, -113.9073299311474301, -348.8264449731210561 ) ) ;
#12729 = VECTOR ( 'NONE', #36000, 1000.000000000000000 ) ;
#12730 = CARTESIAN_POINT ( 'NONE',  ( 788.7366044899766848, -299.9073299311468759, -316.5762568750059813 ) ) ;
#12731 = VERTEX_POINT ( 'NONE', #29240 ) ;
#12732 = CARTESIAN_POINT ( 'NONE',  ( 755.0636971347428243, -412.2709662947829088, -341.7834795799807353 ) ) ;
#12733 = CARTESIAN_POINT ( 'NONE',  ( 795.1360043628807261, -68.08914811296575920, -360.2193346964456282 ) ) ;
#12734 = CARTESIAN_POINT ( 'NONE',  ( 790.8726784830453198, -298.7146871989593251, 362.5472867521010585 ) ) ;
#12735 = CARTESIAN_POINT ( 'NONE',  ( -78.83651009197140525, 256.5000000000000568, -206.1189999999936049 ) ) ;
#12736 = PLANE ( 'NONE',  #37380 ) ;
#12737 = CARTESIAN_POINT ( 'NONE',  ( -728.8365100919714905, 230.0000000000001705, -202.7499999999889440 ) ) ;
#12738 = ORIENTED_EDGE ( 'NONE', *, *, #11477, .F. ) ;
#12739 = CARTESIAN_POINT ( 'NONE',  ( 793.5525998758768083, -343.0999726633342561, -372.6845335610516941 ) ) ;
#12740 = CARTESIAN_POINT ( 'NONE',  ( 814.4686193811664907, -195.2817908451528410, 346.2056067578752732 ) ) ;
#12741 = CARTESIAN_POINT ( 'NONE',  ( 762.1405469898971887, -289.5436935675103882, -357.8594530101015607 ) ) ;
#12742 = DIRECTION ( 'NONE',  ( 1.000000000000000000, 0.000000000000000000, 0.000000000000000000 ) ) ;
#12743 = CARTESIAN_POINT ( 'NONE',  ( 755.8894580844503253, -183.8272453906074020, -332.3691319403863531 ) ) ;
#12744 = EDGE_CURVE ( 'NONE', #32355, #31022, #16675, .T. ) ;
#12745 = CARTESIAN_POINT ( 'NONE',  ( 772.4837098697144029, -47.36187538569312494, 374.5518280994205611 ) ) ;
#12746 = CARTESIAN_POINT ( 'NONE',  ( -775.4999999999993179, -544.8427095258973623, -350.0000000000000000 ) ) ;
#12747 = CARTESIAN_POINT ( 'NONE',  ( 767.7687537140311633, -383.9073299311466485, -372.7932403749916830 ) ) ;
#12748 = DIRECTION ( 'NONE',  ( 0.000000000000000000, 0.000000000000000000, 1.000000000000000000 ) ) ;
#12749 = CARTESIAN_POINT ( 'NONE',  ( 759.7806653035534055, -30.99823902205680071, 324.8639956371180801 ) ) ;
#12750 = CARTESIAN_POINT ( 'NONE',  ( 754.3581564841646241, -329.4636090269706870, 316.1443688327762516 ) ) ;
#12751 = CARTESIAN_POINT ( 'NONE',  ( 746.8695393053150156, -269.9073299311468190, 327.6429770376306010 ) ) ;
#12752 = CARTESIAN_POINT ( 'NONE',  ( 747.2067596250078623, -27.18005720387500901, -352.2312462859687230 ) ) ;
#12753 = CARTESIAN_POINT ( 'NONE',  ( 762.3223304703356007, -247.5436935675106724, -322.3223304703362828 ) ) ;
#12754 = DIRECTION ( 'NONE',  ( 1.000000000000000000, 0.000000000000000000, 0.000000000000000000 ) ) ;
#12755 = CARTESIAN_POINT ( 'NONE',  ( 756.3353852180819104, -365.9073299311465917, 331.1735550268788302 ) ) ;
#12756 = CIRCLE ( 'NONE', #44484, 9.999999999999982236 ) ;
#12757 = CARTESIAN_POINT ( 'NONE',  ( 772.4468031744293057, -105.8272453906076578, 363.8651313633793620 ) ) ;
#12758 = CARTESIAN_POINT ( 'NONE',  ( 789.9200121543843807, -49.98741447168749374, -317.0176451133914384 ) ) ;
#12759 = CARTESIAN_POINT ( 'NONE',  ( 759.8311093483677041, -46.16923265350568784, 310.9282345327691814 ) ) ;
#12760 = CARTESIAN_POINT ( 'NONE',  ( 778.2165204200184689, -358.8164208402375834, 364.9363028652563230 ) ) ;
#12761 = DIRECTION ( 'NONE',  ( -0.000000000000000000, -0.000000000000000000, -1.000000000000000000 ) ) ;
#12762 = DIRECTION ( 'NONE',  ( 0.000000000000000000, -0.9235249282889854694, 0.3835384033298675499 ) ) ;
#12763 = CARTESIAN_POINT ( 'NONE',  ( 764.8639956371174549, -392.0891481129648355, 319.7806653035542013 ) ) ;
#12764 = VERTEX_POINT ( 'NONE', #28780 ) ;
#12765 = CARTESIAN_POINT ( 'NONE',  ( 772.3691319403857278, -335.2601417444137724, -315.8894580844506663 ) ) ;
#12767 = CARTESIAN_POINT ( 'NONE',  ( 778.2165204200184689, -190.8164208402381234, 364.9363028652563230 ) ) ;
#12766 = CARTESIAN_POINT ( 'NONE',  ( 792.1044303154645831, -180.4527844766017211, 317.8323909638837677 ) ) ;
#12768 = CARTESIAN_POINT ( 'NONE',  ( 801.9858362298568863, -363.0783235625955854, -312.7379699480935642 ) ) ;
#12769 = CYLINDRICAL_SURFACE ( 'NONE', #41113, 1.000000000000000888 ) ;
#12770 = EDGE_LOOP ( 'NONE', ( #42336, #12117, #28889, #40301 ) ) ;
#12771 = CARTESIAN_POINT ( 'NONE',  ( 804.6798772138708955, -351.7255117493284047, 334.6312213355107019 ) ) ;
#12772 =( GEOMETRIC_REPRESENTATION_CONTEXT ( 3 ) GLOBAL_UNCERTAINTY_ASSIGNED_CONTEXT ( ( #15357 ) ) GLOBAL_UNIT_ASSIGNED_CONTEXT ( ( #25332, #29037, #8245 ) ) REPRESENTATION_CONTEXT ( 'NONE', 'WORKASPACE' ) );
#12773 = CARTESIAN_POINT ( 'NONE',  ( 772.3691319403857278, -95.26014174441461080, -315.8894580844506663 ) ) ;
#12774 = ORIENTED_EDGE ( 'NONE', *, *, #43315, .F. ) ;
#12775 = CARTESIAN_POINT ( 'NONE',  ( 782.4968714119720516, -226.8164208402380098, -305.0891759886411023 ) ) ;
#12776 = CARTESIAN_POINT ( 'NONE',  ( 777.5031285880264704, -118.8164208402383508, 374.9108240113588408 ) ) ;
#12777 = EDGE_LOOP ( 'NONE', ( #26206, #4904, #41721, #28345 ) ) ;
#12778 = CARTESIAN_POINT ( 'NONE',  ( 754.8072714833583632, -172.8164208402381519, -338.1981804954721156 ) ) ;
#12779 = VERTEX_POINT ( 'NONE', #603 ) ;
#12780 = CARTESIAN_POINT ( 'NONE',  ( 781.7834795799800531, -322.8164208402377540, -315.0636971347436202 ) ) ;
#12781 = CARTESIAN_POINT ( 'NONE',  ( 800.9840315886518738, -460.9181544815156713, -354.1144889064786412 ) ) ;
#12782 = CARTESIAN_POINT ( 'NONE',  ( 787.5162901302840055, -251.3618753856923149, 305.4481719005792684 ) ) ;
#12783 = CARTESIAN_POINT ( 'NONE',  ( 780.5290396650775619, -180.3510508353234343, 365.2837595273619513 ) ) ;
#12785 = CYLINDRICAL_SURFACE ( 'NONE', #25539, 18.00000000000001421 ) ;
#12784 = PLANE ( 'NONE',  #38786 ) ;
#12786 = CARTESIAN_POINT ( 'NONE',  ( -26.63011601220122060, 26.27639943461401018, 900.0000000000001137 ) ) ;
#12787 = EDGE_CURVE ( 'NONE', #28399, #11791, #43087, .T. ) ;
#12788 = VERTEX_POINT ( 'NONE', #35464 ) ;
#12789 = CARTESIAN_POINT ( 'NONE',  ( 779.4763451958990572, -440.7363362996975980, -365.0264073115438919 ) ) ;
#12790 = CARTESIAN_POINT ( 'NONE',  ( 939.9999999999993179, -407.8586036264139807, 201.9999999999998863 ) ) ;
#12791 = LINE ( 'NONE', #26647, #18893 ) ;
#12792 = VECTOR ( 'NONE', #13836, 1000.000000000000000 ) ;
#12793 = VERTEX_POINT ( 'NONE', #40075 ) ;
#12794 = CARTESIAN_POINT ( 'NONE',  ( 748.6759233522253680, -232.3726999360617924, -324.3348316497537098 ) ) ;
#12795 = AXIS2_PLACEMENT_3D ( 'NONE', #37404, #44560, #16379 ) ;
#12796 = CARTESIAN_POINT ( 'NONE',  ( 776.2046728542105711, -116.1908817542440033, 304.8212110874238761 ) ) ;
#12798 = CARTESIAN_POINT ( 'NONE',  ( 781.7834795799800531, -202.8164208402380950, -315.0636971347436202 ) ) ;
#12797 = CARTESIAN_POINT ( 'NONE',  ( -858.8365100919713768, 258.0940000000002215, -199.9999999999881481 ) ) ;
#12799 = CARTESIAN_POINT ( 'NONE',  ( 804.1601925771018387, -367.4419599262319025, -346.5483106153029098 ) ) ;
#12800 = CARTESIAN_POINT ( 'NONE',  ( 775.4999999999993179, -513.1383975375929367, -367.9999999999999432 ) ) ;
#12801 = CARTESIAN_POINT ( 'NONE',  ( 754.3581564841646241, -209.4636090269709996, -316.1443688327762516 ) ) ;
#12802 = CARTESIAN_POINT ( 'NONE',  ( 1238.921997096861332, 579.9999999999998863, -360.0000000000000000 ) ) ;
#12803 = LINE ( 'NONE', #34271, #964 ) ;
#12804 = CARTESIAN_POINT ( 'NONE',  ( 763.8424801807145741, -66.00906357242595845, -320.5453621957614700 ) ) ;
#12805 = ADVANCED_FACE ( 'NONE', ( #29458 ), #44701, .F. ) ;
#12806 = CARTESIAN_POINT ( 'NONE',  ( 793.9708237608222134, -430.9181544815157849, 319.2295555964448681 ) ) ;
#12807 = CARTESIAN_POINT ( 'NONE',  ( 791.0478386215596629, -357.8272453906068904, 306.7653713866226326 ) ) ;
#12808 = CARTESIAN_POINT ( 'NONE',  ( -786.4999999999993179, -513.1383975375929367, -369.9999999999999432 ) ) ;
#12809 = CARTESIAN_POINT ( 'NONE',  ( 802.7791456095903868, -436.7146871989589272, -329.0155153010375102 ) ) ;
#12810 = CARTESIAN_POINT ( 'NONE',  ( 772.4837098697145166, -287.3618753856923718, -374.5518280994205611 ) ) ;
#12811 = FACE_OUTER_BOUND ( 'NONE', #10466, .T. ) ;
#12812 = CARTESIAN_POINT ( 'NONE',  ( 799.9999999999993179, 205.0000000000000568, -339.9999999999999432 ) ) ;
#12813 = CARTESIAN_POINT ( 'NONE',  ( 785.3141322388236176, -45.72551174932949181, -364.4286716492789537 ) ) ;
#12814 = VECTOR ( 'NONE', #22953, 1000.000000000000000 ) ;
#12815 = CARTESIAN_POINT ( 'NONE',  ( 748.6759233522253680, -232.3726999360617924, 324.3348316497537098 ) ) ;
#12816 = CARTESIAN_POINT ( 'NONE',  ( 815.1787889125755555, -174.8965053807779952, -343.7953271457877804 ) ) ;
#12817 = CARTESIAN_POINT ( 'NONE',  ( 815.2698199232961542, -160.8164208402382371, 342.5225473063383106 ) ) ;
#12818 = CARTESIAN_POINT ( 'NONE',  ( 800.9747183278959710, -396.9982390220556567, -311.9810565676471583 ) ) ;
#12819 = CARTESIAN_POINT ( 'NONE',  ( 919.9999999999993179, 154.9999999999998863, -359.9749999999999659 ) ) ;
#12820 = CARTESIAN_POINT ( 'NONE',  ( 800.2193346964447755, -258.9982390220561115, 355.1360043628815788 ) ) ;
#12821 = CARTESIAN_POINT ( 'NONE',  ( 776.9254006560222479, -44.19088175424421649, 314.8983024940802125 ) ) ;
#12822 = EDGE_CURVE ( 'NONE', #11865, #27126, #29003, .T. ) ;
#12823 = CARTESIAN_POINT ( 'NONE',  ( 804.4286716492782716, -377.3618753856920875, -345.3141322388244703 ) ) ;
#12824 = FACE_OUTER_BOUND ( 'NONE', #21247, .T. ) ;
#12826 = ADVANCED_FACE ( 'NONE', ( #22068 ), #39408, .F. ) ;
#12825 = CARTESIAN_POINT ( 'NONE',  ( 793.3938497862117174, -453.0432664090020580, 372.3358127763067955 ) ) ;
#12827 = CARTESIAN_POINT ( 'NONE',  ( 804.9511171171677688, -101.8055962898691718, 335.8780910478229202 ) ) ;
#12828 = ORIENTED_EDGE ( 'NONE', *, *, #8660, .F. ) ;
#12829 = CARTESIAN_POINT ( 'NONE',  ( 766.7756240680305382, -230.5328690171415076, -361.5560724626415663 ) ) ;
#12830 = AXIS2_PLACEMENT_3D ( 'NONE', #24559, #9589, #27360 ) ;
#12831 = CARTESIAN_POINT ( 'NONE',  ( 797.8594530101008786, -61.54369356751124087, 322.1405469898980982 ) ) ;
#12832 = VECTOR ( 'NONE', #6346, 1000.000000000000000 ) ;
#12833 = CARTESIAN_POINT ( 'NONE',  ( 815.0009284576459549, -246.3510508353232638, -338.7629533639073429 ) ) ;
#12834 = CARTESIAN_POINT ( 'NONE',  ( 751.2241431872005251, -376.1692326535046504, 359.9636004259367610 ) ) ;
#12835 = ORIENTED_EDGE ( 'NONE', *, *, #40510, .T. ) ;
#12836 = CARTESIAN_POINT ( 'NONE',  ( 767.7687537140311633, 0.09267006885218045942, 372.7932403749916830 ) ) ;
#12837 = CARTESIAN_POINT ( 'NONE',  ( 783.0433043558608688, -24.89650538077847486, -315.1538015810313027 ) ) ;
#12838 = CARTESIAN_POINT ( 'NONE',  ( 759.7806653035534055, -174.9982390220563673, -324.8639956371180801 ) ) ;
#12839 = CARTESIAN_POINT ( 'NONE',  ( 759.9864689768902508, -386.0891481129647786, 354.9819416627836404 ) ) ;
#12840 = CARTESIAN_POINT ( 'NONE',  ( 811.0346526505616112, -86.63460265842023489, -323.0537975583477532 ) ) ;
#12841 = CARTESIAN_POINT ( 'NONE',  ( 797.8594530101009923, -61.54369356751124798, -322.1405469898982119 ) ) ;
#12842 = EDGE_LOOP ( 'NONE', ( #21763, #36658 ) ) ;
#12843 = CARTESIAN_POINT ( 'NONE',  ( 784.1219089521767955, -21.28179084515337749, -315.0488828828318333 ) ) ;
#12844 = VERTEX_POINT ( 'NONE', #14470 ) ;
#12845 = CARTESIAN_POINT ( 'NONE',  ( 769.9779781133707957, -355.0999726633341993, -316.7813123517150871 ) ) ;
#12846 = CIRCLE ( 'NONE', #18763, 12.00000000000001066 ) ;
#12847 = EDGE_CURVE ( 'NONE', #37198, #9279, #32243, .T. ) ;
#12849 = CARTESIAN_POINT ( 'NONE',  ( 801.5560724626406000, -408.5545181178794110, 326.7756240680316182 ) ) ;
#12848 = CARTESIAN_POINT ( 'NONE',  ( 801.9419747391806368, -90.45278447660209054, 351.9812246680014027 ) ) ;
#12850 = CARTESIAN_POINT ( 'NONE',  ( 795.9930595647434757, -99.07832356259642381, 320.7433823573372820 ) ) ;
#12853 = CARTESIAN_POINT ( 'NONE',  ( 745.1769319972822814, -353.8055962898683333, 346.2694204179732083 ) ) ;
#12852 = CARTESIAN_POINT ( 'NONE',  ( 181.1634899080285948, 260.0000000000000000, -197.2499999999955662 ) ) ;
#12851 = CARTESIAN_POINT ( 'NONE',  ( 772.5602148656447525, -441.7255117493282910, 305.7998596910095443 ) ) ;
#12854 = VECTOR ( 'NONE', #15829, 1000.000000000000000 ) ;
#12855 = EDGE_CURVE ( 'NONE', #39585, #26480, #11225, .T. ) ;
#12856 = CARTESIAN_POINT ( 'NONE',  ( 759.8311093483677041, -118.1692326535054463, 310.9282345327691814 ) ) ;
#12857 = CARTESIAN_POINT ( 'NONE',  ( 798.5707757039680246, -317.4636090269706301, -356.7845633553585003 ) ) ;
#12858 = CARTESIAN_POINT ( 'NONE',  ( 767.8955696845333705, -312.4527844766012663, -362.1676090361162323 ) ) ;
#12859 = CARTESIAN_POINT ( 'NONE',  ( 809.0717654672305343, -148.9181544815166092, -360.1688906516309885 ) ) ;
#12860 = CARTESIAN_POINT ( 'NONE',  ( 791.0478386215596629, 2.172754609392001601, 306.7653713866226326 ) ) ;
#12862 = DIRECTION ( 'NONE',  ( 0.000000000000000000, 0.000000000000000000, -1.000000000000000000 ) ) ;
#12861 = DIRECTION ( 'NONE',  ( 1.000000000000000000, 0.000000000000000000, 0.000000000000000000 ) ) ;
#12863 = CARTESIAN_POINT ( 'NONE',  ( 803.2186876482843445, -271.9874144716868045, -350.0220218866286928 ) ) ;
#12864 = CARTESIAN_POINT ( 'NONE',  ( 750.9282345327678740, -112.9181544815167229, -319.8311093483690115 ) ) ;
#12865 = CARTESIAN_POINT ( 'NONE',  ( 879.9999999999992042, 99.99999999999984368, -360.0000000000000000 ) ) ;
#12866 = DIRECTION ( 'NONE',  ( -0.000000000000000000, 1.000000000000000000, -0.000000000000000000 ) ) ;
#12867 = ADVANCED_FACE ( 'NONE', ( #18393 ), #28549, .F. ) ;
#12868 = CARTESIAN_POINT ( 'NONE',  ( 796.9571628226829034, -335.4636090269705733, 321.2382568024804641 ) ) ;
#12869 = VECTOR ( 'NONE', #25020, 1000.000000000000000 ) ;
#12870 = CARTESIAN_POINT ( 'NONE',  ( 785.3141322388236176, -189.7255117493290300, 364.4286716492789537 ) ) ;
#12871 = ORIENTED_EDGE ( 'NONE', *, *, #4666, .F. ) ;
#12872 = CARTESIAN_POINT ( 'NONE',  ( 778.7629533639073998, -296.7363362996979390, 375.0009284576466371 ) ) ;
#12873 = CARTESIAN_POINT ( 'NONE',  ( 814.2001403089898304, -185.3618753856926844, -347.4397851343538264 ) ) ;
#12874 = FACE_OUTER_BOUND ( 'NONE', #32634, .T. ) ;
#12875 = CARTESIAN_POINT ( 'NONE',  ( 781.2370466360911223, -116.7363362996985217, 304.9990715423533629 ) ) ;
#12876 = CARTESIAN_POINT ( 'NONE',  ( 782.4968714119720516, -298.8164208402377540, -305.0891759886411023 ) ) ;
#12877 = LINE ( 'NONE', #26962, #45140 ) ;
#12878 = CARTESIAN_POINT ( 'NONE',  ( 765.0180583372156207, -144.9982390220564525, 360.0135310231089534 ) ) ;
#12879 = ORIENTED_EDGE ( 'NONE', *, *, #9669, .F. ) ;
#12880 = CARTESIAN_POINT ( 'NONE',  ( 768.9521613784389729, -417.8272453906067199, 373.2346286133773106 ) ) ;
#12881 = CARTESIAN_POINT ( 'NONE',  ( 795.6651683502461765, -346.7146871989592682, -371.3240766477733814 ) ) ;
#12882 = CARTESIAN_POINT ( 'NONE',  ( 800.9747183278959710, -108.9982390220565804, -311.9810565676471583 ) ) ;
#12883 = CIRCLE ( 'NONE', #4777, 7.999999999999896083 ) ;
#12884 = CARTESIAN_POINT ( 'NONE',  ( 755.1538015810308480, -38.19088175424422360, 343.0433043558613804 ) ) ;
#12885 = CARTESIAN_POINT ( 'NONE',  ( 814.5518280994195948, -399.7255117493283478, -332.4837098697145734 ) ) ;
#12886 = DIRECTION ( 'NONE',  ( 0.000000000000000000, 0.000000000000000000, 1.000000000000000000 ) ) ;
#12887 = CARTESIAN_POINT ( 'NONE',  ( 788.4001350590139054, -443.1233509495419298, 363.5803521658918385 ) ) ;
#12888 = EDGE_LOOP ( 'NONE', ( #45405, #20278, #11873, #32537 ) ) ;
#12889 = CARTESIAN_POINT ( 'NONE',  ( 801.3366627262608972, -80.53286901714194812, 353.0897708529566899 ) ) ;
#12890 = CIRCLE ( 'NONE', #16593, 8.024999999999948841 ) ;
#12891 = CARTESIAN_POINT ( 'NONE',  ( 794.9819416627830151, -228.9982390220561683, -319.9864689768909898 ) ) ;
#12892 = CARTESIAN_POINT ( 'NONE',  ( 788.7631598425961101, -169.4419599262325562, -305.7194118038759143 ) ) ;
#12893 = DIRECTION ( 'NONE',  ( -1.000000000000000000, -0.000000000000000000, -0.000000000000000000 ) ) ;
#12894 = CARTESIAN_POINT ( 'NONE',  ( 754.0944755984390895, -279.6237781080503737, 364.1009440267246760 ) ) ;
#12895 = CARTESIAN_POINT ( 'NONE',  ( 756.5762568750052424, -75.18005720387485269, 348.7366044899774238 ) ) ;
#12896 = ORIENTED_EDGE ( 'NONE', *, *, #40197, .F. ) ;
#12897 = CARTESIAN_POINT ( 'NONE',  ( 758.6633372737375112, 3.467130982857797417, -326.9102291470432533 ) ) ;
#12898 = CARTESIAN_POINT ( 'NONE',  ( 797.8594530101008786, -277.5436935675105019, 322.1405469898980982 ) ) ;
#12899 = CLOSED_SHELL ( 'NONE', ( #9161, #5465, #28901, #16248, #41046, #2047, #41289, #37100, #9051, #28925, #23522, #31474, #7758, #23576, #23006, #3744, #41360, #38827, #34309, #35280, #28661, #15958, #14434, #8650, #32602, #11699, #29669, #22647, #21316, #35381, #19329, #36813, #39663, #4436, #26113, #24140, #45577, #8897, #24415, #1901, #43841, #6598, #13670, #44165, #44140, #41085, #467, #26031, #4934, #7751 ) ) ;
#12900 = CARTESIAN_POINT ( 'NONE',  ( 813.2346286133761168, -437.2601417444135450, -328.9521613784389160 ) ) ;
#12901 = LINE ( 'NONE', #26526, #43126 ) ;
#12902 = AXIS2_PLACEMENT_3D ( 'NONE', #9010, #23080, #26778 ) ;
#12903 = ORIENTED_EDGE ( 'NONE', *, *, #15105, .T. ) ;
#12904 = CARTESIAN_POINT ( 'NONE',  ( 814.2805881961230625, -361.6454272087887603, -331.2368401574024119 ) ) ;
#12905 = CONICAL_SURFACE ( 'NONE', #8501, 8.024999999999948841, 0.7853981633974337351 ) ;
#12906 = EDGE_CURVE ( 'NONE', #11328, #24400, #36158, .T. ) ;
#12908 = CARTESIAN_POINT ( 'NONE',  ( 798.0661480581538854, -218.5328690171414792, 309.5768839229118043 ) ) ;
#12907 = CARTESIAN_POINT ( 'NONE',  ( 777.5031285880264704, -310.8164208402377540, 374.9108240113588408 ) ) ;
#12909 = CARTESIAN_POINT ( 'NONE',  ( 760.7433823573367135, -204.0090635724255606, -355.9930595647440441 ) ) ;
#12910 = CARTESIAN_POINT ( 'NONE',  ( 801.9419747391806368, -234.4527844766016358, -351.9812246680014027 ) ) ;
#12911 = CARTESIAN_POINT ( 'NONE',  ( 755.0636971347428243, -412.2709662947829088, -341.7834795799807353 ) ) ;
#12912 = AXIS2_PLACEMENT_3D ( 'NONE', #13796, #21168, #7320 ) ;
#12913 = EDGE_LOOP ( 'NONE', ( #33250, #23393 ) ) ;
#12914 = CARTESIAN_POINT ( 'NONE',  ( 768.0187753319979720, -104.6346026584202207, -318.0580252608186242 ) ) ;
#12915 = EDGE_LOOP ( 'NONE', ( #45177, #30430, #8190, #7941, #26500 ) ) ;
#12916 = CARTESIAN_POINT ( 'NONE',  ( 804.7487373415286811, -355.5436935675103882, 364.7487373415288516 ) ) ;
#12917 = CIRCLE ( 'NONE', #40230, 6.118999999999985562 ) ;
#12918 = DIRECTION ( 'NONE',  ( 1.000000000000000000, -0.000000000000000000, -0.000000000000000000 ) ) ;
#12919 = CARTESIAN_POINT ( 'NONE',  ( 791.3765159950071393, 16.45630643248849623, 314.4691821868552211 ) ) ;
#12920 = FACE_OUTER_BOUND ( 'NONE', #29238, .T. ) ;
#12921 = AXIS2_PLACEMENT_3D ( 'NONE', #2144, #33792, #23139 ) ;
#12922 = CARTESIAN_POINT ( 'NONE',  ( 757.0176451133909268, -229.0999726633345404, 349.9200121543848354 ) ) ;
#12923 = AXIS2_PLACEMENT_3D ( 'NONE', #36384, #39878, #8219 ) ;
#12924 = CARTESIAN_POINT ( 'NONE',  ( 767.8955696845333705, -96.45278447660203369, 362.1676090361162323 ) ) ;
#12925 = CARTESIAN_POINT ( 'NONE',  ( 791.0478386215596629, -453.8272453906066630, -306.7653713866226326 ) ) ;
#12926 = CARTESIAN_POINT ( 'NONE',  ( 808.0189434323515343, -62.08914811296580183, -319.0252816721025511 ) ) ;
#12927 = CARTESIAN_POINT ( 'NONE',  ( 790.8726784830453198, -274.7146871989594388, 362.5472867521010585 ) ) ;
#12928 = CARTESIAN_POINT ( 'NONE',  ( 792.1044303154645831, -444.4527844766009821, -317.8323909638837677 ) ) ;
#12929 = CARTESIAN_POINT ( 'NONE',  ( 756.3353852180820240, -29.90732993114772142, -331.1735550268787733 ) ) ;
#12930 = CARTESIAN_POINT ( 'NONE',  ( 804.7487373415286811, -451.5436935675099903, 364.7487373415288516 ) ) ;
#12931 = LINE ( 'NONE', #2523, #2586 ) ;
#12932 = CARTESIAN_POINT ( 'NONE',  ( 757.0176451133909268, -301.0999726633342561, -349.9200121543848354 ) ) ;
#12933 = CARTESIAN_POINT ( 'NONE',  ( 746.8695393053150156, -197.9073299311472169, -327.6429770376306010 ) ) ;
#12934 = CARTESIAN_POINT ( 'NONE',  ( 804.7487373415286811, -91.54369356751116982, 364.7487373415288516 ) ) ;
#12935 = CARTESIAN_POINT ( 'NONE',  ( 782.4968714119720516, -130.8164208402383224, 305.0891759886411023 ) ) ;
#12936 = DIRECTION ( 'NONE',  ( 0.7071067811865697772, 0.000000000000000000, 0.7071067811865252573 ) ) ;
#12937 = VECTOR ( 'NONE', #44435, 1000.000000000000000 ) ;
#12938 = DIRECTION ( 'NONE',  ( -0.000000000000000000, 1.000000000000000000, -0.000000000000000000 ) ) ;
#12939 = CARTESIAN_POINT ( 'NONE',  ( 814.8230680027162407, -221.8055962898687881, -333.7305795820267917 ) ) ;
#12940 = VECTOR ( 'NONE', #37098, 1000.000000000000000 ) ;
#12941 = CARTESIAN_POINT ( 'NONE',  ( 788.6739635108323228, -415.6454272087885897, 373.9316612368139090 ) ) ;
#12942 = CARTESIAN_POINT ( 'NONE',  ( 782.5225473063381969, -286.2709662947833635, -375.2698199232970637 ) ) ;
#12943 = CARTESIAN_POINT ( 'NONE',  ( 759.9999999999992042, 166.4563064324884465, 319.9999999999999432 ) ) ;
#12944 = CARTESIAN_POINT ( 'NONE',  ( 744.7301800767019131, -412.8164208402372992, 337.4774526936615757 ) ) ;
#12945 = CARTESIAN_POINT ( 'NONE',  ( 801.1904061080338124, 3.910851887033986785, 368.3070685750236066 ) ) ;
#12947 = AXIS2_PLACEMENT_3D ( 'NONE', #7766, #32477, #21614 ) ;
#12946 = CARTESIAN_POINT ( 'NONE',  ( 756.5762568750052424, -339.1800572038740142, -348.7366044899774238 ) ) ;
#12948 = CARTESIAN_POINT ( 'NONE',  ( 775.9200461376533440, -23.80559628986938847, 315.3028492785443291 ) ) ;
#12949 = CARTESIAN_POINT ( 'NONE',  ( 795.8262568251477660, -94.37269993606224716, -308.3538107759623585 ) ) ;
#12950 = CARTESIAN_POINT ( 'NONE',  ( 783.0433043558608688, -144.8965053807781089, -315.1538015810313027 ) ) ;
#12951 = CARTESIAN_POINT ( 'NONE',  ( 800.1688906516307043, -154.1692326535053894, 369.0717654672308186 ) ) ;
#12952 = CARTESIAN_POINT ( 'NONE',  ( 804.9363028652555840, 7.729033705215793582, 338.2165204200192079 ) ) ;
#12953 = ORIENTED_EDGE ( 'NONE', *, *, #12607, .T. ) ;
#12954 = CARTESIAN_POINT ( 'NONE',  ( 804.4286716492782716, -65.36187538569306810, -345.3141322388244703 ) ) ;
#12955 = CARTESIAN_POINT ( 'NONE',  ( 799.4546378042377910, -153.0783235625962675, -356.1575198192848006 ) ) ;
#12956 = CARTESIAN_POINT ( 'NONE',  ( 756.3353852180819104, -173.9073299311472169, 331.1735550268788302 ) ) ;
#12957 = CONICAL_SURFACE ( 'NONE', #7799, 8.024999999999948841, 0.7853981633974337351 ) ;
#12958 = PRODUCT_DEFINITION_SHAPE ( 'NONE', 'NONE',  #21378 ) ;
#12959 = CARTESIAN_POINT ( 'NONE',  ( 814.8230680027162407, 18.19440371013048008, -333.7305795820267917 ) ) ;
#12960 = CARTESIAN_POINT ( 'NONE',  ( 791.9812246680005501, -308.6346026584195670, 361.9419747391813189 ) ) ;
#12961 = DIRECTION ( 'NONE',  ( -0.000000000000000000, 1.000000000000000000, -0.000000000000000000 ) ) ;
#12962 = ORIENTED_EDGE ( 'NONE', *, *, #1239, .F. ) ;
#12963 = CARTESIAN_POINT ( 'NONE',  ( 799.4546378042377910, -9.078323562596708030, 356.1575198192848006 ) ) ;
#12964 = CARTESIAN_POINT ( 'NONE',  ( 766.4474001241216001, -283.0999726633344267, -307.3154664389482491 ) ) ;
#12965 = EDGE_LOOP ( 'NONE', ( #19216, #2436 ) ) ;
#12966 =( LENGTH_UNIT ( ) NAMED_UNIT ( * ) SI_UNIT ( .MILLI., .METRE. ) );
#12967 = CARTESIAN_POINT ( 'NONE',  ( 777.5031285880264704, -214.8164208402380666, 374.9108240113588408 ) ) ;
#12968 = CARTESIAN_POINT ( 'NONE',  ( 754.7162404726377645, -302.7363362996979959, 339.4709603349214717 ) ) ;
#12969 = CARTESIAN_POINT ( 'NONE',  ( 801.3366627262608972, -440.5328690171407970, 353.0897708529566899 ) ) ;
#12970 = ORIENTED_EDGE ( 'NONE', *, *, #6919, .T. ) ;
#12971 = CARTESIAN_POINT ( 'NONE',  ( 775.8780910478218402, -105.2817908451530968, -364.9511171171680530 ) ) ;
#12972 = CARTESIAN_POINT ( 'NONE',  ( 759.9864689768902508, -98.08914811296568814, -354.9819416627836404 ) ) ;
#12974 = ADVANCED_FACE ( 'NONE', ( #14922 ), #39185, .T. ) ;
#12973 = CARTESIAN_POINT ( 'NONE',  ( 758.0580252608178853, -318.4527844766014368, -328.0187753319985404 ) ) ;
#12975 = VECTOR ( 'NONE', #38906, 1000.000000000000000 ) ;
#12976 = ORIENTED_EDGE ( 'NONE', *, *, #20505, .F. ) ;
#12977 = CARTESIAN_POINT ( 'NONE',  ( 778.1981804954714335, -442.2709662947826814, -314.8072714833589885 ) ) ;
#12978 = CIRCLE ( 'NONE', #38804, 8.024999999999948841 ) ;
#12979 = CARTESIAN_POINT ( 'NONE',  ( 769.1273215169530886, -310.7146871989593251, 317.4527132478988847 ) ) ;
#12980 = FACE_OUTER_BOUND ( 'NONE', #40467, .T. ) ;
#12981 = AXIS2_PLACEMENT_3D ( 'NONE', #36377, #4740, #18844 ) ;
#12982 = CYLINDRICAL_SURFACE ( 'NONE', #28553, 2.749999999999863665 ) ;
#12983 = CARTESIAN_POINT ( 'NONE',  ( 804.8461984189677878, -122.1908817542439749, 336.9566956441385628 ) ) ;
#12984 = CARTESIAN_POINT ( 'NONE',  ( 879.9999999999992042, 259.9999999999998863, -179.9999999999999716 ) ) ;
#12985 = EDGE_LOOP ( 'NONE', ( #182, #583, #15784, #6654 ) ) ;
#12986 = CARTESIAN_POINT ( 'NONE',  ( 744.6391490659812007, -326.7363362996979390, -338.7502325331110455 ) ) ;
#12987 = CARTESIAN_POINT ( 'NONE',  ( 786.2694204179717872, -189.2817908451528979, 305.1769319972829067 ) ) ;
#12988 = CARTESIAN_POINT ( 'NONE',  ( 778.2165204200184689, -334.8164208402376403, -364.9363028652563230 ) ) ;
#12989 = CARTESIAN_POINT ( 'NONE',  ( 790.9844846989617508, -190.3726999360619629, -317.2208543904092721 ) ) ;
#12990 = AXIS2_PLACEMENT_3D ( 'NONE', #36612, #40071, #44208 ) ;
#12991 = CARTESIAN_POINT ( 'NONE',  ( 805.0032342141412300, -61.54369356751124087, 314.9967657858571783 ) ) ;
#12992 = DIRECTION ( 'NONE',  ( -1.000000000000000000, -0.000000000000000000, -0.000000000000000000 ) ) ;
#12993 = CARTESIAN_POINT ( 'NONE',  ( 796.7737145352015204, -380.6346026584192828, -370.7187646348536987 ) ) ;
#12994 = LINE ( 'NONE', #27081, #20250 ) ;
#12995 = CARTESIAN_POINT ( 'NONE',  ( 762.1177392798416577, -330.5545181178796952, 309.8865473780659272 ) ) ;
#12996 = CARTESIAN_POINT ( 'NONE',  ( 701.1634899080286232, 259.9999999999999432, -199.9999999999990337 ) ) ;
#12997 = CARTESIAN_POINT ( 'NONE',  ( 755.2512626584698410, -295.5436935675105588, 315.2512626584710915 ) ) ;
#12998 = CARTESIAN_POINT ( 'NONE',  ( 751.6929314249748586, -6.998239022056885972, -318.8095938919659034 ) ) ;
#12999 = CARTESIAN_POINT ( 'NONE',  ( 804.9363028652555840, -256.2709662947834204, -338.2165204200192079 ) ) ;
#13000 = PLANE ( 'NONE',  #5534 ) ;
#13001 = CARTESIAN_POINT ( 'NONE',  ( 755.3201227861273992, -387.7255117493283478, 345.3687786644892981 ) ) ;
#13002 = CARTESIAN_POINT ( 'NONE',  ( 763.0428371773158460, -131.4636090269711985, 358.7617431975195359 ) ) ;
#13003 = CARTESIAN_POINT ( 'NONE',  ( 754.9735926884551418, -42.35105083532388193, -340.5236548041000333 ) ) ;
#13004 = CARTESIAN_POINT ( 'NONE',  ( 754.0944755984390895, -63.62377810805107714, 364.1009440267246760 ) ) ;
#13005 = CARTESIAN_POINT ( 'NONE',  ( 794.9819416627830151, -372.9982390220557704, 319.9864689768909898 ) ) ;
#13006 = CARTESIAN_POINT ( 'NONE',  ( 758.8095938919644823, 15.91085188703394593, 311.6929314249762797 ) ) ;
#13007 = LINE ( 'NONE', #34009, #35834 ) ;
#13008 = CARTESIAN_POINT ( 'NONE',  ( 800.2193346964447755, -426.9982390220554862, 355.1360043628815788 ) ) ;
#13009 = ORIENTED_EDGE ( 'NONE', *, *, #39172, .F. ) ;
#13010 = CARTESIAN_POINT ( 'NONE',  ( 765.0180583372156207, -72.99823902205667991, -360.0135310231089534 ) ) ;
#13011 = CARTESIAN_POINT ( 'NONE',  ( 802.7791456095903868, -364.7146871989592114, -329.0155153010375102 ) ) ;
#13013 = CARTESIAN_POINT ( 'NONE',  ( 756.3353852180820240, -197.9073299311472169, 331.1735550268787733 ) ) ;
#13012 = CARTESIAN_POINT ( 'NONE',  ( 803.4237431249931660, -183.1800572038744974, 331.2633955100225194 ) ) ;
#13014 = CARTESIAN_POINT ( 'NONE',  ( 808.7758568127978833, -364.1692326535046504, -320.0363995740631822 ) ) ;
#13015 = DIRECTION ( 'NONE',  ( 0.000000000000000000, 0.3826834323650838421, 0.9238795325112891810 ) ) ;
#13016 = VERTEX_POINT ( 'NONE', #4520 ) ;
#13017 = CARTESIAN_POINT ( 'NONE',  ( 756.3353852180819104, -389.9073299311465348, 331.1735550268788302 ) ) ;
#13018 = ORIENTED_EDGE ( 'NONE', *, *, #18488, .T. ) ;
#13019 = AXIS2_PLACEMENT_3D ( 'NONE', #27685, #34623, #13602 ) ;
#13020 = CARTESIAN_POINT ( 'NONE',  ( 749.2812353651451076, -222.4527844766016642, -323.2262854647983090 ) ) ;
#13021 = CARTESIAN_POINT ( 'NONE',  ( 745.4481719005789273, -123.7255117493292289, 347.5162901302853697 ) ) ;
#13022 = ORIENTED_EDGE ( 'NONE', *, *, #18304, .T. ) ;
#13023 = CARTESIAN_POINT ( 'NONE',  ( 755.3201227861273992, -219.7255117493289447, -345.3687786644892981 ) ) ;
#13024 = ORIENTED_EDGE ( 'NONE', *, *, #28401, .T. ) ;
#13025 = CARTESIAN_POINT ( 'NONE',  ( 771.1735550268778070, -321.1800572038740142, -316.3353852180827630 ) ) ;
#13026 = CARTESIAN_POINT ( 'NONE',  ( 799.2566176426618085, -456.0090635724247932, -324.0069404352559559 ) ) ;
#13027 = CARTESIAN_POINT ( 'NONE',  ( 800.9747183278959710, -252.9982390220560831, 311.9810565676471583 ) ) ;
#13028 = CARTESIAN_POINT ( 'NONE',  ( 790.8726784830453198, -178.7146871989598083, 362.5472867521010585 ) ) ;
#13030 = LINE ( 'NONE', #41211, #24772 ) ;
#13029 = CARTESIAN_POINT ( 'NONE',  ( 809.6099558218720631, -452.9681489794449476, 335.1781210895659342 ) ) ;
#13031 = DIRECTION ( 'NONE',  ( 0.000000000000000000, -1.000000000000000000, 0.000000000000000000 ) ) ;
#13032 = ORIENTED_EDGE ( 'NONE', *, *, #14519, .T. ) ;
#13033 = CARTESIAN_POINT ( 'NONE',  ( 776.9254006560222479, -452.1908817542428665, -314.8983024940802125 ) ) ;
#13034 = PLANE ( 'NONE',  #43205 ) ;
#13035 = DIRECTION ( 'NONE',  ( 0.000000000000000000, 1.000000000000000000, 0.000000000000000000 ) ) ;
#13036 = ORIENTED_EDGE ( 'NONE', *, *, #16452, .F. ) ;
#13037 = CARTESIAN_POINT ( 'NONE',  ( 797.8822607201568644, -222.5545181178800362, -370.1134526219340160 ) ) ;
#13038 = CARTESIAN_POINT ( 'NONE',  ( 812.3518521366052028, -97.09997266333496668, 326.5853460496235243 ) ) ;
#13039 = VECTOR ( 'NONE', #887, 1000.000000000000000 ) ;
#13041 = CARTESIAN_POINT ( 'NONE',  ( 785.3141322388236176, -189.7255117493290300, -364.4286716492789537 ) ) ;
#13040 = CARTESIAN_POINT ( 'NONE',  ( 879.9999999999990905, 479.9999999999998863, -210.0000000000000000 ) ) ;
#13042 = CARTESIAN_POINT ( 'NONE',  ( 805.1016975059191054, -366.8965053807773984, -343.0745993439771837 ) ) ;
#13043 = CARTESIAN_POINT ( 'NONE',  ( 814.4686193811664907, -243.2817908451526705, -346.2056067578752732 ) ) ;
#13044 = DIRECTION ( 'NONE',  ( 0.000000000000000000, 0.000000000000000000, -1.000000000000000000 ) ) ;
#13045 = DIRECTION ( 'NONE',  ( 1.000000000000000000, 0.000000000000000000, 0.000000000000000000 ) ) ;
#13046 = CARTESIAN_POINT ( 'NONE',  ( 761.4292242960306112, -89.46360902697134065, -323.2154366446414429 ) ) ;
#13047 = CIRCLE ( 'NONE', #35926, 8.024999999999948841 ) ;
#13048 = CARTESIAN_POINT ( 'NONE',  ( 783.0745993439762742, -440.1908817542430370, 365.1016975059196739 ) ) ;
#13049 = EDGE_CURVE ( 'NONE', #19541, #12560, #8213, .T. ) ;
#13050 = VECTOR ( 'NONE', #39474, 1000.000000000000000 ) ;
#13051 = CARTESIAN_POINT ( 'NONE',  ( -858.8365100919713768, 240.0000000000002274, -199.9999999999881481 ) ) ;
#13052 = CARTESIAN_POINT ( 'NONE',  ( 770.0799878456142551, -421.9874144716863498, -362.9823548866085616 ) ) ;
#13053 = CARTESIAN_POINT ( 'NONE',  ( 758.8095938919644823, -272.0891481129651197, -311.6929314249762797 ) ) ;
#13054 = CARTESIAN_POINT ( 'NONE',  ( -26.63011601220122060, -512.9681489794448908, -339.9999999999999432 ) ) ;
#13055 = FACE_OUTER_BOUND ( 'NONE', #39289, .T. ) ;
#13056 = CARTESIAN_POINT ( 'NONE',  ( 801.9419747391806368, -42.45278447660223264, -351.9812246680014027 ) ) ;
#13057 = VECTOR ( 'NONE', #7196, 1000.000000000000000 ) ;
#13058 = CARTESIAN_POINT ( 'NONE',  ( 771.3260364891663130, -211.6454272087891582, 306.0683387631859773 ) ) ;
#13059 = CARTESIAN_POINT ( 'NONE',  ( 815.0009284576459549, -150.3510508353235480, -338.7629533639073429 ) ) ;
#13060 = CARTESIAN_POINT ( 'NONE',  ( 812.7932403749906598, -183.1800572038744974, 327.7687537140311633 ) ) ;
#13061 = CARTESIAN_POINT ( 'NONE',  ( 758.8095938919642549, -416.0891481129645513, -311.6929314249763365 ) ) ;
#13062 = AXIS2_PLACEMENT_3D ( 'NONE', #36673, #2004, #13102 ) ;
#13063 = DIRECTION ( 'NONE',  ( 0.000000000000000000, 0.000000000000000000, 1.000000000000000000 ) ) ;
#13064 = CARTESIAN_POINT ( 'NONE',  ( 756.5762568750052424, -267.1800572038742985, 348.7366044899774238 ) ) ;
#13065 = CARTESIAN_POINT ( 'NONE',  ( 776.9254006560222479, -68.19088175424413123, 314.8983024940802125 ) ) ;
#13066 = CARTESIAN_POINT ( 'NONE',  ( 785.3687786644884454, -419.3618753856918033, -315.3201227861279676 ) ) ;
#13067 = PLANE ( 'NONE',  #12168 ) ;
#13068 = DIRECTION ( 'NONE',  ( 0.000000000000000000, 0.000000000000000000, 1.000000000000000000 ) ) ;
#13070 = CARTESIAN_POINT ( 'NONE',  ( 755.0636971347428243, -340.2709662947831362, 341.7834795799807353 ) ) ;
#13069 = CARTESIAN_POINT ( 'NONE',  ( 760.5453621957607311, -93.07832356259645223, 323.8424801807151425 ) ) ;
#13071 = ORIENTED_EDGE ( 'NONE', *, *, #40816, .T. ) ;
#13072 = EDGE_CURVE ( 'NONE', #41197, #36773, #9316, .T. ) ;
#13073 = CARTESIAN_POINT ( 'NONE',  ( 805.0264073115434940, -246.3510508353232638, -339.4763451958999099 ) ) ;
#13074 = CARTESIAN_POINT ( 'NONE',  ( 756.5762568750052424, -123.1800572038747106, -348.7366044899774238 ) ) ;
#13075 = CARTESIAN_POINT ( 'NONE',  ( 792.1044303154645831, -60.45278447660215448, 317.8323909638837677 ) ) ;
#13076 = CARTESIAN_POINT ( 'NONE',  ( 811.6461892240364477, -244.7146871989596093, -324.1737431748509835 ) ) ;
#13077 = DIRECTION ( 'NONE',  ( 1.000000000000000000, -0.000000000000000000, -0.000000000000000000 ) ) ;
#13078 = CARTESIAN_POINT ( 'NONE',  ( 773.7943932421234194, -383.8055962898682765, 305.5313806188329409 ) ) ;
#13079 = EDGE_LOOP ( 'NONE', ( #45225, #12512, #38631, #30076 ) ) ;
#13080 = CIRCLE ( 'NONE', #16773, 2.749999999999919176 ) ;
#13081 = CARTESIAN_POINT ( 'NONE',  ( 804.4286716492782716, -305.3618753856922581, 345.3141322388244703 ) ) ;
#13082 = CARTESIAN_POINT ( 'NONE',  ( 777.4774526936600978, 13.72903370521577138, 304.7301800767027657 ) ) ;
#13083 = CARTESIAN_POINT ( 'NONE',  ( 765.8855110935204493, -22.16923265350575889, -319.0159684113471599 ) ) ;
#13084 = CARTESIAN_POINT ( 'NONE',  ( 788.7366044899766848, -179.9073299311472454, -316.5762568750059813 ) ) ;
#13085 = CARTESIAN_POINT ( 'NONE',  ( 758.0580252608178853, -390.4527844766011526, 328.0187753319985404 ) ) ;
#13086 = EDGE_CURVE ( 'NONE', #37952, #41015, #7091, .T. ) ;
#13087 = CARTESIAN_POINT ( 'NONE',  ( 767.6429770376289525, -105.1800572038747248, -306.8695393053162093 ) ) ;
#13088 = CARTESIAN_POINT ( 'NONE',  ( 797.8594530101009923, -109.5436935675110988, -322.1405469898982119 ) ) ;
#13089 = ORIENTED_EDGE ( 'NONE', *, *, #41855, .F. ) ;
#13090 = CARTESIAN_POINT ( 'NONE',  ( 776.9254006560222479, -44.19088175424421649, -314.8983024940802125 ) ) ;
#13091 = CIRCLE ( 'NONE', #3495, 2.749999999999835687 ) ;
#13092 = CARTESIAN_POINT ( 'NONE',  ( 761.4292242960306112, -353.4636090269705733, -323.2154366446414429 ) ) ;
#13094 = CARTESIAN_POINT ( 'NONE',  ( 772.4468031744293057, -393.8272453906067199, 363.8651313633793620 ) ) ;
#13093 = CARTESIAN_POINT ( 'NONE',  ( 759.7806653035534055, -78.99823902205662307, 324.8639956371180801 ) ) ;
#13097 = CARTESIAN_POINT ( 'NONE',  ( 746.7653713866222915, -353.2601417444137724, 351.0478386215610271 ) ) ;
#13096 = CARTESIAN_POINT ( 'NONE',  ( -26.63011601220122060, -513.1383975375929367, -369.9999999999999432 ) ) ;
#13095 = CARTESIAN_POINT ( 'NONE',  ( 795.1271208383658404, -452.8379544210779954, 371.6178728169206238 ) ) ;
#13098 = CARTESIAN_POINT ( 'NONE',  ( 769.0155153010367712, -370.3726999360613377, -362.7791456095907279 ) ) ;
#13099 = CARTESIAN_POINT ( 'NONE',  ( 788.8264449731200330, -333.1800572038740142, -363.6646147819171233 ) ) ;
#13100 = CARTESIAN_POINT ( 'NONE',  ( 802.2119215644370342, -150.0090635724257027, -367.5423716828165084 ) ) ;
#13101 = CARTESIAN_POINT ( 'NONE',  ( 805.0032342141412300, -445.5436935675098766, 314.9967657858571783 ) ) ;
#13103 = FACE_OUTER_BOUND ( 'NONE', #32616, .T. ) ;
#13102 = DIRECTION ( 'NONE',  ( 0.000000000000000000, 1.110223024625155554E-15, -1.000000000000000000 ) ) ;
#13104 = CARTESIAN_POINT ( 'NONE',  ( 798.7617431975189675, -267.6237781080504305, -323.0428371773161871 ) ) ;
#13105 = EDGE_CURVE ( 'NONE', #25018, #7575, #32934, .T. ) ;
#13106 = CARTESIAN_POINT ( 'NONE',  ( 745.5313806188320314, -111.2817908451530968, -333.7943932421247268 ) ) ;
#13107 = CARTESIAN_POINT ( 'NONE',  ( -190.7583438952258916, 294.6698570112193920, -274.9999999999999432 ) ) ;
#13108 = CARTESIAN_POINT ( 'NONE',  ( 919.9999999999993179, 219.9999999999998863, -350.0000000000000000 ) ) ;
#13109 = CARTESIAN_POINT ( 'NONE',  ( 805.2837595273609850, -314.7363362996979959, 340.5290396650784714 ) ) ;
#13110 = EDGE_CURVE ( 'NONE', #11422, #21201, #12791, .T. ) ;
#13111 = ORIENTED_EDGE ( 'NONE', *, *, #33150, .F. ) ;
#13112 = CARTESIAN_POINT ( 'NONE',  ( 807.2620300519052989, -288.0090635724252479, 318.0141637701419768 ) ) ;
#13113 = CARTESIAN_POINT ( 'NONE',  ( 749.2812353651451076, -174.4527844766018063, -323.2262854647983090 ) ) ;
#13114 = LINE ( 'NONE', #9638, #45250 ) ;
#13115 = CARTESIAN_POINT ( 'NONE',  ( 814.2805881961230625, -97.64542720878949922, 331.2368401574024119 ) ) ;
#13116 = CARTESIAN_POINT ( 'NONE',  ( 796.7737145352015204, -308.6346026584195670, -370.7187646348536987 ) ) ;
#13117 = CARTESIAN_POINT ( 'NONE',  ( 879.9999999999992042, 239.9999999999998295, 210.0000000000000000 ) ) ;
#13118 = CARTESIAN_POINT ( 'NONE',  ( 701.1634899080286232, 259.9999999999999432, -197.2499999999991758 ) ) ;
#13119 = CARTESIAN_POINT ( 'NONE',  ( 758.0580252608178853, -150.4527844766018916, 328.0187753319985404 ) ) ;
#13120 = ORIENTED_EDGE ( 'NONE', *, *, #1836, .F. ) ;
#13121 = CARTESIAN_POINT ( 'NONE',  ( 781.2370466360911223, -428.7363362996975980, 304.9990715423533629 ) ) ;
#13122 = CARTESIAN_POINT ( 'NONE',  ( 791.1614460488616487, -371.2601417444136587, -373.5763878283158874 ) ) ;
#13123 = CIRCLE ( 'NONE', #43357, 2.749999999999835687 ) ;
#13124 = CARTESIAN_POINT ( 'NONE',  ( 792.2312462859673587, -131.9073299311473875, -307.2067596250082602 ) ) ;
#13125 = EDGE_CURVE ( 'NONE', #15909, #3566, #484, .T. ) ;
#13126 = CARTESIAN_POINT ( 'NONE',  ( 799.2566176426618085, -48.00906357242602951, 324.0069404352559559 ) ) ;
#13127 = CARTESIAN_POINT ( 'NONE',  ( 782.5225473063381969, -382.2709662947828519, -375.2698199232970637 ) ) ;
#13128 = DIRECTION ( 'NONE',  ( 0.000000000000000000, 0.000000000000000000, 1.000000000000000000 ) ) ;
#13129 = CARTESIAN_POINT ( 'NONE',  ( 779.4709603349208464, -432.3510508353226669, 314.7162404726379918 ) ) ;
#13130 = ORIENTED_EDGE ( 'NONE', *, *, #1848, .T. ) ;
#13131 = EDGE_CURVE ( 'NONE', #4341, #27855, #26873, .T. ) ;
#13132 = CARTESIAN_POINT ( 'NONE',  ( 744.9990715423526808, -138.3510508353236048, -341.2370466360926002 ) ) ;
#13133 = DIRECTION ( 'NONE',  ( 1.000000000000000000, 0.000000000000000000, 0.000000000000000000 ) ) ;
#13134 = CARTESIAN_POINT ( 'NONE',  ( 783.7566961878529810, -264.8965053807776826, 305.1792804349288417 ) ) ;
#13135 = CARTESIAN_POINT ( 'NONE',  ( 762.1405469898973024, -97.54369356751114140, 357.8594530101016176 ) ) ;
#13136 = VERTEX_POINT ( 'NONE', #2394 ) ;
#13137 = CARTESIAN_POINT ( 'NONE',  ( 804.1601925771018387, -7.441959926233078448, -346.5483106153029098 ) ) ;
#13138 = CARTESIAN_POINT ( 'NONE',  ( 788.7366044899766848, -275.9073299311469896, 316.5762568750059813 ) ) ;
#13139 = ADVANCED_FACE ( 'NONE', ( #2174 ), #4971, .F. ) ;
#13140 = CARTESIAN_POINT ( 'NONE',  ( 804.7487373415286811, -19.54369356751139364, -364.7487373415288516 ) ) ;
#13141 = CARTESIAN_POINT ( 'NONE',  ( 791.1616803454811588, -448.0882476894967112, 368.5954562921680235 ) ) ;
#13142 = VERTEX_POINT ( 'NONE', #37046 ) ;
#13143 = CARTESIAN_POINT ( 'NONE',  ( 809.0717654672305343, -412.9181544815157281, -360.1688906516309885 ) ) ;
#13144 = CARTESIAN_POINT ( 'NONE',  ( 797.8594530101008786, -253.5436935675104735, -322.1405469898980982 ) ) ;
#13146 = CARTESIAN_POINT ( 'NONE',  ( 810.1134526219336749, -248.5328690171414223, 357.8822607201570349 ) ) ;
#13145 = CARTESIAN_POINT ( 'NONE',  ( 782.5225473063383106, -310.2709662947832499, 375.2698199232970637 ) ) ;
#13147 = CARTESIAN_POINT ( 'NONE',  ( 763.0428371773158460, -203.4636090269709996, -358.7617431975195359 ) ) ;
#13148 = CARTESIAN_POINT ( 'NONE',  ( 794.9819416627830151, -204.9982390220562820, -319.9864689768909898 ) ) ;
#13149 = CARTESIAN_POINT ( 'NONE',  ( 774.6312213355098493, -407.3618753856920307, -364.6798772138717482 ) ) ;
#13150 = CARTESIAN_POINT ( 'NONE',  ( 805.1927285166397041, -232.8164208402379245, 341.8018195045277707 ) ) ;
#13151 = ORIENTED_EDGE ( 'NONE', *, *, #1507, .T. ) ;
#13152 = AXIS2_PLACEMENT_3D ( 'NONE', #14253, #18632, #36179 ) ;
#13153 = CARTESIAN_POINT ( 'NONE',  ( 810.7187646348534145, -354.4527844766012095, 356.7737145352016341 ) ) ;
#13154 = CARTESIAN_POINT ( 'NONE',  ( 789.8657795001898876, -452.9681489794449476, -362.9715936389367812 ) ) ;
#13155 = EDGE_CURVE ( 'NONE', #9635, #39962, #21126, .T. ) ;
#13156 = CARTESIAN_POINT ( 'NONE',  ( 812.3518521366052028, -1.099972663335260226, -326.5853460496235243 ) ) ;
#13157 = CARTESIAN_POINT ( 'NONE',  ( 766.8731515446878575, 16.45630643248848912, 318.5849060538806725 ) ) ;
#13158 = CYLINDRICAL_SURFACE ( 'NONE', #32734, 6.119000000000013095 ) ;
#13159 = CARTESIAN_POINT ( 'NONE',  ( 769.9779781133707957, -235.0999726633344835, 316.7813123517150871 ) ) ;
#13160 = CARTESIAN_POINT ( 'NONE',  ( 800.0135310231082713, -86.08914811296573077, 325.0180583372163028 ) ) ;
#13161 = EDGE_LOOP ( 'NONE', ( #18940, #30114, #2853, #15354 ) ) ;
#13162 = CARTESIAN_POINT ( 'NONE',  ( 805.6418435158337843, -461.4636090269701754, -363.8556311672236916 ) ) ;
#13163 = CARTESIAN_POINT ( 'NONE',  ( 815.2698199232962679, -64.81642084023852135, -342.5225473063383674 ) ) ;
#13164 = CARTESIAN_POINT ( 'NONE',  ( 779.4709603349208464, -240.3510508353232069, 314.7162404726379918 ) ) ;
#13165 = CARTESIAN_POINT ( 'NONE',  ( 785.3687786644884454, -443.3618753856917465, -315.3201227861279676 ) ) ;
#13166 = CARTESIAN_POINT ( 'NONE',  ( 758.0580252608178853, -30.45278447660226817, -328.0187753319985404 ) ) ;
#13167 = CARTESIAN_POINT ( 'NONE',  ( 814.2805881961230625, -1.645427208789804308, 331.2368401574024119 ) ) ;
#13168 = CARTESIAN_POINT ( 'NONE',  ( 804.6798772138708955, 8.274488250670337663, -334.6312213355107019 ) ) ;
#13169 = CARTESIAN_POINT ( 'NONE',  ( 766.0291762391763086, -298.9181544815161828, -360.7704444035551319 ) ) ;
#13170 = CARTESIAN_POINT ( 'NONE',  ( 759.0252816721024374, -216.9982390220562252, -368.0189434323527280 ) ) ;
#13171 = CARTESIAN_POINT ( 'NONE',  ( 748.9653473494363425, -98.63460265842024910, 356.9462024416521331 ) ) ;
#13172 = CARTESIAN_POINT ( 'NONE',  ( 815.2698199232961542, -160.8164208402382371, 342.5225473063383106 ) ) ;
#13173 = PLANE ( 'NONE',  #32865 ) ;
#13174 = FILL_AREA_STYLE_COLOUR ( '', #17317 ) ;
#13175 = CARTESIAN_POINT ( 'NONE',  ( 812.6845335610512393, -247.9874144716867761, -353.5525998758768651 ) ) ;
#13176 = EDGE_CURVE ( 'NONE', #35738, #35219, #44678, .T. ) ;
#13177 = CARTESIAN_POINT ( 'NONE',  ( 809.0717654672305343, -412.9181544815157281, 360.1688906516309885 ) ) ;
#13178 = CARTESIAN_POINT ( 'NONE',  ( 810.7187646348534145, -282.4527844766014937, -356.7737145352016341 ) ) ;
#13179 = DIRECTION ( 'NONE',  ( 0.000000000000000000, -1.000000000000000000, 0.000000000000000000 ) ) ;
#13180 = CARTESIAN_POINT ( 'NONE',  ( 748.9653473494363425, -386.6346026584191691, 356.9462024416521331 ) ) ;
#13181 = CARTESIAN_POINT ( 'NONE',  ( 763.2262854647970016, -8.634602658420517329, 309.2812353651462445 ) ) ;
#13182 = CARTESIAN_POINT ( 'NONE',  ( 755.5713283507202505, -341.3618753856922012, -334.6858677611754729 ) ) ;
#13183 = EDGE_CURVE ( 'NONE', #26065, #11266, #19963, .T. ) ;
#13184 = CARTESIAN_POINT ( 'NONE',  ( 795.9930595647434757, -3.078323562596726681, 320.7433823573372820 ) ) ;
#13185 = CARTESIAN_POINT ( 'NONE',  ( 746.0683387631852383, -67.44195992623289726, -331.3260364891676204 ) ) ;
#13186 = CARTESIAN_POINT ( 'NONE',  ( 802.7791456095903868, -148.7146871989598935, -329.0155153010375102 ) ) ;
#13187 = CARTESIAN_POINT ( 'NONE',  ( 791.1614460488616487, -179.2601417444143692, 373.5763878283158874 ) ) ;
#13188 = CARTESIAN_POINT ( 'NONE',  ( 768.0187753319979720, 15.36539734157940629, 318.0580252608186242 ) ) ;
#13189 = CARTESIAN_POINT ( 'NONE',  ( 786.2056067578752163, -179.8055962898688733, 374.4686193811670023 ) ) ;
#13190 = ORIENTED_EDGE ( 'NONE', *, *, #14278, .T. ) ;
#13191 = CARTESIAN_POINT ( 'NONE',  ( 804.9363028652555840, -64.27096629478397460, -338.2165204200192079 ) ) ;
#13192 = CARTESIAN_POINT ( 'NONE',  ( 800.7704444035546203, -172.1692326535052757, -326.0291762391768771 ) ) ;
#13193 = EDGE_CURVE ( 'NONE', #17901, #29615, #40983, .T. ) ;
#13194 = CARTESIAN_POINT ( 'NONE',  ( 755.3201227861273992, -147.7255117493291152, 345.3687786644892981 ) ) ;
#13195 = CARTESIAN_POINT ( 'NONE',  ( 807.5423716828161105, -9.078323562596708030, -362.2119215644372048 ) ) ;
#13196 = PRODUCT_DEFINITION ( 'UNKNOWN', '', #37863, #27486 ) ;
#13198 = CARTESIAN_POINT ( 'NONE',  ( 794.9819416627830151, -300.9982390220559409, 319.9864689768909898 ) ) ;
#13197 = CARTESIAN_POINT ( 'NONE',  ( 805.1927285166397041, -280.8164208402378677, 341.8018195045277707 ) ) ;
#13199 = PLANE ( 'NONE',  #35233 ) ;
#13200 = EDGE_LOOP ( 'NONE', ( #32735, #2429, #33922, #15494 ) ) ;
#13201 = CARTESIAN_POINT ( 'NONE',  ( 802.7791456095903868, -4.714687198960358039, 329.0155153010375102 ) ) ;
#13202 = CARTESIAN_POINT ( 'NONE',  ( 783.7953271457878373, -296.1908817542434917, -375.1787889125761239 ) ) ;
#13203 = APPLICATION_PROTOCOL_DEFINITION ( 'draft international standard', 'automotive_design', 1998, #22838 ) ;
#13204 = CARTESIAN_POINT ( 'NONE',  ( 813.1304606946831655, -209.9073299311471317, 352.3570229623691716 ) ) ;
#13205 = CARTESIAN_POINT ( 'NONE',  ( 776.9254006560222479, -332.1908817542433781, 314.8983024940802125 ) ) ;
#13206 = CARTESIAN_POINT ( 'NONE',  ( 805.0264073115434940, -438.3510508353226669, 339.4763451958999099 ) ) ;
#13207 = ORIENTED_EDGE ( 'NONE', *, *, #19682, .F. ) ;
#13208 = CARTESIAN_POINT ( 'NONE',  ( 759.0159684113467620, -112.9181544815167229, -325.8855110935213020 ) ) ;
#13209 = CARTESIAN_POINT ( 'NONE',  ( 802.1676090361156639, -110.6346026584201638, -327.8955696845344505 ) ) ;
#13210 = CARTESIAN_POINT ( 'NONE',  ( 802.1676090361155502, -302.6346026584195670, -327.8955696845344505 ) ) ;
#13211 = EDGE_LOOP ( 'NONE', ( #18034, #33343 ) ) ;
#13212 = CARTESIAN_POINT ( 'NONE',  ( 792.1044303154645831, -444.4527844766009821, -317.8323909638837677 ) ) ;
#13213 = CARTESIAN_POINT ( 'NONE',  ( 754.8983024940795303, -282.8965053807776258, 336.9254006560228163 ) ) ;
#13214 = LINE ( 'NONE', #39017, #43282 ) ;
#13215 = LINE ( 'NONE', #20124, #7160 ) ;
#13216 = CARTESIAN_POINT ( 'NONE',  ( 769.0155153010367712, -130.3726999360621619, 362.7791456095907279 ) ) ;
#13217 = CARTESIAN_POINT ( 'NONE',  ( 805.1927285166397041, 7.183579159761247723, 341.8018195045277707 ) ) ;
#13218 = ORIENTED_EDGE ( 'NONE', *, *, #36564, .F. ) ;
#13219 = CARTESIAN_POINT ( 'NONE',  ( 757.7880784355613741, -330.0090635724251342, -312.4576283171834916 ) ) ;
#13220 = CARTESIAN_POINT ( 'NONE',  ( 814.8207195650702488, -218.1908817542437191, 336.2433038121456548 ) ) ;
#13221 = AXIS2_PLACEMENT_3D ( 'NONE', #11352, #32603, #29374 ) ;
#13222 = CARTESIAN_POINT ( 'NONE',  ( 767.8955696845333705, -312.4527844766012663, -362.1676090361162323 ) ) ;
#13223 =( NAMED_UNIT ( * ) SI_UNIT ( $, .STERADIAN. ) SOLID_ANGLE_UNIT ( ) );
#13224 = CARTESIAN_POINT ( 'NONE',  ( 796.1575198192839480, -174.0090635724256742, -359.4546378042384163 ) ) ;
#13225 = CARTESIAN_POINT ( 'NONE',  ( 745.7998596910086917, -53.36187538569310362, 332.5602148656461168 ) ) ;
#13226 = CARTESIAN_POINT ( 'NONE',  ( 795.1526350630804245, -452.9681489794450044, 359.9976132353968410 ) ) ;
#13227 = CARTESIAN_POINT ( 'NONE',  ( 758.8095938919644823, -368.0891481129647786, -311.6929314249762797 ) ) ;
#13228 = PLANE ( 'NONE',  #342 ) ;
#13229 = CARTESIAN_POINT ( 'NONE',  ( 793.5525998758768083, -319.0999726633342561, 372.6845335610516941 ) ) ;
#13230 = DIRECTION ( 'NONE',  ( 1.000000000000000000, 0.000000000000000000, 0.000000000000000000 ) ) ;
#13231 = CARTESIAN_POINT ( 'NONE',  ( 749.2812353651451076, -294.4527844766013800, 323.2262854647983090 ) ) ;
#13232 = CARTESIAN_POINT ( 'NONE',  ( 744.7301800767019131, -28.81642084023863148, -337.4774526936615757 ) ) ;
#13233 = CARTESIAN_POINT ( 'NONE',  ( 758.0580252608178853, -246.4527844766016074, -328.0187753319985404 ) ) ;
#13234 = LINE ( 'NONE', #9066, #34288 ) ;
#13235 = CARTESIAN_POINT ( 'NONE',  ( 802.1676090361156639, -398.6346026584193396, 327.8955696845344505 ) ) ;
#13236 = CARTESIAN_POINT ( 'NONE',  ( 790.9844846989617508, -166.3726999360620198, 317.2208543904092721 ) ) ;
#13237 = CARTESIAN_POINT ( 'NONE',  ( 798.7617431975189675, -51.62377810805111267, -323.0428371773161871 ) ) ;
#13238 = CARTESIAN_POINT ( 'NONE',  ( 751.2241431872005251, -64.16923265350563099, 359.9636004259367610 ) ) ;
#13239 = CARTESIAN_POINT ( 'NONE',  ( 759.7806653035535192, -366.9982390220557136, 324.8639956371181370 ) ) ;
#13240 = CARTESIAN_POINT ( 'NONE',  ( 701.1634899080286232, 259.9999999999999432, -206.1189999999990334 ) ) ;
#13241 = FILL_AREA_STYLE_COLOUR ( '', #42462 ) ;
#13242 = CARTESIAN_POINT ( 'NONE',  ( 795.1360043628807261, -428.0891481129644944, 360.2193346964456282 ) ) ;
#13243 = ORIENTED_EDGE ( 'NONE', *, *, #4401, .T. ) ;
#13244 = CARTESIAN_POINT ( 'NONE',  ( 755.3201227861273992, -51.72551174932946338, -345.3687786644892981 ) ) ;
#13245 = CARTESIAN_POINT ( 'NONE',  ( 766.7756240680305382, -374.5328690171410813, -361.5560724626415663 ) ) ;
#13247 = CARTESIAN_POINT ( 'NONE',  ( 774.6858677611749044, -201.7255117493290015, 315.5713283507209894 ) ) ;
#13246 = CARTESIAN_POINT ( 'NONE',  ( 788.7366044899766848, -203.9073299311471885, 316.5762568750059813 ) ) ;
#13248 = CARTESIAN_POINT ( 'NONE',  ( 810.1134526219336749, -368.5328690171409676, -357.8822607201570349 ) ) ;
#13249 = CARTESIAN_POINT ( 'NONE',  ( 998.9999999999992042, 248.9999999999998863, 360.0000000000000000 ) ) ;
#13250 = ORIENTED_EDGE ( 'NONE', *, *, #17953, .F. ) ;
#13251 = CARTESIAN_POINT ( 'NONE',  ( 778.2165204200184689, -382.8164208402374697, 364.9363028652563230 ) ) ;
#13252 = AXIS2_PLACEMENT_3D ( 'NONE', #1099, #9098, #43586 ) ;
#13253 = VERTEX_POINT ( 'NONE', #30344 ) ;
#13254 = CARTESIAN_POINT ( 'NONE',  ( 772.5602148656447525, -225.7255117493289163, -305.7998596910095443 ) ) ;
#13255 = CARTESIAN_POINT ( 'NONE',  ( 751.6929314249750860, -102.9982390220565662, 318.8095938919659034 ) ) ;
#13256 = ORIENTED_EDGE ( 'NONE', *, *, #37668, .F. ) ;
#13257 = CARTESIAN_POINT ( 'NONE',  ( 754.8072714833583632, -220.8164208402380098, -338.1981804954721156 ) ) ;
#13258 = ORIENTED_EDGE ( 'NONE', *, *, #30571, .T. ) ;
#13259 = CARTESIAN_POINT ( 'NONE',  ( 765.0180583372156207, -336.9982390220558273, -360.0135310231089534 ) ) ;
#13260 = CARTESIAN_POINT ( 'NONE',  ( 771.1735550268778070, 14.81994279612486309, -316.3353852180827630 ) ) ;
#13261 = CARTESIAN_POINT ( 'NONE',  ( 775.9200461376533440, -191.8055962898689017, 315.3028492785443291 ) ) ;
#13263 = DIRECTION ( 'NONE',  ( 0.000000000000000000, 0.000000000000000000, -1.000000000000000000 ) ) ;
#13262 = DIRECTION ( 'NONE',  ( 0.000000000000000000, 0.000000000000000000, 1.000000000000000000 ) ) ;
#13264 = DIRECTION ( 'NONE',  ( -1.000000000000000000, -0.000000000000000000, -0.000000000000000000 ) ) ;
#13265 = VERTEX_POINT ( 'NONE', #9101 ) ;
#13266 = CARTESIAN_POINT ( 'NONE',  ( 788.7366044899766848, 12.09267006885214180, -316.5762568750059813 ) ) ;
#13267 = CARTESIAN_POINT ( 'NONE',  ( 779.9999999999992042, -462.9681489794448339, 339.9999999999999432 ) ) ;
#13268 = CARTESIAN_POINT ( 'NONE',  ( 799.9999999999993179, 166.4563064324884465, 319.9999999999999432 ) ) ;
#13269 = CARTESIAN_POINT ( 'NONE',  ( 747.6481478633932056, -253.0999726633345119, -353.4146539503763620 ) ) ;
#13270 = CARTESIAN_POINT ( 'NONE',  ( 762.1177392798416577, -90.55451811788041994, 309.8865473780659272 ) ) ;
#13272 = CARTESIAN_POINT ( 'NONE',  ( 800.0135310231082713, -230.0891481129652618, -325.0180583372163028 ) ) ;
#13271 = LINE ( 'NONE', #3091, #40843 ) ;
#13273 = CARTESIAN_POINT ( 'NONE',  ( 780.5290396650775619, -348.3510508353228943, -365.2837595273619513 ) ) ;
#13274 = CARTESIAN_POINT ( 'NONE',  ( 745.7194118038753459, -253.6454272087889876, -348.7631598425976449 ) ) ;
#13275 = DIRECTION ( 'NONE',  ( -0.000000000000000000, 1.000000000000000000, -0.000000000000000000 ) ) ;
#13276 = CARTESIAN_POINT ( 'NONE',  ( 939.9999999999992042, 50.81038600091411439, 217.3872392842761769 ) ) ;
#13277 = CARTESIAN_POINT ( 'NONE',  ( 773.4516893846965786, -91.64542720878951343, -315.8398074228977066 ) ) ;
#13278 = CARTESIAN_POINT ( 'NONE',  ( 769.0155153010367712, -442.3726999360611103, 362.7791456095907279 ) ) ;
#13279 = DIRECTION ( 'NONE',  ( 0.000000000000000000, 0.000000000000000000, -1.000000000000000000 ) ) ;
#13280 = CARTESIAN_POINT ( 'NONE',  ( 754.9735926884551418, -426.3510508353226669, -340.5236548041000333 ) ) ;
#13281 = CARTESIAN_POINT ( 'NONE',  ( 772.5602148656447525, -273.7255117493288026, -305.7998596910095443 ) ) ;
#13282 = DIRECTION ( 'NONE',  ( -0.000000000000000000, 1.000000000000000000, -0.000000000000000000 ) ) ;
#13283 = DIRECTION ( 'NONE',  ( -1.880165489482579047E-16, -1.000000000000000000, 0.000000000000000000 ) ) ;
#13284 = CARTESIAN_POINT ( 'NONE',  ( 785.3687786644884454, -59.36187538569306810, -315.3201227861279676 ) ) ;
#13285 = CARTESIAN_POINT ( 'NONE',  ( 764.1737431748507561, -226.3726999360617924, 371.6461892240376415 ) ) ;
#13286 = CARTESIAN_POINT ( 'NONE',  ( 776.2433038121456548, -180.8965053807779952, -374.8207195650711014 ) ) ;
#13287 = CARTESIAN_POINT ( 'NONE',  ( 767.6429770376289525, -201.1800572038744690, 306.8695393053162093 ) ) ;
#13288 = CARTESIAN_POINT ( 'NONE',  ( 772.5602148656447525, -417.7255117493283478, -305.7998596910095443 ) ) ;
#13289 = CARTESIAN_POINT ( 'NONE',  ( 998.9999999999992042, 248.9999999999998863, -360.0000000000000000 ) ) ;
#13290 = CARTESIAN_POINT ( 'NONE',  ( 768.0187753319979720, -272.6346026584196807, 318.0580252608186242 ) ) ;
#13291 = EDGE_CURVE ( 'NONE', #32281, #28399, #33153, .T. ) ;
#13292 = CARTESIAN_POINT ( 'NONE',  ( 801.5560724626406000, -72.55451811788049099, 326.7756240680316182 ) ) ;
#13293 = CARTESIAN_POINT ( 'NONE',  ( 756.3353852180819104, -413.9073299311465348, -331.1735550268788302 ) ) ;
#13294 = PLANE ( 'NONE',  #12203 ) ;
#13295 = CARTESIAN_POINT ( 'NONE',  ( 831.1634899080286232, 256.4999999999998863, -199.9999999999999432 ) ) ;
#13297 = CARTESIAN_POINT ( 'NONE',  ( 774.6312213355099630, -311.3618753856922581, 364.6798772138717482 ) ) ;
#13296 = CARTESIAN_POINT ( 'NONE',  ( 772.3691319403857278, -95.26014174441461080, 315.8894580844506663 ) ) ;
#13298 = VERTEX_POINT ( 'NONE', #15807 ) ;
#13299 = CARTESIAN_POINT ( 'NONE',  ( 776.9566956441375396, -276.8965053807776258, -364.8461984189686405 ) ) ;
#13300 = CARTESIAN_POINT ( 'NONE',  ( 785.3687786644884454, -131.3618753856928834, -315.3201227861279676 ) ) ;
#13301 = CARTESIAN_POINT ( 'NONE',  ( 785.3141322388236176, -45.72551174932949181, 364.4286716492789537 ) ) ;
#13302 = CARTESIAN_POINT ( 'NONE',  ( 764.3348316497523456, -262.7146871989594956, -308.6759233522265617 ) ) ;
#13303 = CARTESIAN_POINT ( 'NONE',  ( 181.1634899080285948, 230.0000000000000000, -199.9999999999953957 ) ) ;
#13304 = CARTESIAN_POINT ( 'NONE',  ( 795.6651683502461765, -394.7146871989591546, 371.3240766477733814 ) ) ;
#13305 = ORIENTED_EDGE ( 'NONE', *, *, #711, .T. ) ;
#13306 = CARTESIAN_POINT ( 'NONE',  ( 755.0636971347428243, -292.2709662947831930, 341.7834795799807353 ) ) ;
#13307 = CARTESIAN_POINT ( 'NONE',  ( 800.7704444035546203, -28.16923265350574468, -326.0291762391768771 ) ) ;
#13308 = CARTESIAN_POINT ( 'NONE',  ( 791.9812246680005501, -164.6346026584200217, -361.9419747391813189 ) ) ;
#13309 = CARTESIAN_POINT ( 'NONE',  ( 774.6312213355099630, -359.3618753856920875, 364.6798772138717482 ) ) ;
#13310 = CARTESIAN_POINT ( 'NONE',  ( 745.7998596910086917, -101.3618753856929544, -332.5602148656461168 ) ) ;
#13311 = EDGE_CURVE ( 'NONE', #34024, #22852, #31473, .T. ) ;
#13312 = CARTESIAN_POINT ( 'NONE',  ( 785.3141322388236176, -117.7255117493292715, -364.4286716492789537 ) ) ;
#13313 = EDGE_LOOP ( 'NONE', ( #21092, #22725 ) ) ;
#13314 = CARTESIAN_POINT ( 'NONE',  ( 759.0159684113467620, -40.91815448151695023, -325.8855110935213020 ) ) ;
#13315 = CARTESIAN_POINT ( 'NONE',  ( 766.0291762391763086, -370.9181544815159555, -360.7704444035551319 ) ) ;
#13317 = CARTESIAN_POINT ( 'NONE',  ( 796.1575198192839480, -414.0090635724249637, 359.4546378042384163 ) ) ;
#13316 = CARTESIAN_POINT ( 'NONE',  ( 778.1981804954714335, -106.2709662947838467, 314.8072714833589885 ) ) ;
#13318 = CARTESIAN_POINT ( 'NONE',  ( 804.9511171171677688, -101.8055962898691718, 335.8780910478229202 ) ) ;
#13321 = CARTESIAN_POINT ( 'NONE',  ( 812.6845335610512393, -367.9874144716865203, 353.5525998758768651 ) ) ;
#13320 = LINE ( 'NONE', #20685, #9285 ) ;
#13319 = LINE ( 'NONE', #41266, #21102 ) ;
#13322 = CARTESIAN_POINT ( 'NONE',  ( 757.4527132478984868, -352.3726999360614514, -329.1273215169538844 ) ) ;
#13323 = CARTESIAN_POINT ( 'NONE',  ( 788.7366044899766848, -371.9073299311465917, -316.5762568750059813 ) ) ;
#13324 = CARTESIAN_POINT ( 'NONE',  ( 805.6418435158337843, -125.4636090269712412, -363.8556311672236916 ) ) ;
#13325 = CARTESIAN_POINT ( 'NONE',  ( 811.0346526505616112, -446.6346026584189985, 323.0537975583477532 ) ) ;
#13327 = DIRECTION ( 'NONE',  ( -1.000000000000000000, 0.000000000000000000, 0.000000000000000000 ) ) ;
#13326 = DIRECTION ( 'NONE',  ( 0.000000000000000000, 0.000000000000000000, 1.000000000000000000 ) ) ;
#13328 = CARTESIAN_POINT ( 'NONE',  ( 747.6481478633932056, -157.0999726633347962, -353.4146539503763620 ) ) ;
#13329 = LINE ( 'NONE', #44279, #520 ) ;
#13330 = DIRECTION ( 'NONE',  ( -1.000000000000000000, 0.000000000000000000, -0.000000000000000000 ) ) ;
#13331 = CARTESIAN_POINT ( 'NONE',  ( 783.0745993439762742, -344.1908817542433212, 365.1016975059196739 ) ) ;
#13332 = EDGE_LOOP ( 'NONE', ( #7533, #14567, #8402, #35438 ) ) ;
#13333 = CARTESIAN_POINT ( 'NONE',  ( 814.4686193811664907, -315.2817908451525000, 346.2056067578752732 ) ) ;
#13334 = CARTESIAN_POINT ( 'NONE',  ( 767.6429770376291799, -177.1800572038744974, -306.8695393053162093 ) ) ;
#13335 = EDGE_CURVE ( 'NONE', #36781, #2171, #11570, .T. ) ;
#13336 = DIRECTION ( 'NONE',  ( -1.880165489482579047E-16, -1.000000000000000000, -0.000000000000000000 ) ) ;
#13337 = CARTESIAN_POINT ( 'NONE',  ( 797.8822607201568644, -126.5545181178803205, 370.1134526219340160 ) ) ;
#13338 = CARTESIAN_POINT ( 'NONE',  ( 810.7187646348534145, -306.4527844766013800, -356.7737145352016341 ) ) ;
#13339 = EDGE_CURVE ( 'NONE', #35556, #37602, #32944, .T. ) ;
#13340 = CARTESIAN_POINT ( 'NONE',  ( 190.7583438952258916, 294.6698570112193920, -244.9999999999999716 ) ) ;
#13341 = PRODUCT_DEFINITION_SHAPE ( 'NONE', 'NONE',  #45735 ) ;
#13342 = DIRECTION ( 'NONE',  ( 0.000000000000000000, 0.000000000000000000, 1.000000000000000000 ) ) ;
#13343 = CARTESIAN_POINT ( 'NONE',  ( 765.0180583372156207, -192.9982390220562820, 360.0135310231089534 ) ) ;
#13344 = EDGE_LOOP ( 'NONE', ( #25228, #25600, #12000, #16372 ) ) ;
#13345 = CARTESIAN_POINT ( 'NONE',  ( 814.2805881961230625, -433.6454272087884760, 331.2368401574024119 ) ) ;
#13346 = CARTESIAN_POINT ( 'NONE',  ( 795.6651683502461765, -370.7146871989592114, -371.3240766477733814 ) ) ;
#13347 = CARTESIAN_POINT ( 'NONE',  ( 812.7932403749906598, -111.1800572038747532, -327.7687537140311633 ) ) ;
#13348 = CARTESIAN_POINT ( 'NONE',  ( 757.4527132478984868, -40.37269993606240348, 329.1273215169538844 ) ) ;
#13349 = CARTESIAN_POINT ( 'NONE',  ( 772.5602148656447525, -369.7255117493284615, -305.7998596910095443 ) ) ;
#13350 = CARTESIAN_POINT ( 'NONE',  ( 794.9999999999993179, 239.9999999999998863, -235.0000000000000000 ) ) ;
#13351 = CARTESIAN_POINT ( 'NONE',  ( 757.2208543904082489, -424.7146871989589840, 350.9844846989624330 ) ) ;
#13352 = VERTEX_POINT ( 'NONE', #5639 ) ;
#13353 = CARTESIAN_POINT ( 'NONE',  ( 798.0661480581538854, -146.5328690171417350, -309.5768839229118043 ) ) ;
#13354 = CARTESIAN_POINT ( 'NONE',  ( -746.4999999999993179, -365.3551492539851893, -18.13243251470705886 ) ) ;
#13355 = CARTESIAN_POINT ( 'NONE',  ( 813.2346286133761168, -269.2601417444139997, 328.9521613784389160 ) ) ;
#13356 = CARTESIAN_POINT ( 'NONE',  ( 759.9864689768902508, -74.08914811296577341, 354.9819416627836404 ) ) ;
#13357 = ORIENTED_EDGE ( 'NONE', *, *, #26058, .T. ) ;
#13358 = CARTESIAN_POINT ( 'NONE',  ( 789.9200121543843807, -1.987414471687640294, -317.0176451133914384 ) ) ;
#13359 = CARTESIAN_POINT ( 'NONE',  ( 759.7806653035534055, -270.9982390220561115, 324.8639956371180801 ) ) ;
#13360 = CARTESIAN_POINT ( 'NONE',  ( 814.5518280994195948, 8.274488250670337663, -332.4837098697145734 ) ) ;
#13361 = CYLINDRICAL_SURFACE ( 'NONE', #32775, 30.00000000000008171 ) ;
#13362 = ORIENTED_EDGE ( 'NONE', *, *, #15926, .T. ) ;
#13363 = VERTEX_POINT ( 'NONE', #15588 ) ;
#13364 = ADVANCED_BREP_SHAPE_REPRESENTATION ( '', ( #2718, #26858 ), #32791 ) ;
#13365 = CARTESIAN_POINT ( 'NONE',  ( 771.3260364891663130, -403.6454272087884760, -306.0683387631859773 ) ) ;
#13366 = CARTESIAN_POINT ( 'NONE',  ( 792.1044303154645831, -300.4527844766012663, 317.8323909638837677 ) ) ;
#13367 = CARTESIAN_POINT ( 'NONE',  ( 771.2633955100217236, -263.9073299311469327, -363.4237431249939618 ) ) ;
#13369 = CARTESIAN_POINT ( 'NONE',  ( 812.6845335610512393, -247.9874144716867761, 353.5525998758768651 ) ) ;
#13368 = CARTESIAN_POINT ( 'NONE',  ( 763.2262854647970016, -344.6346026584195101, 309.2812353651462445 ) ) ;
#13370 = CARTESIAN_POINT ( 'NONE',  ( 811.6461892240364477, -52.71468719896020616, 324.1737431748509835 ) ) ;
#13371 = CARTESIAN_POINT ( 'NONE',  ( 793.9708237608222134, -238.9181544815163534, -319.2295555964448681 ) ) ;
#13372 = CARTESIAN_POINT ( 'NONE',  ( 759.9864689768902508, -218.0891481129653187, -354.9819416627836404 ) ) ;
#13373 = CARTESIAN_POINT ( 'NONE',  ( 767.8955696845334842, -432.4527844766009252, -362.1676090361161755 ) ) ;
#13374 = CARTESIAN_POINT ( 'NONE',  ( 804.4286716492782716, -233.3618753856925423, 345.3141322388244703 ) ) ;
#13375 = VERTEX_POINT ( 'NONE', #40322 ) ;
#13376 = CARTESIAN_POINT ( 'NONE',  ( 763.2262854647970016, -344.6346026584195101, 309.2812353651462445 ) ) ;
#13377 = LINE ( 'NONE', #10829, #5623 ) ;
#13378 = CARTESIAN_POINT ( 'NONE',  ( 814.4686193811664907, -51.28179084515328867, -346.2056067578752732 ) ) ;
#13379 = CARTESIAN_POINT ( 'NONE',  ( 764.4978033197144214, 16.45630643248849267, 320.3127214678681867 ) ) ;
#13380 = DIRECTION ( 'NONE',  ( -0.000000000000000000, -0.000000000000000000, -1.000000000000000000 ) ) ;
#13381 = ADVANCED_FACE ( 'NONE', ( #26435 ), #8675, .F. ) ;
#13382 = CARTESIAN_POINT ( 'NONE',  ( 804.1105419155481968, -243.8272453906072030, 347.6308680596136469 ) ) ;
#13383 = CARTESIAN_POINT ( 'NONE',  ( 778.2165204200184689, -118.8164208402383508, 364.9363028652563230 ) ) ;
#13384 = ORIENTED_EDGE ( 'NONE', *, *, #5499, .T. ) ;
#13385 = CARTESIAN_POINT ( 'NONE',  ( 769.0155153010367712, -10.37269993606250473, -362.7791456095907279 ) ) ;
#13386 = AXIS2_PLACEMENT_3D ( 'NONE', #43265, #10956, #22022 ) ;
#13387 = CARTESIAN_POINT ( 'NONE',  ( 787.5162901302840055, -59.36187538569307520, -305.4481719005793252 ) ) ;
#13388 = CARTESIAN_POINT ( 'NONE',  ( 760.5453621957607311, -285.0783235625958127, 323.8424801807151425 ) ) ;
#13389 = CARTESIAN_POINT ( 'NONE',  ( 762.3223304703356007, -439.5436935675101040, -322.3223304703362828 ) ) ;
#13390 = CARTESIAN_POINT ( 'NONE',  ( 797.6776695296629214, -43.54369356751131903, -357.6776695296636603 ) ) ;
#13391 = CARTESIAN_POINT ( 'NONE',  ( 766.4474001241216001, 4.900027336664720679, 307.3154664389482491 ) ) ;
#13392 = ADVANCED_FACE ( 'NONE', ( #5185 ), #19271, .F. ) ;
#13393 = CARTESIAN_POINT ( 'NONE',  ( 745.7998596910086917, -197.3618753856926560, -332.5602148656461168 ) ) ;
#13394 = EDGE_CURVE ( 'NONE', #13265, #17501, #23412, .T. ) ;
#13395 = CARTESIAN_POINT ( 'NONE',  ( 810.7187646348534145, -90.45278447660209054, 356.7737145352016341 ) ) ;
#13396 = CARTESIAN_POINT ( 'NONE',  ( 777.5031285880264704, -190.8164208402381234, 374.9108240113588408 ) ) ;
#13397 = CARTESIAN_POINT ( 'NONE',  ( 772.4999999999993179, -512.9681489794448908, -370.0000000000000000 ) ) ;
#13398 = FACE_OUTER_BOUND ( 'NONE', #5949, .T. ) ;
#13399 = CARTESIAN_POINT ( 'NONE',  ( 805.9055244015594326, -267.6237781080504305, -315.8990559732753240 ) ) ;
#13400 = CARTESIAN_POINT ( 'NONE',  ( 811.3240766477731540, -412.3726999360612808, 355.6651683502462902 ) ) ;
#13401 = CARTESIAN_POINT ( 'NONE',  ( 751.9810565676468741, -266.0891481129651197, -360.9747183278973921 ) ) ;
#13402 = PLANE ( 'NONE',  #9520 ) ;
#13403 = CARTESIAN_POINT ( 'NONE',  ( 805.0032342141412300, -397.5436935675100472, 314.9967657858571783 ) ) ;
#13404 = CARTESIAN_POINT ( 'NONE',  ( 754.9967657858570647, -25.54369356751137232, 365.0032342141425943 ) ) ;
#13405 = CARTESIAN_POINT ( 'NONE',  ( 774.6312213355099630, -335.3618753856920307, -364.6798772138717482 ) ) ;
#13406 = CARTESIAN_POINT ( 'NONE',  ( 773.3843516231979720, -13.44195992623305713, 364.4086373105754433 ) ) ;
#13407 = CARTESIAN_POINT ( 'NONE',  ( 805.9055244015594326, -51.62377810805111267, -315.8990559732753240 ) ) ;
#13408 = CARTESIAN_POINT ( 'NONE',  ( 805.1016975059191054, -150.8965053807781089, -343.0745993439771837 ) ) ;
#13409 = EDGE_CURVE ( 'NONE', #22607, #42507, #37280, .T. ) ;
#13410 = CARTESIAN_POINT ( 'NONE',  ( 803.8556311672234642, -177.6237781080507148, 365.6418435158340117 ) ) ;
#13411 = CARTESIAN_POINT ( 'NONE',  ( 803.6646147819162707, 6.092670068852160448, 348.8264449731211130 ) ) ;
#13412 = EDGE_CURVE ( 'NONE', #8421, #32576, #18929, .T. ) ;
#13413 = CARTESIAN_POINT ( 'NONE',  ( 815.1787889125755555, -174.8965053807779952, 343.7953271457877804 ) ) ;
#13414 = ORIENTED_EDGE ( 'NONE', *, *, #35683, .F. ) ;
#13415 = CARTESIAN_POINT ( 'NONE',  ( 755.3201227861273992, -75.72551174932937101, -345.3687786644892981 ) ) ;
#13416 = CARTESIAN_POINT ( 'NONE',  ( 803.8651313633788504, -173.2601417444143692, -332.4468031744301015 ) ) ;
#13417 = CARTESIAN_POINT ( 'NONE',  ( 785.3687786644884454, -155.3618753856927128, 315.3201227861279676 ) ) ;
#13418 = CARTESIAN_POINT ( 'NONE',  ( 773.7943932421234194, 0.1944037101305369775, -305.5313806188329409 ) ) ;
#13419 = CARTESIAN_POINT ( 'NONE',  ( 785.3687786644885591, -299.3618753856923149, 315.3201227861280813 ) ) ;
#13420 = AXIS2_PLACEMENT_3D ( 'NONE', #2580, #24737, #1172 ) ;
#13421 = CYLINDRICAL_SURFACE ( 'NONE', #33810, 6.118999999999985562 ) ;
#13422 = EDGE_LOOP ( 'NONE', ( #8784, #35897, #18691, #40870 ) ) ;
#13423 = CARTESIAN_POINT ( 'NONE',  ( 789.9200121543843807, -1.987414471687640294, 317.0176451133914384 ) ) ;
#13424 = CARTESIAN_POINT ( 'NONE',  ( 749.5768839229115201, -324.5545181178796952, -358.0661480581553064 ) ) ;
#13425 = VECTOR ( 'NONE', #3405, 999.9999999999998863 ) ;
#13426 = CARTESIAN_POINT ( 'NONE',  ( 746.8695393053151292, -245.9073299311469896, 327.6429770376306578 ) ) ;
#13427 = CARTESIAN_POINT ( 'NONE',  ( 796.1575198192839480, -342.0090635724251342, 359.4546378042384163 ) ) ;
#13428 = CARTESIAN_POINT ( 'NONE',  ( 798.7617431975189675, -435.6237781080499190, 323.0428371773161871 ) ) ;
#13429 = CARTESIAN_POINT ( 'NONE',  ( 790.9844846989617508, -166.3726999360620198, -317.2208543904092721 ) ) ;
#13430 = CARTESIAN_POINT ( 'NONE',  ( 759.7806653035534055, -102.9982390220565520, -324.8639956371180801 ) ) ;
#13431 = CARTESIAN_POINT ( 'NONE',  ( 800.2193346964446619, -306.9982390220558841, -355.1360043628816925 ) ) ;
#13432 = ORIENTED_EDGE ( 'NONE', *, *, #41613, .T. ) ;
#13433 = EDGE_CURVE ( 'NONE', #34173, #45635, #38207, .T. ) ;
#13434 = CARTESIAN_POINT ( 'NONE',  ( 799.4546378042377910, -297.0783235625957559, 356.1575198192848006 ) ) ;
#13435 = CARTESIAN_POINT ( 'NONE',  ( -37.63011601220122770, -513.1383975375929367, -369.9999999999999432 ) ) ;
#13436 = EDGE_CURVE ( 'NONE', #40320, #25938, #20855, .T. ) ;
#13437 = CARTESIAN_POINT ( 'NONE',  ( 757.4527132478984868, -136.3726999360621051, 329.1273215169538844 ) ) ;
#13438 = CARTESIAN_POINT ( 'NONE',  ( 792.1044303154645831, -12.45278447660232146, 317.8323909638837677 ) ) ;
#13439 = ORIENTED_EDGE ( 'NONE', *, *, #39900, .F. ) ;
#13440 = CARTESIAN_POINT ( 'NONE',  ( 745.1792804349281596, -350.1908817542433212, -343.7566961878542884 ) ) ;
#13441 = CARTESIAN_POINT ( 'NONE',  ( 805.6418435158337843, -245.4636090269709143, 363.8556311672236916 ) ) ;
#13442 = CARTESIAN_POINT ( 'NONE',  ( 791.9812246680005501, -332.6346026584195101, -361.9419747391813189 ) ) ;
#13443 = PLANE ( 'NONE',  #35527 ) ;
#13444 = CARTESIAN_POINT ( 'NONE',  ( 798.5707757039680246, -173.4636090269710849, -356.7845633553585003 ) ) ;
#13445 = EDGE_CURVE ( 'NONE', #41260, #27562, #21154, .T. ) ;
#13446 = EDGE_CURVE ( 'NONE', #15113, #29224, #4897, .T. ) ;
#13447 = CARTESIAN_POINT ( 'NONE',  ( 815.2698199232961542, -88.81642084023842187, 342.5225473063383106 ) ) ;
#13448 = AXIS2_PLACEMENT_3D ( 'NONE', #6563, #27812, #24331 ) ;
#13449 = CARTESIAN_POINT ( 'NONE',  ( 796.3364271039121149, -452.9681489794448339, 359.1033184105688747 ) ) ;
#13450 = CARTESIAN_POINT ( 'NONE',  ( 796.9462024416508257, -372.4527844766012095, -308.9653473494370246 ) ) ;
#13451 = CARTESIAN_POINT ( 'NONE',  ( 794.9999999999993179, 205.0000000000000568, -245.0000000000000284 ) ) ;
#13452 = CARTESIAN_POINT ( 'NONE',  ( 778.7629533639073998, -320.7363362996979390, 375.0009284576466371 ) ) ;
#13453 = CARTESIAN_POINT ( 'NONE',  ( 999.5857864376259840, -600.0000000000001137, -360.0000000000000000 ) ) ;
#13454 = CARTESIAN_POINT ( 'NONE',  ( 808.0189434323515343, -302.0891481129650629, 319.0252816721025511 ) ) ;
#13455 = CARTESIAN_POINT ( 'NONE',  ( 796.7737145352015204, -20.63460265842048003, -370.7187646348536987 ) ) ;
#13456 = CARTESIAN_POINT ( 'NONE',  ( 801.9419747391806368, -258.4527844766016074, -351.9812246680014027 ) ) ;
#13457 = DIRECTION ( 'NONE',  ( -1.000000000000000000, 1.892425610156518354E-16, 0.000000000000000000 ) ) ;
#13458 = CARTESIAN_POINT ( 'NONE',  ( 797.6776695296629214, -403.5436935675101608, 357.6776695296636603 ) ) ;
#13459 = CARTESIAN_POINT ( 'NONE',  ( 798.5707757039680246, -149.4636090269711417, 356.7845633553585003 ) ) ;
#13460 = CARTESIAN_POINT ( 'NONE',  ( 812.3518521366052028, -25.09997266333519050, -326.5853460496235243 ) ) ;
#13461 = CARTESIAN_POINT ( 'NONE',  ( 756.7813123517142913, -43.98741447168752217, -329.9779781133712504 ) ) ;
#13462 = CARTESIAN_POINT ( 'NONE',  ( 788.7631598425961101, -73.44195992623286884, 305.7194118038759143 ) ) ;
#13463 = CARTESIAN_POINT ( 'NONE',  ( 804.9363028652555840, -376.2709662947829656, 338.2165204200192079 ) ) ;
#13464 = DIRECTION ( 'NONE',  ( 0.000000000000000000, 1.000000000000000000, 0.000000000000000000 ) ) ;
#13465 = PRESENTATION_STYLE_ASSIGNMENT (( #37486 ) ) ;
#13466 = CARTESIAN_POINT ( 'NONE',  ( 759.7806653035534055, -438.9982390220553157, 324.8639956371180801 ) ) ;
#13467 = EDGE_LOOP ( 'NONE', ( #45009, #19011, #29556, #13089 ) ) ;
#13468 = CARTESIAN_POINT ( 'NONE',  ( 788.8264449731200330, -69.18005720387488111, -363.6646147819171233 ) ) ;
#13469 = CARTESIAN_POINT ( 'NONE',  ( 784.0799538623451781, -347.8055962898683333, -364.6971507214555572 ) ) ;
#13471 = CARTESIAN_POINT ( 'NONE',  ( 785.3687786644885591, -179.3618753856927128, 315.3201227861280813 ) ) ;
#13470 = CARTESIAN_POINT ( 'NONE',  ( 803.6646147819161570, -209.9073299311470748, 348.8264449731210561 ) ) ;
#13472 = VECTOR ( 'NONE', #31097, 999.9999999999998863 ) ;
#13473 = CARTESIAN_POINT ( 'NONE',  ( 778.7502325331095108, -360.3510508353228374, -304.6391490659818828 ) ) ;
#13474 = CARTESIAN_POINT ( 'NONE',  ( -786.4999999999993179, -32.84703287382745174, 757.2634078669104838 ) ) ;
#13475 = ORIENTED_EDGE ( 'NONE', *, *, #29751, .F. ) ;
#13476 = CARTESIAN_POINT ( 'NONE',  ( 788.8264449731200330, -405.1800572038737300, 363.6646147819171233 ) ) ;
#13477 = VERTEX_POINT ( 'NONE', #44909 ) ;
#13478 =( NAMED_UNIT ( * ) PLANE_ANGLE_UNIT ( ) SI_UNIT ( $, .RADIAN. ) );
#13479 = CARTESIAN_POINT ( 'NONE',  ( 812.7932403749906598, -207.1800572038744406, -327.7687537140311633 ) ) ;
#13480 = CARTESIAN_POINT ( 'NONE',  ( 804.7487373415286811, -115.5436935675110988, 364.7487373415288516 ) ) ;
#13481 = ORIENTED_EDGE ( 'NONE', *, *, #6921, .F. ) ;
#13482 = CARTESIAN_POINT ( 'NONE',  ( 801.9419747391806368, -210.4527844766016926, -351.9812246680014027 ) ) ;
#13483 = ORIENTED_EDGE ( 'NONE', *, *, #15671, .F. ) ;
#13484 = CARTESIAN_POINT ( 'NONE',  ( 759.9864689768902508, -314.0891481129650629, -354.9819416627836404 ) ) ;
#13485 = CARTESIAN_POINT ( 'NONE',  ( 805.1927285166397041, -16.81642084023866701, -341.8018195045277707 ) ) ;
#13486 = CARTESIAN_POINT ( 'NONE',  ( 766.7756240680305382, -206.5328690171415360, 361.5560724626415663 ) ) ;
#13487 = CARTESIAN_POINT ( 'NONE',  ( 779.9999999999992042, -462.9681489794448339, 309.9999999999998863 ) ) ;
#13488 = CARTESIAN_POINT ( 'NONE',  ( 794.9999999999993179, -365.3551492539851893, 18.13243251470705886 ) ) ;
#13489 = ORIENTED_EDGE ( 'NONE', *, *, #20442, .T. ) ;
#13490 = CARTESIAN_POINT ( 'NONE',  ( 797.8594530101008786, 10.45630643248850866, -322.1405469898980982 ) ) ;
#13491 = CARTESIAN_POINT ( 'NONE',  ( 774.2415430293718828, 19.23444159658009056, -310.5578503957772796 ) ) ;
#13492 = DIRECTION ( 'NONE',  ( -1.000000000000000000, 0.000000000000000000, -0.000000000000000000 ) ) ;
#13493 = ORIENTED_EDGE ( 'NONE', *, *, #32811, .T. ) ;
#13494 = CARTESIAN_POINT ( 'NONE',  ( 766.4474001241216001, -235.0999726633344835, -307.3154664389482491 ) ) ;
#13496 = CARTESIAN_POINT ( 'NONE',  ( 804.6798772138708955, -207.7255117493289447, -334.6312213355107019 ) ) ;
#13495 = LINE ( 'NONE', #31268, #42324 ) ;
#13497 = CARTESIAN_POINT ( 'NONE',  ( 795.9930595647434757, -387.0783235625955285, -320.7433823573372820 ) ) ;
#13498 =( BOUNDED_CURVE ( )  B_SPLINE_CURVE ( 2, ( #28891, #35574, #25417, #42973, #39770, #42527, #254, #31884, #17816, #491, #38849, #10893, #3951, #14597, #11338, #32365, #39538, #14351, #39074, #32588, #18290, #8118, #28670, #24960, #22179, #18045, #32126, #28429, #36273, #36055, #21496, #35819, #42748, #10649, #720, #11110, #25180, #39292, #7895, #14818, #7646, #4630, #11577, #18726, #21725, #4198, #21969, #1166, #4418, #35353, #42287, #931, #15034, #32814, #29122, #7423, #43206, #24729, #25657, #15275, #3728, #7202, #21273, #36947, #40646, #36729, #33263, #29362, #22854, #43652, #19621, #30240, #23068, #15496, #4859, #2066, #33055, #9236, #1609, #25869, #44332, #1392, #44105, #37167, #19395, #43432, #33934, #33717, #12022, #16158, #40203, #29576, #26089, #11800, #8564, #26548, #22630, #5087, #5526, #5300, #12469, #23307, #30019, #39980, #15707, #33481, #2285, #12687, #19178, #8999, #29791, #26767, #40872, #1827, #8329, #15935, #22392, #26329, #37408, #5766, #43871, #12250, #40434, #19854, #36496, #18960, #8786, #41556, #30709, #9464, #44806, #24222, #6676, #20072, #27694, #38330, #42022, #34393, #16384, #13387, #10368, #34147, #24444, #20302, #12926, #31388, #20981, #38102, #34843, #13163, #30462, #16858, #45493, #17298, #20753, #38548, #44565, #6901, #27459, #41334, #41111, #27242, #2517, #3207, #9910, #31153, #27012, #13849, #23527, #35077, #27927, #37629, #10147, #5980, #23982, #16623, #9684, #23748, #37862, #6209, #2764, #13610, #30938, #45031, #6458, #20537, #34631, #2988, #17075, #45251, #41797, #42473, #32314, #35768, #885, #3684, #7149, #38793, #24674, #7375, #45722, #21677, #28150, #670, #14075, #21226, #32538, #32068, #39247, #39720, #7842, #14987, #35528, #17771, #29074, #10839, #24911, #35307, #43160, #42923, #28371, #11289, #440, #42702, #11527, #25610, #31837, #14772, #14542, #21917, #42242, #8070, #22132, #3449, #28620, #3903, #11066, #17546, #39025, #10599, #31619, #207, #25133, #17998, #14300, #28843, #21451, #36005, #7599, #25368, #4146, #18240, #4368, #18676, #8511, #32767, #12198, #11967, #1557, #12641, #4585, #36446, #39934, #25822, #11755, #40148, #1112, #4809, #43601, #22579, #5253, #26278, #36900, #8279, #33006, #12421, #40390, #36681, #5040, #16110, #29526, #26035, #19132, #22343, #2014, #29970, #15450, #29734, #33220, #15227, #8741, #15657, #43814, #22807, #19343, #33428, #1772, #30195, #43388, #18913, #36221, #15882, #44054, #40822, #26501, #29314, #1346, #40602, #8953, #26722, #23022, #37113, #5473, #19568, #33665, #44285, #9178, #16805, #2712, #37581, #16335, #44754, #41284, #23253, #30885, #5935, #13561, #24173, #17023, #9412, #44513, #41744, #26955, #3155, #9637, #19803, #38281, #27879, #44980, #10097, #20025, #37355, #41977, #27636, #34102, #6626, #2468, #41055, #16575, #5716, #13113, #20490, #23701, #23479, #45199, #13334, #38050, #33887, #20701, #2240, #17247, #27412, #30416, #34792, #37813, #34576, #6162, #2936, #23930, #41509, #12873, #9859, #20251, #34342, #6408, #31100, #31333, #45440, #13802, #17494, #18181, #24390, #14485, #24859, #28312, #42412, #11016, #28564, #31784, #35947, #31572, #24614, #10319, #28094, #154, #17720, #21402, #17942, #38976, #32010, #38733, #32484, #10782, #45672, #14025, #38494, #39423, #18404, #3400, #3851, #35476, #7094, #42188, #21175, #32257, #615, #10538, #21624, #14717, #4313, #7326, #35255, #3633, #28792, #14243, #834, #383, #6846, #25310, #14933, #42654, #42870, #25083, #20926, #39197, #7778, #11237, #21854, #29016, #35023, #7547, #35707, #4083, #40336, #11698, #15164, #19285, #36630, #12139, #39662, #26448, #8012, #22964, #12372, #37059, #36848, #4531, #40088, #40547, #25549, #8898, #1502, #22080, #33166, #36171, #8450, #8688, #15600, #15391, #11909, #18624, #29469, #32710, #19078, #18856, #22520, #19507, #11469, #33604, #1057, #43543, #25981, #4984, #29683, #43760, #29255, #22752, #43332, #25771, #5412, #26221, #5199, #1956, #1716, #16056, #33372, #39883, #43099, #8224, #22293, #36389, #4752, #32946, #1292, #15821, #29912, #43997, #2410, #44923, #20196, #30829, #33835, #26891, #6345, #6107, #34052, #44693, #10041, #23427, #2880, #40998, #2189, #41687, #23872, #9358, #23647, #37528, #44228, #34277, #13053, #16511, #30593, #13281, #2649, #5887, #24110, #37295, #44454, #30140, #16281, #19976, #34739, #27141, #23187, #12585, #41228, #9587, #6569, #37758, #19749, #30360, #26664, #13508, #38222, #5656, #16747, #27358, #12810, #41453, #9805, #37992, #40761, #20429, #34522, #16972, #31048, #45147, #27581, #20647, #3099, #9119, #42819, #21118, #13742, #32197, #21795, #38921, #35646, #31514, #31277, #17664, #21563, #45617, #4018, #28039, #34967, #13965, #45380, #42132, #14424, #10483, #3341, #39141, #10722, #31950, #27819, #559, #41916, #11180, #14662, #25250, #18119, #17434, #28503, #24557, #42601, #17883, #21344, #10260, #7273, #24337, #14186, #10962, #35420, #35202, #31727, #38441, #3578, #6792, #3793, #38673, #320, #25031, #39360, #94, #17190, #28254, #7714, #7032, #7491, #42353, #24802, #28738, #20869, #35888, #19022, #43710, #40037, #4262, #8845, #8631, #40277, #29855, #32435, #40493, #15336, #29191, #28961, #22913, #11857, #25930, #18354, #11641, #18794, #43941, #4924, #783, #22239, #8393, #14883, #22693, #1230, #1665, #43041, #15768, #26162, #11403, #25491, #15551, #1450, #26392, #39603, #22462, #36792, #39831, #22027, #5149, #12085, #36570, #43270, #33113, #7959, #36116, #4481, #36336, #25719, #4694, #29418, #29631, #19233, #18573, #33320, #32656, #998, #12317, #32885, #15101, #8174, #43490, #2823, #23368, #30297, #9746, #2131, #9059, #13227, #37004, #23812, #44168, #44864, #33994, #30529, #6279, #13450, #12531, #2585, #19917, #41398, #30085, #34461, #20367, #5358, #23126, #26826, #44392, #2346, #44628, #16446, #12993, #19687, #27080, #5832, #16915, #34212, #12747, #37922, #27517, #9527, #41173, #30994, #23591, #26605, #5596, #27304, #45092, #40705, #16688, #41619, #37696, #9975, #33780, #6046, #40933, #16220, #20135, #37230, #9299, #30773, #19452, #33546, #1896, #16003, #37470, #14361, #3962, #6513, #14609, #35137, #3274, #3045, #28681, #31670, #37, #42758, #31453, #38610, #18055, #24743, #20592, #42076, #14131, #28442, #10202, #21285, #34909, #35363, #38861, #28203, #34687, #42297, #17136, #21054, #3738, #10660, #10425, #6969, #31219, #24502, #45313, #7212, #45555, #17826, #31894, #21506, #24280, #27756, #13675, #41858, #27981, #38386, #6735, #13907, #3516, #265, #42541, #10905, #20810, #17366, #24971, #39084, #17600, #7433, #35585, #32137, #502, #24046, #38165, #23259, #5477, #36685, #5257, #19136, #25190, #15889, #26282, #29739, #43818, #12426, #29974, #33224, #37360, #26725, #5721, #40394, #12204, #19349, #16339, #5045, #4209, #11121, #1563, #15661, #33891, #8745, #732, #14829, #39303, #40826, #19808, #18301, #33432, #22812, #1777 ),
 .UNSPECIFIED., .F., .T. ) 
 B_SPLINE_CURVE_WITH_KNOTS ( ( 3, 2, 2, 2, 2, 2, 2, 2, 2, 2, 2, 2, 2, 2, 2, 2, 2, 2, 2, 2, 2, 2, 2, 2, 2, 2, 2, 2, 2, 2, 2, 2, 2, 2, 2, 2, 2, 2, 2, 2, 2, 2, 2, 2, 2, 2, 2, 2, 2, 2, 2, 2, 2, 2, 2, 2, 2, 2, 2, 2, 2, 2, 2, 2, 2, 2, 2, 2, 2, 2, 2, 2, 2, 2, 2, 2, 2, 2, 2, 2, 2, 2, 2, 2, 2, 2, 2, 2, 2, 2, 2, 2, 2, 2, 2, 2, 2, 2, 2, 2, 2, 2, 2, 2, 2, 2, 2, 2, 2, 2, 2, 2, 2, 2, 2, 2, 2, 2, 2, 2, 2, 2, 2, 2, 2, 2, 2, 2, 2, 2, 2, 2, 2, 2, 2, 2, 2, 2, 2, 2, 2, 2, 2, 2, 2, 2, 2, 2, 2, 2, 2, 2, 2, 2, 2, 2, 2, 2, 2, 2, 2, 2, 2, 2, 2, 2, 2, 2, 2, 2, 2, 2, 2, 2, 2, 2, 2, 2, 2, 2, 2, 2, 2, 2, 2, 2, 2, 2, 2, 2, 2, 2, 2, 2, 2, 2, 2, 2, 2, 2, 2, 2, 2, 2, 2, 2, 2, 2, 2, 2, 2, 2, 2, 2, 2, 2, 2, 2, 2, 2, 2, 2, 2, 2, 2, 2, 2, 2, 2, 2, 2, 2, 2, 2, 2, 2, 2, 2, 2, 2, 2, 2, 2, 2, 2, 2, 2, 2, 2, 2, 2, 2, 2, 2, 2, 2, 2, 2, 2, 2, 2, 2, 2, 2, 2, 2, 2, 2, 2, 2, 2, 2, 2, 2, 2, 2, 2, 2, 2, 2, 2, 2, 2, 2, 2, 2, 2, 2, 2, 2, 2, 2, 2, 2, 2, 2, 2, 2, 2, 2, 2, 2, 2, 2, 2, 2, 2, 2, 2, 2, 2, 2, 2, 2, 2, 2, 2, 2, 2, 2, 2, 2, 2, 2, 2, 2, 2, 2, 2, 2, 2, 2, 2, 2, 2, 2, 2, 2, 2, 2, 2, 2, 2, 2, 2, 2, 2, 2, 2, 2, 2, 2, 2, 2, 2, 2, 2, 2, 2, 2, 2, 2, 2, 2, 2, 2, 2, 2, 2, 2, 2, 2, 2, 2, 2, 2, 2, 2, 2, 2, 2, 2, 2, 2, 2, 2, 2, 2, 2, 2, 2, 2, 2, 2, 2, 2, 2, 2, 2, 2, 2, 2, 2, 2, 2, 2, 2, 2, 2, 2, 2, 2, 2, 2, 2, 2, 2, 2, 2, 2, 2, 2, 2, 2, 2, 2, 2, 2, 2, 2, 2, 3 ),
 ( 8.755858387967423303E-18, 0.002272727272727281290, 0.004545454545454553907, 0.006818181818181826524, 0.009090909090909099141, 0.01136363636363637263, 0.01363636363636364437, 0.01590909090909091786, 0.01818181818181819134, 0.02045454545454546483, 0.02272727272727273831, 0.02500000000000001180, 0.02727272727272728181, 0.02954545454545455530, 0.03181818181818182184, 0.03409090909090909532, 0.03636363636363636881, 0.03863636363636364229, 0.04090909090909091578, 0.04318181818181818926, 0.04545454545454546275, 0.04772727272727273623, 0.05000000000000000971, 0.05227272727272727626, 0.05454545454545454974, 0.05681818181818182323, 0.05909090909090909671, 0.06136363636363637020, 0.06363636363636364368, 0.06590909090909091717, 0.06818181818181819065, 0.07045454545454546413, 0.07272727272727273762, 0.07500000000000001110, 0.07727272727272728459, 0.07954545454545455807, 0.08181818181818183155, 0.08409090909090910504, 0.08636363636363637852, 0.08863636363636365201, 0.09090909090909092549, 0.09318181818181819898, 0.09545454545454547246, 0.09772727272727274594, 0.1000000000000000194, 0.1022727272727272929, 0.1045454545454545525, 0.1068181818181818260, 0.1090909090909090995, 0.1113636363636363730, 0.1136363636363636465, 0.1159090909090909199, 0.1181818181818181934, 0.1204545454545454669, 0.1227272727272727404, 0.1250000000000000000, 0.1272727272727272596, 0.1295454545454545470, 0.1318181818181818066, 0.1340909090909090939, 0.1363636363636363535, 0.1386363636363636409, 0.1409090909090909005, 0.1431818181818181879, 0.1454545454545454475, 0.1477272727272727348, 0.1499999999999999944, 0.1522727272727272818, 0.1545454545454545414, 0.1568181818181818288, 0.1590909090909090884, 0.1613636363636363757, 0.1636363636363636354, 0.1659090909090909227, 0.1681818181818181823, 0.1704545454545454419, 0.1727272727272727293, 0.1749999999999999889, 0.1772727272727272763, 0.1795454545454545359, 0.1818181818181818232, 0.1840909090909090828, 0.1863636363636363702, 0.1886363636363636298, 0.1909090909090909172, 0.1931818181818181768, 0.1954545454545454641, 0.1977272727272727237, 0.2000000000000000111, 0.2022727272727272707, 0.2045454545454545581, 0.2068181818181818177, 0.2090909090909090773, 0.2113636363636363646, 0.2136363636363636243, 0.2159090909090909116, 0.2181818181818181712, 0.2204545454545454586, 0.2227272727272727182, 0.2250000000000000056, 0.2272727272727272652, 0.2295454545454545525, 0.2318181818181818121, 0.2340909090909090995, 0.2363636363636363591, 0.2386363636363636465, 0.2409090909090909061, 0.2431818181818181934, 0.2454545454545454530, 0.2477272727272727404, 0.2500000000000000000, 0.2522727272727272596, 0.2545454545454545192, 0.2568181818181818343, 0.2590909090909090939, 0.2613636363636363535, 0.2636363636363636131, 0.2659090909090909283, 0.2681818181818181879, 0.2704545454545454475, 0.2727272727272727071, 0.2750000000000000222, 0.2772727272727272818, 0.2795454545454545414, 0.2818181818181818010, 0.2840909090909091161, 0.2863636363636363757, 0.2886363636363636354, 0.2909090909090908950, 0.2931818181818181546, 0.2954545454545454697, 0.2977272727272727293, 0.2999999999999999889, 0.3022727272727272485, 0.3045454545454545636, 0.3068181818181818232, 0.3090909090909090828, 0.3113636363636363424, 0.3136363636363636576, 0.3159090909090909172, 0.3181818181818181768, 0.3204545454545454364, 0.3227272727272727515, 0.3250000000000000111, 0.3272727272727272707, 0.3295454545454545303, 0.3318181818181818454, 0.3340909090909091050, 0.3363636363636363646, 0.3386363636363636243, 0.3409090909090908839, 0.3431818181818181990, 0.3454545454545454586, 0.3477272727272727182, 0.3499999999999999778, 0.3522727272727272929, 0.3545454545454545525, 0.3568181818181818121, 0.3590909090909090717, 0.3613636363636363869, 0.3636363636363636465, 0.3659090909090909061, 0.3681818181818181657, 0.3704545454545454808, 0.3727272727272727404, 0.3749999999999999445, 0.3772727272727272596, 0.3795454545454545192, 0.3818181818181818343, 0.3840909090909090939, 0.3863636363636363535, 0.3886363636363636131, 0.3909090909090909283, 0.3931818181818181879, 0.3954545454545454475, 0.3977272727272727071, 0.4000000000000000222, 0.4022727272727272818, 0.4045454545454545414, 0.4068181818181818010, 0.4090909090909091161, 0.4113636363636363757, 0.4136363636363636354, 0.4159090909090908950, 0.4181818181818181546, 0.4204545454545454697, 0.4227272727272727293, 0.4249999999999999889, 0.4272727272727272485, 0.4295454545454545636, 0.4318181818181818232, 0.4340909090909090828, 0.4363636363636363424, 0.4386363636363636576, 0.4409090909090909172, 0.4431818181818181768, 0.4454545454545454364, 0.4477272727272727515, 0.4500000000000000111, 0.4522727272727272707, 0.4545454545454545303, 0.4568181818181818454, 0.4590909090909091050, 0.4613636363636363646, 0.4636363636363636243, 0.4659090909090908839, 0.4681818181818181990, 0.4704545454545454586, 0.4727272727272727182, 0.4749999999999999778, 0.4772727272727272929, 0.4795454545454545525, 0.4818181818181818121, 0.4840909090909090717, 0.4863636363636363869, 0.4886363636363636465, 0.4909090909090909061, 0.4931818181818181657, 0.4954545454545454808, 0.4977272727272727404, 0.5000000000000000000, 0.5022727272727273151, 0.5045454545454545192, 0.5068181818181818343, 0.5090909090909090384, 0.5113636363636363535, 0.5136363636363636687, 0.5159090909090908728, 0.5181818181818181879, 0.5204545454545455030, 0.5227272727272727071, 0.5250000000000000222, 0.5272727272727272263, 0.5295454545454545414, 0.5318181818181818565, 0.5340909090909090606, 0.5363636363636363757, 0.5386363636363636909, 0.5409090909090908950, 0.5431818181818182101, 0.5454545454545454142, 0.5477272727272727293, 0.5500000000000000444, 0.5522727272727272485, 0.5545454545454545636, 0.5568181818181817677, 0.5590909090909090828, 0.5613636363636363980, 0.5636363636363636020, 0.5659090909090909172, 0.5681818181818182323, 0.5704545454545454364, 0.5727272727272727515, 0.5749999999999999556, 0.5772727272727272707, 0.5795454545454545858, 0.5818181818181817899, 0.5840909090909091050, 0.5863636363636363091, 0.5886363636363636243, 0.5909090909090909394, 0.5931818181818181435, 0.5954545454545454586, 0.5977272727272727737, 0.5999999999999999778, 0.6022727272727272929, 0.6045454545454544970, 0.6068181818181818121, 0.6090909090909091272, 0.6113636363636362203, 0.6136363636363636465, 0.6159090909090909616, 0.6181818181818181657, 0.6204545454545454808, 0.6227272727272726849, 0.6250000000000000000, 0.6272727272727273151, 0.6295454545454546302, 0.6318181818181818343, 0.6340909090909090384, 0.6363636363636363535, 0.6386363636363636687, 0.6409090909090908728, 0.6431818181818181879, 0.6454545454545455030, 0.6477272727272727071, 0.6500000000000000222, 0.6522727272727272263, 0.6545454545454545414, 0.6568181818181818565, 0.6590909090909090606, 0.6613636363636363757, 0.6636363636363636909, 0.6659090909090908950, 0.6681818181818182101, 0.6704545454545454142, 0.6727272727272727293, 0.6750000000000000444, 0.6772727272727272485, 0.6795454545454545636, 0.6818181818181817677, 0.6840909090909090828, 0.6863636363636363980, 0.6886363636363636020, 0.6909090909090909172, 0.6931818181818182323, 0.6954545454545454364, 0.6977272727272727515, 0.6999999999999999556, 0.7022727272727272707, 0.7045454545454545858, 0.7068181818181817899, 0.7090909090909091050, 0.7113636363636363091, 0.7136363636363636243, 0.7159090909090909394, 0.7181818181818181435, 0.7204545454545454586, 0.7227272727272727737, 0.7249999999999999778, 0.7272727272727272929, 0.7295454545454544970, 0.7318181818181818121, 0.7340909090909091272, 0.7363636363636363313, 0.7386363636363636465, 0.7409090909090909616, 0.7431818181818181657, 0.7454545454545454808, 0.7477272727272726849, 0.7499999999999998890, 0.7522727272727273151, 0.7545454545454545192, 0.7568181818181818343, 0.7590909090909090384, 0.7613636363636363535, 0.7636363636363636687, 0.7659090909090908728, 0.7681818181818181879, 0.7704545454545455030, 0.7727272727272727071, 0.7750000000000000222, 0.7772727272727272263, 0.7795454545454545414, 0.7818181818181818565, 0.7840909090909090606, 0.7863636363636363757, 0.7886363636363636909, 0.7909090909090908950, 0.7931818181818182101, 0.7954545454545454142, 0.7977272727272727293, 0.8000000000000000444, 0.8022727272727272485, 0.8045454545454545636, 0.8068181818181817677, 0.8090909090909090828, 0.8113636363636363980, 0.8136363636363636020, 0.8159090909090909172, 0.8181818181818182323, 0.8204545454545454364, 0.8227272727272727515, 0.8249999999999999556, 0.8272727272727272707, 0.8295454545454545858, 0.8318181818181817899, 0.8340909090909091050, 0.8363636363636363091, 0.8386363636363636243, 0.8409090909090909394, 0.8431818181818181435, 0.8454545454545454586, 0.8477272727272727737, 0.8499999999999999778, 0.8522727272727272929, 0.8545454545454544970, 0.8568181818181818121, 0.8590909090909091272, 0.8613636363636363313, 0.8636363636363636465, 0.8659090909090909616, 0.8681818181818181657, 0.8704545454545453698, 0.8727272727272726849, 0.8750000000000000000, 0.8772727272727273151, 0.8795454545454545192, 0.8818181818181818343, 0.8840909090909090384, 0.8863636363636363535, 0.8886363636363637797, 0.8909090909090908728, 0.8931818181818181879, 0.8954545454545455030, 0.8977272727272727071, 0.9000000000000000222, 0.9022727272727272263, 0.9045454545454545414, 0.9068181818181818565, 0.9090909090909090606, 0.9113636363636363757, 0.9136363636363636909, 0.9159090909090908950, 0.9181818181818182101, 0.9204545454545454142, 0.9227272727272727293, 0.9250000000000000444, 0.9272727272727272485, 0.9295454545454545636, 0.9318181818181817677, 0.9340909090909090828, 0.9363636363636363980, 0.9386363636363636020, 0.9409090909090909172, 0.9431818181818182323, 0.9454545454545454364, 0.9477272727272727515, 0.9499999999999999556, 0.9522727272727272707, 0.9545454545454545858, 0.9568181818181817899, 0.9590909090909091050, 0.9613636363636363091, 0.9636363636363636243, 0.9659090909090909394, 0.9681818181818181435, 0.9704545454545454586, 0.9727272727272727737, 0.9749999999999999778, 0.9772727272727272929, 0.9781254700864302487 ),
 .UNSPECIFIED. ) 
 CURVE ( )  GEOMETRIC_REPRESENTATION_ITEM ( )  RATIONAL_B_SPLINE_CURVE ( ( 1.000000000000000000, 0.9898214418809326842, 1.000000000000000000, 0.9898214418809326842, 1.000000000000000000, 0.9898214418809326842, 1.000000000000000000, 0.9898214418809326842, 1.000000000000000000, 0.9898214418809326842, 1.000000000000000000, 0.9898214418809326842, 1.000000000000000000, 0.9898214418809326842, 1.000000000000000000, 0.9898214418809326842, 1.000000000000000000, 0.9898214418809326842, 1.000000000000000000, 0.9898214418809326842, 1.000000000000000000, 0.9898214418809326842, 1.000000000000000000, 0.9898214418809326842, 1.000000000000000000, 0.9898214418809326842, 1.000000000000000000, 0.9898214418809326842, 1.000000000000000000, 0.9898214418809326842, 1.000000000000000000, 0.9898214418809326842, 1.000000000000000000, 0.9898214418809326842, 1.000000000000000000, 0.9898214418809326842, 1.000000000000000000, 0.9898214418809326842, 1.000000000000000000, 0.9898214418809326842, 1.000000000000000000, 0.9898214418809326842, 1.000000000000000000, 0.9898214418809326842, 1.000000000000000000, 0.9898214418809326842, 1.000000000000000000, 0.9898214418809326842, 1.000000000000000000, 0.9898214418809326842, 1.000000000000000000, 0.9898214418809326842, 1.000000000000000000, 0.9898214418809326842, 1.000000000000000000, 0.9898214418809326842, 1.000000000000000000, 0.9898214418809326842, 1.000000000000000000, 0.9898214418809326842, 1.000000000000000000, 0.9898214418809326842, 1.000000000000000000, 0.9898214418809326842, 1.000000000000000000, 0.9898214418809326842, 1.000000000000000000, 0.9898214418809326842, 1.000000000000000000, 0.9898214418809326842, 1.000000000000000000, 0.9898214418809326842, 1.000000000000000000, 0.9898214418809326842, 1.000000000000000000, 0.9898214418809326842, 1.000000000000000000, 0.9898214418809326842, 1.000000000000000000, 0.9898214418809326842, 1.000000000000000000, 0.9898214418809326842, 1.000000000000000000, 0.9898214418809326842, 1.000000000000000000, 0.9898214418809326842, 1.000000000000000000, 0.9898214418809326842, 1.000000000000000000, 0.9898214418809326842, 1.000000000000000000, 0.9898214418809326842, 1.000000000000000000, 0.9898214418809326842, 1.000000000000000000, 0.9898214418809326842, 1.000000000000000000, 0.9898214418809326842, 1.000000000000000000, 0.9898214418809326842, 1.000000000000000000, 0.9898214418809326842, 1.000000000000000000, 0.9898214418809326842, 1.000000000000000000, 0.9898214418809326842, 1.000000000000000000, 0.9898214418809326842, 1.000000000000000000, 0.9898214418809326842, 1.000000000000000000, 0.9898214418809326842, 1.000000000000000000, 0.9898214418809326842, 1.000000000000000000, 0.9898214418809326842, 1.000000000000000000, 0.9898214418809326842, 1.000000000000000000, 0.9898214418809326842, 1.000000000000000000, 0.9898214418809326842, 1.000000000000000000, 0.9898214418809326842, 1.000000000000000000, 0.9898214418809326842, 1.000000000000000000, 0.9898214418809326842, 1.000000000000000000, 0.9898214418809326842, 1.000000000000000000, 0.9898214418809326842, 1.000000000000000000, 0.9898214418809326842, 1.000000000000000000, 0.9898214418809326842, 1.000000000000000000, 0.9898214418809326842, 1.000000000000000000, 0.9898214418809326842, 1.000000000000000000, 0.9898214418809326842, 1.000000000000000000, 0.9898214418809326842, 1.000000000000000000, 0.9898214418809326842, 1.000000000000000000, 0.9898214418809326842, 1.000000000000000000, 0.9898214418809326842, 1.000000000000000000, 0.9898214418809326842, 1.000000000000000000, 0.9898214418809326842, 1.000000000000000000, 0.9898214418809326842, 1.000000000000000000, 0.9898214418809326842, 1.000000000000000000, 0.9898214418809326842, 1.000000000000000000, 0.9898214418809326842, 1.000000000000000000, 0.9898214418809326842, 1.000000000000000000, 0.9898214418809326842, 1.000000000000000000, 0.9898214418809326842, 1.000000000000000000, 0.9898214418809326842, 1.000000000000000000, 0.9898214418809326842, 1.000000000000000000, 0.9898214418809326842, 1.000000000000000000, 0.9898214418809326842, 1.000000000000000000, 0.9898214418809326842, 1.000000000000000000, 0.9898214418809326842, 1.000000000000000000, 0.9898214418809326842, 1.000000000000000000, 0.9898214418809326842, 1.000000000000000000, 0.9898214418809326842, 1.000000000000000000, 0.9898214418809326842, 1.000000000000000000, 0.9898214418809326842, 1.000000000000000000, 0.9898214418809326842, 1.000000000000000000, 0.9898214418809326842, 1.000000000000000000, 0.9898214418809326842, 1.000000000000000000, 0.9898214418809326842, 1.000000000000000000, 0.9898214418809326842, 1.000000000000000000, 0.9898214418809326842, 1.000000000000000000, 0.9898214418809326842, 1.000000000000000000, 0.9898214418809326842, 1.000000000000000000, 0.9898214418809326842, 1.000000000000000000, 0.9898214418809326842, 1.000000000000000000, 0.9898214418809326842, 1.000000000000000000, 0.9898214418809326842, 1.000000000000000000, 0.9898214418809326842, 1.000000000000000000, 0.9898214418809326842, 1.000000000000000000, 0.9898214418809326842, 1.000000000000000000, 0.9898214418809326842, 1.000000000000000000, 0.9898214418809326842, 1.000000000000000000, 0.9898214418809326842, 1.000000000000000000, 0.9898214418809326842, 1.000000000000000000, 0.9898214418809326842, 1.000000000000000000, 0.9898214418809326842, 1.000000000000000000, 0.9898214418809326842, 1.000000000000000000, 0.9898214418809326842, 1.000000000000000000, 0.9898214418809326842, 1.000000000000000000, 0.9898214418809326842, 1.000000000000000000, 0.9898214418809326842, 1.000000000000000000, 0.9898214418809326842, 1.000000000000000000, 0.9898214418809326842, 1.000000000000000000, 0.9898214418809326842, 1.000000000000000000, 0.9898214418809326842, 1.000000000000000000, 0.9898214418809326842, 1.000000000000000000, 0.9898214418809326842, 1.000000000000000000, 0.9898214418809326842, 1.000000000000000000, 0.9898214418809326842, 1.000000000000000000, 0.9898214418809326842, 1.000000000000000000, 0.9898214418809326842, 1.000000000000000000, 0.9898214418809326842, 1.000000000000000000, 0.9898214418809326842, 1.000000000000000000, 0.9898214418809326842, 1.000000000000000000, 0.9898214418809326842, 1.000000000000000000, 0.9898214418809326842, 1.000000000000000000, 0.9898214418809326842, 1.000000000000000000, 0.9898214418809326842, 1.000000000000000000, 0.9898214418809326842, 1.000000000000000000, 0.9898214418809326842, 1.000000000000000000, 0.9898214418809326842, 1.000000000000000000, 0.9898214418809326842, 1.000000000000000000, 0.9898214418809326842, 1.000000000000000000, 0.9898214418809326842, 1.000000000000000000, 0.9898214418809326842, 1.000000000000000000, 0.9898214418809326842, 1.000000000000000000, 0.9898214418809326842, 1.000000000000000000, 0.9898214418809326842, 1.000000000000000000, 0.9898214418809326842, 1.000000000000000000, 0.9898214418809326842, 1.000000000000000000, 0.9898214418809326842, 1.000000000000000000, 0.9898214418809326842, 1.000000000000000000, 0.9898214418809326842, 1.000000000000000000, 0.9898214418809326842, 1.000000000000000000, 0.9898214418809326842, 1.000000000000000000, 0.9898214418809326842, 1.000000000000000000, 0.9898214418809326842, 1.000000000000000000, 0.9898214418809326842, 1.000000000000000000, 0.9898214418809326842, 1.000000000000000000, 0.9898214418809326842, 1.000000000000000000, 0.9898214418809326842, 1.000000000000000000, 0.9898214418809326842, 1.000000000000000000, 0.9898214418809326842, 1.000000000000000000, 0.9898214418809326842, 1.000000000000000000, 0.9898214418809326842, 1.000000000000000000, 0.9898214418809326842, 1.000000000000000000, 0.9898214418809326842, 1.000000000000000000, 0.9898214418809326842, 1.000000000000000000, 0.9898214418809326842, 1.000000000000000000, 0.9898214418809326842, 1.000000000000000000, 0.9898214418809326842, 1.000000000000000000, 0.9898214418809326842, 1.000000000000000000, 0.9898214418809326842, 1.000000000000000000, 0.9898214418809326842, 1.000000000000000000, 0.9898214418809326842, 1.000000000000000000, 0.9898214418809326842, 1.000000000000000000, 0.9898214418809326842, 1.000000000000000000, 0.9898214418809326842, 1.000000000000000000, 0.9898214418809326842, 1.000000000000000000, 0.9898214418809326842, 1.000000000000000000, 0.9898214418809326842, 1.000000000000000000, 0.9898214418809326842, 1.000000000000000000, 0.9898214418809326842, 1.000000000000000000, 0.9898214418809326842, 1.000000000000000000, 0.9898214418809326842, 1.000000000000000000, 0.9898214418809326842, 1.000000000000000000, 0.9898214418809326842, 1.000000000000000000, 0.9898214418809326842, 1.000000000000000000, 0.9898214418809326842, 1.000000000000000000, 0.9898214418809326842, 1.000000000000000000, 0.9898214418809326842, 1.000000000000000000, 0.9898214418809326842, 1.000000000000000000, 0.9898214418809326842, 1.000000000000000000, 0.9898214418809326842, 1.000000000000000000, 0.9898214418809326842, 1.000000000000000000, 0.9898214418809326842, 1.000000000000000000, 0.9898214418809326842, 1.000000000000000000, 0.9898214418809326842, 1.000000000000000000, 0.9898214418809326842, 1.000000000000000000, 0.9898214418809326842, 1.000000000000000000, 0.9898214418809326842, 1.000000000000000000, 0.9898214418809326842, 1.000000000000000000, 0.9898214418809326842, 1.000000000000000000, 0.9898214418809326842, 1.000000000000000000, 0.9898214418809326842, 1.000000000000000000, 0.9898214418809326842, 1.000000000000000000, 0.9898214418809326842, 1.000000000000000000, 0.9898214418809326842, 1.000000000000000000, 0.9898214418809326842, 1.000000000000000000, 0.9898214418809326842, 1.000000000000000000, 0.9898214418809326842, 1.000000000000000000, 0.9898214418809326842, 1.000000000000000000, 0.9898214418809326842, 1.000000000000000000, 0.9898214418809326842, 1.000000000000000000, 0.9898214418809326842, 1.000000000000000000, 0.9898214418809326842, 1.000000000000000000, 0.9898214418809326842, 1.000000000000000000, 0.9898214418809326842, 1.000000000000000000, 0.9898214418809326842, 1.000000000000000000, 0.9898214418809326842, 1.000000000000000000, 0.9898214418809326842, 1.000000000000000000, 0.9898214418809326842, 1.000000000000000000, 0.9898214418809326842, 1.000000000000000000, 0.9898214418809326842, 1.000000000000000000, 0.9898214418809326842, 1.000000000000000000, 0.9898214418809326842, 1.000000000000000000, 0.9898214418809326842, 1.000000000000000000, 0.9898214418809326842, 1.000000000000000000, 0.9898214418809326842, 1.000000000000000000, 0.9898214418809326842, 1.000000000000000000, 0.9898214418809326842, 1.000000000000000000, 0.9898214418809326842, 1.000000000000000000, 0.9898214418809326842, 1.000000000000000000, 0.9898214418809326842, 1.000000000000000000, 0.9898214418809326842, 1.000000000000000000, 0.9898214418809326842, 1.000000000000000000, 0.9898214418809326842, 1.000000000000000000, 0.9898214418809326842, 1.000000000000000000, 0.9898214418809326842, 1.000000000000000000, 0.9898214418809326842, 1.000000000000000000, 0.9898214418809326842, 1.000000000000000000, 0.9898214418809326842, 1.000000000000000000, 0.9898214418809326842, 1.000000000000000000, 0.9898214418809326842, 1.000000000000000000, 0.9898214418809326842, 1.000000000000000000, 0.9898214418809326842, 1.000000000000000000, 0.9898214418809326842, 1.000000000000000000, 0.9898214418809326842, 1.000000000000000000, 0.9898214418809326842, 1.000000000000000000, 0.9898214418809326842, 1.000000000000000000, 0.9898214418809326842, 1.000000000000000000, 0.9898214418809326842, 1.000000000000000000, 0.9898214418809326842, 1.000000000000000000, 0.9898214418809326842, 1.000000000000000000, 0.9898214418809326842, 1.000000000000000000, 0.9898214418809326842, 1.000000000000000000, 0.9898214418809326842, 1.000000000000000000, 0.9898214418809326842, 1.000000000000000000, 0.9898214418809326842, 1.000000000000000000, 0.9898214418809326842, 1.000000000000000000, 0.9898214418809326842, 1.000000000000000000, 0.9898214418809326842, 1.000000000000000000, 0.9898214418809326842, 1.000000000000000000, 0.9898214418809326842, 1.000000000000000000, 0.9898214418809326842, 1.000000000000000000, 0.9898214418809326842, 1.000000000000000000, 0.9898214418809326842, 1.000000000000000000, 0.9898214418809326842, 1.000000000000000000, 0.9898214418809326842, 1.000000000000000000, 0.9898214418809326842, 1.000000000000000000, 0.9898214418809326842, 1.000000000000000000, 0.9898214418809326842, 1.000000000000000000, 0.9898214418809326842, 1.000000000000000000, 0.9898214418809326842, 1.000000000000000000, 0.9898214418809326842, 1.000000000000000000, 0.9898214418809326842, 1.000000000000000000, 0.9898214418809326842, 1.000000000000000000, 0.9898214418809326842, 1.000000000000000000, 0.9898214418809326842, 1.000000000000000000, 0.9898214418809326842, 1.000000000000000000, 0.9898214418809326842, 1.000000000000000000, 0.9898214418809326842, 1.000000000000000000, 0.9898214418809326842, 1.000000000000000000, 0.9898214418809326842, 1.000000000000000000, 0.9898214418809326842, 1.000000000000000000, 0.9898214418809326842, 1.000000000000000000, 0.9898214418809326842, 1.000000000000000000, 0.9898214418809326842, 1.000000000000000000, 0.9898214418809326842, 1.000000000000000000, 0.9898214418809326842, 1.000000000000000000, 0.9898214418809326842, 1.000000000000000000, 0.9898214418809326842, 1.000000000000000000, 0.9898214418809326842, 1.000000000000000000, 0.9898214418809326842, 1.000000000000000000, 0.9898214418809326842, 1.000000000000000000, 0.9898214418809326842, 1.000000000000000000, 0.9898214418809326842, 1.000000000000000000, 0.9898214418809326842, 1.000000000000000000, 0.9898214418809326842, 1.000000000000000000, 0.9898214418809326842, 1.000000000000000000, 0.9898214418809326842, 1.000000000000000000, 0.9898214418809326842, 1.000000000000000000, 0.9898214418809326842, 1.000000000000000000, 0.9898214418809326842, 1.000000000000000000, 0.9898214418809326842, 1.000000000000000000, 0.9898214418809326842, 1.000000000000000000, 0.9898214418809326842, 1.000000000000000000, 0.9898214418809326842, 1.000000000000000000, 0.9898214418809326842, 1.000000000000000000, 0.9898214418809326842, 1.000000000000000000, 0.9898214418809326842, 1.000000000000000000, 0.9898214418809326842, 1.000000000000000000, 0.9898214418809326842, 1.000000000000000000, 0.9898214418809326842, 1.000000000000000000, 0.9898214418809326842, 1.000000000000000000, 0.9898214418809326842, 1.000000000000000000, 0.9898214418809326842, 1.000000000000000000, 0.9898214418809326842, 1.000000000000000000, 0.9898214418809326842, 1.000000000000000000, 0.9898214418809326842, 1.000000000000000000, 0.9898214418809326842, 1.000000000000000000, 0.9898214418809326842, 1.000000000000000000, 0.9898214418809326842, 1.000000000000000000, 0.9898214418809326842, 1.000000000000000000, 0.9898214418809326842, 1.000000000000000000, 0.9898214418809326842, 1.000000000000000000, 0.9898214418809326842, 1.000000000000000000, 0.9898214418809326842, 1.000000000000000000, 0.9898214418809326842, 1.000000000000000000, 0.9898214418809326842, 1.000000000000000000, 0.9898214418809326842, 1.000000000000000000, 0.9898214418809326842, 1.000000000000000000, 0.9898214418809326842, 1.000000000000000000, 0.9898214418809326842, 1.000000000000000000, 0.9898214418809326842, 1.000000000000000000, 0.9898214418809326842, 1.000000000000000000, 0.9898214418809326842, 1.000000000000000000, 0.9898214418809326842, 1.000000000000000000, 0.9898214418809326842, 1.000000000000000000, 0.9898214418809326842, 1.000000000000000000, 0.9898214418809326842, 1.000000000000000000, 0.9898214418809326842, 1.000000000000000000, 0.9898214418809326842, 1.000000000000000000, 0.9898214418809326842, 1.000000000000000000, 0.9898214418809326842, 1.000000000000000000, 0.9898214418809326842, 1.000000000000000000, 0.9898214418809326842, 1.000000000000000000, 0.9898214418809326842, 1.000000000000000000, 0.9898214418809326842, 1.000000000000000000, 0.9898214418809326842, 1.000000000000000000, 0.9898214418809326842, 1.000000000000000000, 0.9898214418809326842, 1.000000000000000000, 0.9898214418809326842, 1.000000000000000000, 0.9898214418809326842, 1.000000000000000000, 0.9898214418809326842, 1.000000000000000000, 0.9898214418809326842, 1.000000000000000000, 0.9898214418809326842, 1.000000000000000000, 0.9898214418809326842, 1.000000000000000000, 0.9898214418809326842, 1.000000000000000000, 0.9898214418809326842, 1.000000000000000000, 0.9898214418809326842, 1.000000000000000000, 0.9898214418809326842, 1.000000000000000000, 0.9898214418809326842, 1.000000000000000000, 0.9898214418809326842, 1.000000000000000000, 0.9898214418809326842, 1.000000000000000000, 0.9898214418809326842, 1.000000000000000000, 0.9898214418809326842, 1.000000000000000000, 0.9898214418809326842, 1.000000000000000000, 0.9898214418809326842, 1.000000000000000000, 0.9898214418809326842, 1.000000000000000000, 0.9898214418809326842, 1.000000000000000000, 0.9898214418809326842, 1.000000000000000000, 0.9898214418809326842, 1.000000000000000000, 0.9898214418809326842, 1.000000000000000000, 0.9898214418809326842, 1.000000000000000000, 0.9898214418809326842, 1.000000000000000000, 0.9898214418809326842, 1.000000000000000000, 0.9898214418809326842, 1.000000000000000000, 0.9898214418809326842, 1.000000000000000000, 0.9898214418809326842, 1.000000000000000000, 0.9898214418809326842, 1.000000000000000000, 0.9898214418809326842, 1.000000000000000000, 0.9898214418809326842, 1.000000000000000000, 0.9898214418809326842, 1.000000000000000000, 0.9898214418809326842, 1.000000000000000000, 0.9898214418809326842, 1.000000000000000000, 0.9898214418809326842, 1.000000000000000000, 0.9898214418809326842, 1.000000000000000000, 0.9898214418809326842, 1.000000000000000000, 0.9898214418809326842, 1.000000000000000000, 0.9898214418809326842, 1.000000000000000000, 0.9898214418809326842, 1.000000000000000000, 0.9898214418809326842, 1.000000000000000000, 0.9898214418809326842, 1.000000000000000000, 0.9898214418809326842, 1.000000000000000000, 0.9898214418809326842, 1.000000000000000000, 0.9898214418809326842, 1.000000000000000000, 0.9898214418809326842, 1.000000000000000000, 0.9898214418809326842, 1.000000000000000000, 0.9898214418809326842, 1.000000000000000000, 0.9898214418809326842, 1.000000000000000000, 0.9898214418809326842, 1.000000000000000000, 0.9898214418809326842, 1.000000000000000000, 0.9898214418809326842, 1.000000000000000000, 0.9898214418809326842, 1.000000000000000000, 0.9898214418809326842, 1.000000000000000000, 0.9898214418809326842, 1.000000000000000000, 0.9898214418809326842, 1.000000000000000000, 0.9898214418809326842, 1.000000000000000000, 0.9898214418809326842, 1.000000000000000000, 0.9898214418809326842, 1.000000000000000000, 0.9898214418809326842, 1.000000000000000000, 0.9898214418809326842, 1.000000000000000000, 0.9898214418809326842, 1.000000000000000000, 0.9898214418809326842, 1.000000000000000000, 0.9898214418809326842, 1.000000000000000000, 0.9898214418809326842, 1.000000000000000000, 0.9898214418809326842, 1.000000000000000000, 0.9898214418809326842, 1.000000000000000000, 0.9898214418809326842, 1.000000000000000000, 0.9898214418809326842, 1.000000000000000000, 0.9898214418809326842, 1.000000000000000000, 0.9898214418809326842, 1.000000000000000000, 0.9898214418809326842, 1.000000000000000000, 0.9898214418809326842, 1.000000000000000000, 0.9898214418809326842, 1.000000000000000000, 0.9898214418809326842, 1.000000000000000000, 0.9898214418809326842, 1.000000000000000000, 0.9898214418809326842, 1.000000000000000000, 0.9898214418809326842, 1.000000000000000000, 0.9961809353924466759, 0.9952277490961531914 ) ) 
 REPRESENTATION_ITEM ( '' )  );
#13499 = CARTESIAN_POINT ( 'NONE',  ( -598.8365100919716042, 260.0000000000001705, -206.1189999999899385 ) ) ;
#13500 = CARTESIAN_POINT ( 'NONE',  ( 797.8594530101009923, 10.45630643248851044, -322.1405469898982119 ) ) ;
#13501 = CARTESIAN_POINT ( 'NONE',  ( 757.0176451133909268, -85.09997266333499510, -349.9200121543848354 ) ) ;
#13502 = EDGE_CURVE ( 'NONE', #36535, #30501, #3086, .T. ) ;
#13503 = CARTESIAN_POINT ( 'NONE',  ( 804.1105419155481968, -435.8272453906066062, 347.6308680596136469 ) ) ;
#13504 = CARTESIAN_POINT ( 'NONE',  ( 814.8207195650702488, -362.1908817542432644, 336.2433038121456548 ) ) ;
#13505 = AXIS2_PLACEMENT_3D ( 'NONE', #37290, #23867, #2184 ) ;
#13506 = PLANE ( 'NONE',  #348 ) ;
#13507 = CARTESIAN_POINT ( 'NONE',  ( 746.7653713866222915, 6.739858255585061464, -351.0478386215610271 ) ) ;
#13508 = CARTESIAN_POINT ( 'NONE',  ( 796.7737145352015204, -284.6346026584196807, -370.7187646348536987 ) ) ;
#13509 = DIRECTION ( 'NONE',  ( -1.000000000000000000, -0.000000000000000000, -0.000000000000000000 ) ) ;
#13510 = CARTESIAN_POINT ( 'NONE',  ( 800.0135310231082713, 9.910851887033969021, 325.0180583372163028 ) ) ;
#13511 = CARTESIAN_POINT ( 'NONE',  ( 778.1981804954714335, -82.27096629478388934, -314.8072714833589885 ) ) ;
#13512 = CARTESIAN_POINT ( 'NONE',  ( 787.5531968255692163, 2.172754609392001601, 316.1348686366205811 ) ) ;
#13513 = CARTESIAN_POINT ( 'NONE',  ( 810.4231160770870019, -216.5545181178800931, 321.9338519418446936 ) ) ;
#13514 = CARTESIAN_POINT ( 'NONE',  ( 814.8230680027162407, -173.8055962898689302, -333.7305795820267917 ) ) ;
#13515 = CARTESIAN_POINT ( 'NONE',  ( 744.7301800767019131, -172.8164208402381234, 337.4774526936615757 ) ) ;
#13516 = CARTESIAN_POINT ( 'NONE',  ( 796.9462024416508257, -420.4527844766009252, -308.9653473494370246 ) ) ;
#13517 = DIRECTION ( 'NONE',  ( 1.000000000000000000, 0.000000000000000000, 0.000000000000000000 ) ) ;
#13518 = CARTESIAN_POINT ( 'NONE',  ( 795.1360043628807261, -284.0891481129650629, 360.2193346964456282 ) ) ;
#13519 = CARTESIAN_POINT ( 'NONE',  ( 790.0220218866281812, -55.09997266333508747, 363.2186876482849129 ) ) ;
#13520 = CARTESIAN_POINT ( 'NONE',  ( 778.1981804954714335, -442.2709662947826814, -314.8072714833589885 ) ) ;
#13521 = DIRECTION ( 'NONE',  ( 1.000000000000000000, 0.000000000000000000, 0.000000000000000000 ) ) ;
#13522 = DIRECTION ( 'NONE',  ( -1.000000000000000000, 0.000000000000000000, 0.000000000000000000 ) ) ;
#13524 = CARTESIAN_POINT ( 'NONE',  ( 755.0636971347428243, -316.2709662947832499, 341.7834795799807353 ) ) ;
#13523 = CARTESIAN_POINT ( 'NONE',  ( 796.7845633553578182, -129.6237781080508853, 358.5707757039688204 ) ) ;
#13525 = ORIENTED_EDGE ( 'NONE', *, *, #31676, .T. ) ;
#13526 = CARTESIAN_POINT ( 'NONE',  ( 770.0799878456142551, -253.9874144716868329, -362.9823548866085616 ) ) ;
#13527 = CARTESIAN_POINT ( 'NONE',  ( 803.4237431249931660, -87.18005720387481006, 331.2633955100225194 ) ) ;
#13528 = CARTESIAN_POINT ( 'NONE',  ( 754.0944755984390895, -255.6237781080504874, -364.1009440267246760 ) ) ;
#13529 = FACE_OUTER_BOUND ( 'NONE', #18581, .T. ) ;
#13530 = CARTESIAN_POINT ( 'NONE',  ( 781.2497674668890113, -372.3510508353228374, 375.3608509340180603 ) ) ;
#13531 = ORIENTED_EDGE ( 'NONE', *, *, #919, .F. ) ;
#13532 = CARTESIAN_POINT ( 'NONE',  ( 788.7366044899766848, -275.9073299311469896, 316.5762568750059813 ) ) ;
#13533 = CARTESIAN_POINT ( 'NONE',  ( 774.6312213355099630, -167.3618753856927412, -364.6798772138717482 ) ) ;
#13534 = CARTESIAN_POINT ( 'NONE',  ( 788.8264449731200330, -405.1800572038737300, 363.6646147819171233 ) ) ;
#13535 = CARTESIAN_POINT ( 'NONE',  ( 782.5225473063381969, -118.2709662947837899, -375.2698199232970637 ) ) ;
#13536 = VECTOR ( 'NONE', #34578, 1000.000000000000000 ) ;
#13537 = CARTESIAN_POINT ( 'NONE',  ( 781.8018195045267476, -94.27096629478387513, -365.1927285166407273 ) ) ;
#13538 = VERTEX_POINT ( 'NONE', #13950 ) ;
#13539 = CARTESIAN_POINT ( 'NONE',  ( 798.5707757039680246, -29.46360902697153250, -356.7845633553585003 ) ) ;
#13540 = CIRCLE ( 'NONE', #10600, 8.025000000000003908 ) ;
#13541 = CARTESIAN_POINT ( 'NONE',  ( 776.9254006560222479, -356.1908817542432075, -314.8983024940802125 ) ) ;
#13543 = CARTESIAN_POINT ( 'NONE',  ( 760.7433823573367135, -444.0090635724249069, 355.9930595647440441 ) ) ;
#13542 = CARTESIAN_POINT ( 'NONE',  ( 781.8018195045266339, -118.2709662947837899, 365.1927285166406705 ) ) ;
#13544 = CARTESIAN_POINT ( 'NONE',  ( 779.4709603349208464, -96.35105083532370429, 314.7162404726379918 ) ) ;
#13547 = CARTESIAN_POINT ( 'NONE',  ( 773.7943932421234194, -359.8055962898683333, 305.5313806188329409 ) ) ;
#13546 = DIRECTION ( 'NONE',  ( -1.000000000000000000, -0.000000000000000000, 0.000000000000000000 ) ) ;
#13545 = LINE ( 'NONE', #2918, #40273 ) ;
#13548 = CARTESIAN_POINT ( 'NONE',  ( 793.0897708529556667, -342.5545181178796952, -361.3366627262616362 ) ) ;
#13549 = CARTESIAN_POINT ( 'NONE',  ( 797.8594530101008786, -373.5436935675101040, -322.1405469898980982 ) ) ;
#13550 = CARTESIAN_POINT ( 'NONE',  ( 778.7629533639073998, -128.7363362996984790, -375.0009284576466371 ) ) ;
#13551 = EDGE_CURVE ( 'NONE', #28289, #4399, #10246, .T. ) ;
#13552 = CARTESIAN_POINT ( 'NONE',  ( 800.9747183278959710, -444.9982390220554862, 311.9810565676471583 ) ) ;
#13553 = MECHANICAL_DESIGN_GEOMETRIC_PRESENTATION_REPRESENTATION (  '', ( #16474 ), #44500 ) ;
#13554 = DIRECTION ( 'NONE',  ( 0.000000000000000000, -0.6438296778008192334, -0.7651688349527138167 ) ) ;
#13555 = CARTESIAN_POINT ( 'NONE',  ( 756.1348686366196716, -305.2601417444139429, -347.5531968255698416 ) ) ;
#13556 = CARTESIAN_POINT ( 'NONE',  ( 786.2694204179717872, -165.2817908451529547, -305.1769319972829067 ) ) ;
#13557 = CARTESIAN_POINT ( 'NONE',  ( 927.9999999999992042, 154.9999999999998863, 350.0000000000000000 ) ) ;
#13558 = CARTESIAN_POINT ( 'NONE',  ( -199.6009925648704098, 290.0000000000001137, -274.9999999999999432 ) ) ;
#13559 = CARTESIAN_POINT ( 'NONE',  ( 763.0428371773158460, -347.4636090269705733, 358.7617431975195359 ) ) ;
#13560 = CARTESIAN_POINT ( 'NONE',  ( 802.2119215644370342, -294.0090635724253048, 367.5423716828165084 ) ) ;
#13561 = CARTESIAN_POINT ( 'NONE',  ( 814.2001403089898304, -161.3618753856927697, -347.4397851343538264 ) ) ;
#13562 = DIRECTION ( 'NONE',  ( 0.000000000000000000, 0.000000000000000000, 1.000000000000000000 ) ) ;
#13563 = CARTESIAN_POINT ( 'NONE',  ( 745.1792804349281596, -110.1908817542440033, 343.7566961878542884 ) ) ;
#13564 = CARTESIAN_POINT ( 'NONE',  ( 814.9108240113580450, -304.2709662947832499, -337.5031285880265273 ) ) ;
#13565 = DIRECTION ( 'NONE',  ( -1.000000000000000000, 0.000000000000000000, 0.000000000000000000 ) ) ;
#13566 = CYLINDRICAL_SURFACE ( 'NONE', #24942, 2.749999999999863665 ) ;
#13567 = CARTESIAN_POINT ( 'NONE',  ( 759.7806653035534055, -198.9982390220562252, 324.8639956371180801 ) ) ;
#13568 = EDGE_LOOP ( 'NONE', ( #29071, #26926, #30510, #6299 ) ) ;
#13569 = AXIS2_PLACEMENT_3D ( 'NONE', #24558, #38674, #18574 ) ;
#13570 = CARTESIAN_POINT ( 'NONE',  ( 788.6739635108323228, -439.6454272087884760, 373.9316612368139090 ) ) ;
#13571 = CARTESIAN_POINT ( 'NONE',  ( 811.6461892240364477, -364.7146871989592114, -324.1737431748509835 ) ) ;
#13572 = CARTESIAN_POINT ( 'NONE',  ( 749.2812353651451076, -126.4527844766019626, -323.2262854647983090 ) ) ;
#13573 = CARTESIAN_POINT ( 'NONE',  ( 755.8894580844503253, -63.82724539060779279, 332.3691319403863531 ) ) ;
#13574 = CARTESIAN_POINT ( 'NONE',  ( 808.3070685750230950, -402.9982390220555430, -361.1904061080339261 ) ) ;
#13575 = FACE_OUTER_BOUND ( 'NONE', #22685, .T. ) ;
#13576 = CARTESIAN_POINT ( 'NONE',  ( 794.1144889064781864, -442.1692326535044231, 360.9840315886528401 ) ) ;
#13577 = ORIENTED_EDGE ( 'NONE', *, *, #10862, .T. ) ;
#13578 = CARTESIAN_POINT ( 'NONE',  ( 815.0009284576459549, -150.3510508353235480, -338.7629533639073429 ) ) ;
#13579 = DIRECTION ( 'NONE',  ( 1.000000000000000000, -0.000000000000000000, -0.000000000000000000 ) ) ;
#13580 = CARTESIAN_POINT ( 'NONE',  ( 788.7631598425961101, -265.4419599262323004, 305.7194118038759143 ) ) ;
#13581 = CARTESIAN_POINT ( 'NONE',  ( 802.1676090361155502, -110.6346026584201923, 327.8955696845344505 ) ) ;
#13582 = ORIENTED_EDGE ( 'NONE', *, *, #31883, .F. ) ;
#13583 = AXIS2_PLACEMENT_3D ( 'NONE', #25244, #31718, #17875 ) ;
#13584 = CARTESIAN_POINT ( 'NONE',  ( 774.6858677611749044, -273.7255117493288026, 315.5713283507209894 ) ) ;
#13585 = CARTESIAN_POINT ( 'NONE',  ( 763.0537975583475827, -0.4527844766023628176, -371.0346526505627480 ) ) ;
#13586 = DIRECTION ( 'NONE',  ( -1.000000000000000000, -0.000000000000000000, -0.000000000000000000 ) ) ;
#13587 = ORIENTED_EDGE ( 'NONE', *, *, #20102, .F. ) ;
#13588 = ORIENTED_EDGE ( 'NONE', *, *, #21860, .T. ) ;
#13589 = CARTESIAN_POINT ( 'NONE',  ( 812.3518521366052028, -409.0999726633340288, -326.5853460496235243 ) ) ;
#13590 = CARTESIAN_POINT ( 'NONE',  ( 804.9363028652555840, -40.27096629478405987, 338.2165204200192079 ) ) ;
#13591 = CARTESIAN_POINT ( 'NONE',  ( 765.0180583372156207, -264.9982390220561115, -360.0135310231089534 ) ) ;
#13593 = CARTESIAN_POINT ( 'NONE',  ( 776.2433038121456548, -252.8965053807777394, 374.8207195650711014 ) ) ;
#13592 = CARTESIAN_POINT ( 'NONE',  ( 755.2512626584698410, -367.5436935675102745, 315.2512626584710915 ) ) ;
#13594 = CARTESIAN_POINT ( 'NONE',  ( 801.5560724626406000, -264.5545181178798657, -326.7756240680316182 ) ) ;
#13595 = CARTESIAN_POINT ( 'NONE',  ( 759.9864689768902508, -242.0891481129652618, -354.9819416627836404 ) ) ;
#13596 = CARTESIAN_POINT ( 'NONE',  ( 797.6776695296629214, -403.5436935675101608, -357.6776695296636603 ) ) ;
#13597 = CARTESIAN_POINT ( 'NONE',  ( 794.9819416627830151, -84.99823902205663728, -319.9864689768909898 ) ) ;
#13598 = AXIS2_PLACEMENT_3D ( 'NONE', #41399, #42298, #17367 ) ;
#13599 = CARTESIAN_POINT ( 'NONE',  ( 804.6798772138708955, -231.7255117493288310, 334.6312213355107019 ) ) ;
#13600 = VERTEX_POINT ( 'NONE', #34507 ) ;
#13601 = CARTESIAN_POINT ( 'NONE',  ( 748.9653473494363425, -362.6346026584194533, 356.9462024416521331 ) ) ;
#13602 = DIRECTION ( 'NONE',  ( 0.000000000000000000, 0.000000000000000000, 1.000000000000000000 ) ) ;
#13603 = CARTESIAN_POINT ( 'NONE',  ( 788.6739635108323228, -55.64542720878963422, -373.9316612368139090 ) ) ;
#13604 = PLANE ( 'NONE',  #32976 ) ;
#13605 = CARTESIAN_POINT ( 'NONE',  ( 1238.921997096861332, 430.0000000000002842, -320.0000000000000568 ) ) ;
#13606 = CARTESIAN_POINT ( 'NONE',  ( 804.4086373105744769, -217.6454272087891582, 333.3843516231986541 ) ) ;
#13607 = CARTESIAN_POINT ( 'NONE',  ( 756.5762568750052424, -123.1800572038747106, 348.7366044899774238 ) ) ;
#13608 = VERTEX_POINT ( 'NONE', #13268 ) ;
#13609 = CARTESIAN_POINT ( 'NONE',  ( 798.5707757039680246, -29.46360902697153250, -356.7845633553585003 ) ) ;
#13610 = CARTESIAN_POINT ( 'NONE',  ( 777.4774526936600978, -82.27096629478390355, -304.7301800767028226 ) ) ;
#13611 = CARTESIAN_POINT ( 'NONE',  ( 789.9200121543843807, -289.9874144716866908, 317.0176451133914384 ) ) ;
#13612 = CARTESIAN_POINT ( 'NONE',  ( 785.3687786644884454, -419.3618753856918033, -315.3201227861279676 ) ) ;
#13613 = CARTESIAN_POINT ( 'NONE',  ( 791.9812246680005501, -44.63460265842040542, -361.9419747391813189 ) ) ;
#13614 = AXIS2_PLACEMENT_3D ( 'NONE', #39947, #682, #21688 ) ;
#13615 = CARTESIAN_POINT ( 'NONE',  ( 805.6418435158337843, -5.463609026971610660, 363.8556311672236916 ) ) ;
#13616 = CARTESIAN_POINT ( 'NONE',  ( 755.2512626584698410, -199.5436935675108430, -315.2512626584710915 ) ) ;
#13617 = AXIS2_PLACEMENT_3D ( 'NONE', #24345, #19757, #38449 ) ;
#13618 = CARTESIAN_POINT ( 'NONE',  ( 763.0537975583475827, -168.4527844766018347, 371.0346526505627480 ) ) ;
#13619 = CARTESIAN_POINT ( 'NONE',  ( 792.1044303154645831, -84.45278447660206211, 317.8323909638837677 ) ) ;
#13620 = LINE ( 'NONE', #38338, #15871 ) ;
#13621 = LINE ( 'NONE', #38556, #38732 ) ;
#13622 = CARTESIAN_POINT ( 'NONE',  ( 814.8230680027162407, -269.8055962898686175, -333.7305795820267917 ) ) ;
#13623 = CARTESIAN_POINT ( 'NONE',  ( 786.2694204179717872, -429.2817908451521021, 305.1769319972829067 ) ) ;
#13624 = CARTESIAN_POINT ( 'NONE',  ( 755.2512626584698410, -271.5436935675106156, -315.2512626584710915 ) ) ;
#13625 = DIRECTION ( 'NONE',  ( 0.000000000000000000, 0.000000000000000000, -1.000000000000000000 ) ) ;
#13626 = CARTESIAN_POINT ( 'NONE',  ( 810.7187646348534145, -402.4527844766010389, 356.7737145352016341 ) ) ;
#13627 = CARTESIAN_POINT ( 'NONE',  ( 749.2812353651451076, -30.45278447660226817, 323.2262854647983090 ) ) ;
#13628 = CARTESIAN_POINT ( 'NONE',  ( 800.0135310231082713, -374.0891481129647786, -325.0180583372163028 ) ) ;
#13629 = VECTOR ( 'NONE', #30537, 1000.000000000000000 ) ;
#13630 = CARTESIAN_POINT ( 'NONE',  ( 802.7791456095903868, -4.714687198960358039, 329.0155153010375102 ) ) ;
#13631 = CARTESIAN_POINT ( 'NONE',  ( 766.5853460496234675, -61.98741447168745822, -372.3518521366060554 ) ) ;
#13632 = CARTESIAN_POINT ( 'NONE',  ( 790.8726784830453198, -154.7146871989598935, -362.5472867521010585 ) ) ;
#13633 = CARTESIAN_POINT ( 'NONE',  ( 744.8212110874229666, -186.8965053807779668, 336.2046728542121627 ) ) ;
#13634 = CARTESIAN_POINT ( 'NONE',  ( 756.5762568750052424, -3.180057203875080063, 348.7366044899774238 ) ) ;
#13635 = CARTESIAN_POINT ( 'NONE',  ( 807.5423716828161105, -177.0783235625961538, 362.2119215644372048 ) ) ;
#13636 = ORIENTED_EDGE ( 'NONE', *, *, #109, .T. ) ;
#13637 = CARTESIAN_POINT ( 'NONE',  ( 801.9419747391806368, -66.45278447660216159, -351.9812246680014027 ) ) ;
#13638 = CARTESIAN_POINT ( 'NONE',  ( 786.6156483768007774, -193.4419599262325278, -315.5913626894246136 ) ) ;
#13639 = CARTESIAN_POINT ( 'NONE',  ( 758.0580252608178853, -150.4527844766018916, 328.0187753319985404 ) ) ;
#13640 = ADVANCED_FACE ( 'NONE', ( #34727 ), #38658, .T. ) ;
#13641 = CARTESIAN_POINT ( 'NONE',  ( 744.8212110874229666, 5.103494619221427442, -336.2046728542121627 ) ) ;
#13642 = CARTESIAN_POINT ( 'NONE',  ( 754.8072714833583632, -292.8164208402378108, 338.1981804954721156 ) ) ;
#13643 = DIRECTION ( 'NONE',  ( -0.000000000000000000, -0.000000000000000000, 1.000000000000000000 ) ) ;
#13644 = ORIENTED_EDGE ( 'NONE', *, *, #39646, .F. ) ;
#13645 = CARTESIAN_POINT ( 'NONE',  ( 803.8651313633788504, -5.260141744414903897, 332.4468031744301015 ) ) ;
#13646 = CARTESIAN_POINT ( 'NONE',  ( 747.6481478633932056, -325.0999726633342561, -353.4146539503763620 ) ) ;
#13647 = CONICAL_SURFACE ( 'NONE', #24710, 8.025000000000003908, 0.7853981633974482790 ) ;
#13648 = EDGE_CURVE ( 'NONE', #4330, #43869, #42119, .T. ) ;
#13649 = CIRCLE ( 'NONE', #43864, 30.00000000000008171 ) ;
#13650 = CARTESIAN_POINT ( 'NONE',  ( 811.0346526505617248, -254.6346026584197091, 323.0537975583478101 ) ) ;
#13651 = CARTESIAN_POINT ( 'NONE',  ( 804.4086373105744769, -337.6454272087888171, 333.3843516231986541 ) ) ;
#13652 = CARTESIAN_POINT ( 'NONE',  ( 784.0799538623451781, -419.8055962898681059, 364.6971507214555572 ) ) ;
#13653 = CARTESIAN_POINT ( 'NONE',  ( 773.4516893846965786, -139.6454272087893571, -315.8398074228977066 ) ) ;
#13654 = CARTESIAN_POINT ( 'NONE',  ( 788.7366044899766848, -155.9073299311473306, -316.5762568750059813 ) ) ;
#13655 = CARTESIAN_POINT ( 'NONE',  ( 803.4237431249931660, -303.1800572038740711, -331.2633955100225194 ) ) ;
#13656 = ORIENTED_EDGE ( 'NONE', *, *, #18237, .T. ) ;
#13657 = CARTESIAN_POINT ( 'NONE',  ( 803.8651313633788504, -341.2601417444138292, 332.4468031744301015 ) ) ;
#13658 = DIRECTION ( 'NONE',  ( 0.000000000000000000, 0.000000000000000000, 1.000000000000000000 ) ) ;
#13659 = AXIS2_PLACEMENT_3D ( 'NONE', #42767, #42992, #18309 ) ;
#13660 = CARTESIAN_POINT ( 'NONE',  ( 757.0176451133909268, -133.0999726633348246, 349.9200121543848354 ) ) ;
#13661 = CARTESIAN_POINT ( 'NONE',  ( 788.8264449731200330, 2.819942796124898177, 363.6646147819171233 ) ) ;
#13662 = ORIENTED_EDGE ( 'NONE', *, *, #19046, .T. ) ;
#13663 = CARTESIAN_POINT ( 'NONE',  ( 762.1177392798416577, -378.5545181178795247, -309.8865473780659272 ) ) ;
#13664 =( GEOMETRIC_REPRESENTATION_CONTEXT ( 3 ) GLOBAL_UNCERTAINTY_ASSIGNED_CONTEXT ( ( #7979 ) ) GLOBAL_UNIT_ASSIGNED_CONTEXT ( ( #38802, #39253, #18005 ) ) REPRESENTATION_CONTEXT ( 'NONE', 'WORKASPACE' ) );
#13665 = LINE ( 'NONE', #20800, #18841 ) ;
#13666 = ADVANCED_FACE ( 'NONE', ( #23857 ), #37973, .F. ) ;
#13667 = CARTESIAN_POINT ( 'NONE',  ( 771.3260364891663130, -235.6454272087890729, 306.0683387631859773 ) ) ;
#13668 = CARTESIAN_POINT ( 'NONE',  ( 795.9930595647434757, -195.0783235625961538, 320.7433823573372820 ) ) ;
#13669 = CARTESIAN_POINT ( 'NONE',  ( 768.0187753319979720, -344.6346026584195101, -318.0580252608186242 ) ) ;
#13670 = ADVANCED_FACE ( 'NONE', ( #31035, #35189 ), #45134, .T. ) ;
#13671 = DIRECTION ( 'NONE',  ( 0.000000000000000000, -0.000000000000000000, -1.000000000000000000 ) ) ;
#13672 = CARTESIAN_POINT ( 'NONE',  ( 755.3028492785439312, -231.2817908451527558, -335.9200461376539693 ) ) ;
#13673 = CARTESIAN_POINT ( 'NONE',  ( 767.7687537140311633, -71.90732993114760063, 372.7932403749916830 ) ) ;
#13674 = CARTESIAN_POINT ( 'NONE',  ( 767.9999999999992042, 205.0000000000000568, -339.9999999999999432 ) ) ;
#13676 = AXIS2_PLACEMENT_3D ( 'NONE', #31786, #30715, #32013 ) ;
#13675 = CARTESIAN_POINT ( 'NONE',  ( 812.7932403749906598, -423.1800572038737300, -327.7687537140311633 ) ) ;
#13677 = LINE ( 'NONE', #3739, #12150 ) ;
#13678 = AXIS2_PLACEMENT_3D ( 'NONE', #36132, #35660, #4276 ) ;
#13679 = CARTESIAN_POINT ( 'NONE',  ( 776.2046728542105711, -356.1908817542432075, 304.8212110874238761 ) ) ;
#13680 = CARTESIAN_POINT ( 'NONE',  ( 809.8718804791541288, -453.2309196406925480, -337.2303869152726179 ) ) ;
#13681 = CARTESIAN_POINT ( 'NONE',  ( 796.9462024416508257, -276.4527844766013800, 308.9653473494370246 ) ) ;
#13682 = CARTESIAN_POINT ( 'NONE',  ( 777.4774526936600978, -58.27096629478398171, -304.7301800767027657 ) ) ;
#13683 = CARTESIAN_POINT ( 'NONE',  ( 788.8264449731200330, -285.1800572038740711, -363.6646147819171233 ) ) ;
#13684 = CIRCLE ( 'NONE', #43902, 7.999999999999896083 ) ;
#13685 = CYLINDRICAL_SURFACE ( 'NONE', #41695, 10.00000000000000888 ) ;
#13686 = CARTESIAN_POINT ( 'NONE',  ( 762.1405469898971887, -409.5436935675101040, 357.8594530101015607 ) ) ;
#13687 = CARTESIAN_POINT ( 'NONE',  ( 755.1538015810308480, -158.1908817542438612, 343.0433043558613804 ) ) ;
#13688 = CARTESIAN_POINT ( 'NONE',  ( 746.4236121716829757, -15.82724539060794200, -328.8385539511384650 ) ) ;
#13689 = CARTESIAN_POINT ( 'NONE',  ( 766.7756240680305382, -62.53286901714199786, -361.5560724626415663 ) ) ;
#13690 = CARTESIAN_POINT ( 'NONE',  ( 783.7566961878529810, -48.89650538077840025, 305.1792804349288417 ) ) ;
#13691 = CARTESIAN_POINT ( 'NONE',  ( 774.6312213355098493, -383.3618753856920875, 364.6798772138717482 ) ) ;
#13692 = FACE_OUTER_BOUND ( 'NONE', #5737, .T. ) ;
#13693 = ADVANCED_FACE ( 'NONE', ( #41670 ), #24093, .F. ) ;
#13694 = CARTESIAN_POINT ( 'NONE',  ( 774.6858677611749044, -441.7255117493282910, 315.5713283507209894 ) ) ;
#13695 = VERTEX_POINT ( 'NONE', #45603 ) ;
#13696 = CARTESIAN_POINT ( 'NONE',  ( 788.7366044899766848, -59.90732993114762905, -316.5762568750059813 ) ) ;
#13697 = EDGE_CURVE ( 'NONE', #31813, #12399, #27805, .T. ) ;
#13698 = CARTESIAN_POINT ( 'NONE',  ( 754.8983024940795303, -354.8965053807774552, -336.9254006560228163 ) ) ;
#13700 = CARTESIAN_POINT ( 'NONE',  ( 804.6798772138710092, -183.7255117493290300, 334.6312213355106451 ) ) ;
#13699 = CARTESIAN_POINT ( 'NONE',  ( 785.3141322388236176, -237.7255117493289163, 364.4286716492789537 ) ) ;
#13701 = ORIENTED_EDGE ( 'NONE', *, *, #22138, .F. ) ;
#13702 = AXIS2_PLACEMENT_3D ( 'NONE', #42588, #31498, #21549 ) ;
#13703 = CARTESIAN_POINT ( 'NONE',  ( 811.6461892240364477, -388.7146871989592114, -324.1737431748509835 ) ) ;
#13704 = CARTESIAN_POINT ( 'NONE',  ( -37.63011601220122770, -501.1515549466498669, -368.0974687824633520 ) ) ;
#13705 = EDGE_LOOP ( 'NONE', ( #5815, #22452, #37020, #17621 ) ) ;
#13706 = CARTESIAN_POINT ( 'NONE',  ( 803.4237431249931660, -399.1800572038738437, 331.2633955100225194 ) ) ;
#13707 = ORIENTED_EDGE ( 'NONE', *, *, #8301, .T. ) ;
#13708 = EDGE_CURVE ( 'NONE', #20290, #1691, #17421, .T. ) ;
#13709 = CIRCLE ( 'NONE', #1881, 10.00000000000000888 ) ;
#13710 = EDGE_CURVE ( 'NONE', #25447, #15531, #28025, .T. ) ;
#13711 = CARTESIAN_POINT ( 'NONE',  ( 792.2312462859673587, -203.9073299311471885, -307.2067596250082602 ) ) ;
#13712 = CARTESIAN_POINT ( 'NONE',  ( 763.2262854647970016, -152.6346026584200786, 309.2812353651462445 ) ) ;
#13713 = ORIENTED_EDGE ( 'NONE', *, *, #35022, .T. ) ;
#13714 = CARTESIAN_POINT ( 'NONE',  ( 812.6845335610512393, -199.9874144716870603, 353.5525998758768651 ) ) ;
#13715 = CARTESIAN_POINT ( 'NONE',  ( 759.9864689768902508, -218.0891481129653187, -354.9819416627836404 ) ) ;
#13716 = ORIENTED_EDGE ( 'NONE', *, *, #15084, .F. ) ;
#13717 = CARTESIAN_POINT ( 'NONE',  ( 804.9363028652555840, -376.2709662947829656, -338.2165204200192079 ) ) ;
#13718 = CARTESIAN_POINT ( 'NONE',  ( 764.8639956371174549, -8.089148112965974136, -319.7806653035542013 ) ) ;
#13719 = CIRCLE ( 'NONE', #12229, 7.999999999999785061 ) ;
#13720 = CARTESIAN_POINT ( 'NONE',  ( 793.2243759319678702, -242.5328690171414507, 318.4439275373583200 ) ) ;
#13721 = LINE ( 'NONE', #41665, #8566 ) ;
#13722 = CARTESIAN_POINT ( 'NONE',  ( 789.9999999999992042, 205.0000000000000568, -329.9999999999999432 ) ) ;
#13723 = AXIS2_PLACEMENT_3D ( 'NONE', #31765, #8209, #42393 ) ;
#13724 = PRODUCT ( 'Slot', 'Slot', '', ( #16662 ) ) ;
#13725 = ORIENTED_EDGE ( 'NONE', *, *, #12847, .T. ) ;
#13726 = CARTESIAN_POINT ( 'NONE',  ( 781.8018195045266339, 1.729033705215812011, -365.1927285166406705 ) ) ;
#13727 = DIRECTION ( 'NONE',  ( 0.000000000000000000, 0.000000000000000000, -1.000000000000000000 ) ) ;
#13728 = CARTESIAN_POINT ( 'NONE',  ( 799.9999999999993179, -462.9681489794448339, -370.0000000000000568 ) ) ;
#13729 = VERTEX_POINT ( 'NONE', #23632 ) ;
#13730 = CARTESIAN_POINT ( 'NONE',  ( 815.3608509340175488, -290.7363362996980527, -341.2497674668889545 ) ) ;
#13731 = CARTESIAN_POINT ( 'NONE',  ( 814.8207195650702488, -146.1908817542438896, 336.2433038121456548 ) ) ;
#13733 = CARTESIAN_POINT ( 'NONE',  ( 755.3201227861273992, -219.7255117493289447, -345.3687786644892981 ) ) ;
#13732 = DIRECTION ( 'NONE',  ( 0.000000000000000000, 0.000000000000000000, 1.000000000000000000 ) ) ;
#13734 = CARTESIAN_POINT ( 'NONE',  ( 786.6156483768007774, -385.4419599262319593, -315.5913626894246136 ) ) ;
#13735 = EDGE_CURVE ( 'NONE', #30554, #42559, #37741, .T. ) ;
#13736 = CARTESIAN_POINT ( 'NONE',  ( 831.1634899080286232, 259.9999999999998863, -191.9749999999999943 ) ) ;
#13737 = DIRECTION ( 'NONE',  ( 0.000000000000000000, 0.000000000000000000, 1.000000000000000000 ) ) ;
#13738 = CARTESIAN_POINT ( 'NONE',  ( 802.9823548866075953, -97.09997266333496668, -330.0799878456151077 ) ) ;
#13739 = CARTESIAN_POINT ( 'NONE',  ( 805.6418435158337843, -389.4636090269704027, 363.8556311672236916 ) ) ;
#13740 = DIRECTION ( 'NONE',  ( 0.000000000000000000, 0.3826834323650836756, 0.9238795325112892920 ) ) ;
#13741 = CARTESIAN_POINT ( 'NONE',  ( 800.1688906516307043, 13.83076734649413098, -369.0717654672308186 ) ) ;
#13742 = CARTESIAN_POINT ( 'NONE',  ( 758.8095938919644823, -296.0891481129650629, -311.6929314249762797 ) ) ;
#13743 = LINE ( 'NONE', #321, #3242 ) ;
#13744 = CARTESIAN_POINT ( 'NONE',  ( 781.7834795799800531, 13.18357915976123174, 315.0636971347436202 ) ) ;
#13745 = CARTESIAN_POINT ( 'NONE',  ( 771.2633955100217236, -95.90732993114751537, -363.4237431249939618 ) ) ;
#13746 = AXIS2_PLACEMENT_3D ( 'NONE', #42113, #28019, #13263 ) ;
#13747 = CARTESIAN_POINT ( 'NONE',  ( 807.2620300519052989, -264.0090635724253616, 318.0141637701419768 ) ) ;
#13748 = CARTESIAN_POINT ( 'NONE',  ( 764.3348316497523456, -166.7146871989598367, -308.6759233522265617 ) ) ;
#13749 = CARTESIAN_POINT ( 'NONE',  ( 763.0537975583475827, -192.4527844766016926, 371.0346526505627480 ) ) ;
#13750 = CARTESIAN_POINT ( 'NONE',  ( 804.1009440267234822, 0.5363909730283709099, -314.0944755984392600 ) ) ;
#13751 = CARTESIAN_POINT ( 'NONE',  ( 181.1634899080285948, 260.0000000000000000, -202.7499999999952536 ) ) ;
#13752 = CARTESIAN_POINT ( 'NONE',  ( 804.6798772138708955, -279.7255117493288026, 334.6312213355107019 ) ) ;
#13753 = CARTESIAN_POINT ( 'NONE',  ( 796.1575198192839480, -54.00906357242601530, 359.4546378042384163 ) ) ;
#13754 = CARTESIAN_POINT ( 'NONE',  ( 774.6312213355099630, -431.3618753856918033, -364.6798772138717482 ) ) ;
#13755 = VECTOR ( 'NONE', #25629, 1000.000000000000000 ) ;
#13756 = DIRECTION ( 'NONE',  ( 0.000000000000000000, 0.000000000000000000, -1.000000000000000000 ) ) ;
#13757 = EDGE_CURVE ( 'NONE', #3427, #32578, #41439, .T. ) ;
#13758 = DIRECTION ( 'NONE',  ( 0.000000000000000000, -0.000000000000000000, -1.000000000000000000 ) ) ;
#13760 = CARTESIAN_POINT ( 'NONE',  ( 785.3141322388236176, -309.7255117493287457, 364.4286716492789537 ) ) ;
#13759 = CARTESIAN_POINT ( 'NONE',  ( 805.0264073115434940, -126.3510508353236048, 339.4763451958999099 ) ) ;
#13761 = ORIENTED_EDGE ( 'NONE', *, *, #22981, .F. ) ;
#13762 = VECTOR ( 'NONE', #19614, 1000.000000000000000 ) ;
#13763 = EDGE_CURVE ( 'NONE', #24071, #44488, #7888, .T. ) ;
#13764 = CARTESIAN_POINT ( 'NONE',  ( 796.7845633553578182, -249.6237781080505158, -358.5707757039688204 ) ) ;
#13765 = CARTESIAN_POINT ( 'NONE',  ( 774.6312213355099630, -95.36187538569294020, 364.6798772138717482 ) ) ;
#13766 = CARTESIAN_POINT ( 'NONE',  ( 795.6651683502461765, -274.7146871989594388, -371.3240766477733814 ) ) ;
#13767 = CARTESIAN_POINT ( 'NONE',  ( -858.8365100919713768, 260.0000000000002274, -208.0249999999880970 ) ) ;
#13768 = CARTESIAN_POINT ( 'NONE',  ( 768.8385539511368734, -407.2601417444137155, 306.4236121716840557 ) ) ;
#13769 = VERTEX_POINT ( 'NONE', #19388 ) ;
#13770 = CARTESIAN_POINT ( 'NONE',  ( 790.8726784830453198, -34.71468719896025590, -362.5472867521010585 ) ) ;
#13771 = CARTESIAN_POINT ( 'NONE',  ( 762.3223304703356007, -175.5436935675108998, -322.3223304703362828 ) ) ;
#13772 = CARTESIAN_POINT ( 'NONE',  ( 801.9419747391806368, -210.4527844766016926, -351.9812246680014027 ) ) ;
#13773 = CARTESIAN_POINT ( 'NONE',  ( 803.6646147819161570, -425.9073299311463074, 348.8264449731210561 ) ) ;
#13774 = CARTESIAN_POINT ( 'NONE',  ( 759.0252816721024374, -120.9982390220565378, -368.0189434323527280 ) ) ;
#13775 = CARTESIAN_POINT ( 'NONE',  ( 791.9812246680005501, -92.63460265842026331, -361.9419747391813189 ) ) ;
#13776 = ORIENTED_EDGE ( 'NONE', *, *, #17400, .T. ) ;
#13777 = CARTESIAN_POINT ( 'NONE',  ( 787.5531968255692163, -45.82724539060783542, -316.1348686366205811 ) ) ;
#13778 = AXIS2_PLACEMENT_3D ( 'NONE', #10830, #42234, #37683 ) ;
#13779 = CARTESIAN_POINT ( 'NONE',  ( 796.9571628226829034, -407.4636090269703459, -321.2382568024804641 ) ) ;
#13781 = CARTESIAN_POINT ( 'NONE',  ( 783.0745993439762742, -440.1908817542430370, 365.1016975059196739 ) ) ;
#13780 = CARTESIAN_POINT ( 'NONE',  ( 795.1360043628807261, -116.0891481129656029, 360.2193346964456282 ) ) ;
#13782 = CIRCLE ( 'NONE', #39610, 24.99999999999991118 ) ;
#13785 = CARTESIAN_POINT ( 'NONE',  ( 781.2497674668890113, -348.3510508353228943, 375.3608509340180603 ) ) ;
#13784 = FACE_OUTER_BOUND ( 'NONE', #11618, .T. ) ;
#13783 = CARTESIAN_POINT ( 'NONE',  ( 989.9999999999992042, 47.45399382421947365, -201.9999999999999432 ) ) ;
#13786 = ORIENTED_EDGE ( 'NONE', *, *, #39132, .T. ) ;
#13787 = CARTESIAN_POINT ( 'NONE',  ( 804.4086373105744769, -361.6454272087887603, -333.3843516231986541 ) ) ;
#13788 = CARTESIAN_POINT ( 'NONE',  ( 795.1360043628807261, -356.0891481129647218, -360.2193346964456282 ) ) ;
#13789 = AXIS2_PLACEMENT_3D ( 'NONE', #877, #11281, #21910 ) ;
#13790 = CARTESIAN_POINT ( 'NONE',  ( 813.5763878283155464, -171.8272453906074304, -351.1614460488615350 ) ) ;
#13791 = CARTESIAN_POINT ( 'NONE',  ( 814.2805881961230625, -25.64542720878973014, 331.2368401574024119 ) ) ;
#13792 = AXIS2_PLACEMENT_3D ( 'NONE', #33533, #22682, #19221 ) ;
#13794 = FACE_OUTER_BOUND ( 'NONE', #16209, .T. ) ;
#13793 = CARTESIAN_POINT ( 'NONE',  ( -180.7583438952258916, 294.6698570112193920, -244.9999999999999716 ) ) ;
#13795 = CARTESIAN_POINT ( 'NONE',  ( 802.7791456095903868, -292.7146871989594956, -329.0155153010375102 ) ) ;
#13796 = CARTESIAN_POINT ( 'NONE',  ( -598.8365100919716042, 260.0000000000001705, -199.9999999999899671 ) ) ;
#13797 = CARTESIAN_POINT ( 'NONE',  ( 799.9636004259356241, -142.9181544815166376, -311.2241431872006956 ) ) ;
#13798 = CARTESIAN_POINT ( 'NONE',  ( 441.1634899080286232, 240.0000000000000000, -202.7499999999971010 ) ) ;
#13799 = CARTESIAN_POINT ( 'NONE',  ( 441.1634899080286232, 256.4999999999999432, -197.2499999999973284 ) ) ;
#13800 = CARTESIAN_POINT ( 'NONE',  ( 804.1105419155481968, -363.8272453906068336, 347.6308680596136469 ) ) ;
#13801 = CARTESIAN_POINT ( 'NONE',  ( 755.8990559732751535, -323.4636090269706301, 365.9055244015606831 ) ) ;
#13802 = CARTESIAN_POINT ( 'NONE',  ( 787.4397851343537695, -189.7255117493290300, -374.2001403089903988 ) ) ;
#13803 = DIRECTION ( 'NONE',  ( 0.000000000000000000, 0.000000000000000000, -1.000000000000000000 ) ) ;
#13804 = CARTESIAN_POINT ( 'NONE',  ( 804.1009440267234822, -119.4636090269712554, 314.0944755984392600 ) ) ;
#13805 = CARTESIAN_POINT ( 'NONE',  ( 751.6929314249748586, -294.9982390220560546, -318.8095938919659034 ) ) ;
#13806 = CARTESIAN_POINT ( 'NONE',  ( 919.9999999999993179, 154.9999999999998863, -360.0000000000000000 ) ) ;
#13807 = CYLINDRICAL_SURFACE ( 'NONE', #29383, 6.118999999999985562 ) ;
#13808 = CARTESIAN_POINT ( 'NONE',  ( 803.6646147819161570, -185.9073299311472454, 348.8264449731210561 ) ) ;
#13809 = ORIENTED_EDGE ( 'NONE', *, *, #1475, .F. ) ;
#13810 = CARTESIAN_POINT ( 'NONE',  ( 783.7953271457878373, -440.1908817542430370, 375.1787889125761239 ) ) ;
#13811 = CARTESIAN_POINT ( 'NONE',  ( 756.1443688327750579, -381.6237781080500326, -314.3581564841659315 ) ) ;
#13812 = CARTESIAN_POINT ( 'NONE',  ( 796.7737145352015204, -140.6346026584201070, -370.7187646348536987 ) ) ;
#13813 = CARTESIAN_POINT ( 'NONE',  ( 777.4774526936600978, -370.2709662947831362, -304.7301800767027657 ) ) ;
#13814 = PLANE ( 'NONE',  #15104 ) ;
#13815 = CARTESIAN_POINT ( 'NONE',  ( 800.1688906516307043, 13.83076734649413098, 369.0717654672308186 ) ) ;
#13816 = ORIENTED_EDGE ( 'NONE', *, *, #14766, .T. ) ;
#13817 = AXIS2_PLACEMENT_3D ( 'NONE', #200, #14292, #28365 ) ;
#13818 = CARTESIAN_POINT ( 'NONE',  ( 807.5423716828161105, -153.0783235625962675, -362.2119215644372048 ) ) ;
#13819 = CARTESIAN_POINT ( 'NONE',  ( 808.7758568127978833, -316.1692326535048210, 320.0363995740631822 ) ) ;
#13820 = CARTESIAN_POINT ( 'NONE',  ( 771.2633955100217236, -119.9073299311474443, 363.4237431249939618 ) ) ;
#13821 = EDGE_LOOP ( 'NONE', ( #11383, #13644, #6035, #34359 ) ) ;
#13822 = VECTOR ( 'NONE', #17631, 1000.000000000000000 ) ;
#13823 = CARTESIAN_POINT ( 'NONE',  ( 797.6776695296629214, -307.5436935675104451, 357.6776695296636603 ) ) ;
#13824 = CIRCLE ( 'NONE', #45298, 10.00000000000000888 ) ;
#13825 = CARTESIAN_POINT ( 'NONE',  ( 772.4837098697144029, -23.36187538569318889, -374.5518280994205611 ) ) ;
#13826 = DIRECTION ( 'NONE',  ( 0.000000000000000000, 0.000000000000000000, -1.000000000000000000 ) ) ;
#13827 = EDGE_LOOP ( 'NONE', ( #24770, #32740 ) ) ;
#13828 = CARTESIAN_POINT ( 'NONE',  ( 766.4474001241216001, -427.0999726633338582, -307.3154664389482491 ) ) ;
#13829 = ORIENTED_EDGE ( 'NONE', *, *, #32525, .F. ) ;
#13830 = CARTESIAN_POINT ( 'NONE',  ( 802.1676090361156639, -38.63460265842041252, 327.8955696845344505 ) ) ;
#13831 = CARTESIAN_POINT ( 'NONE',  ( 771.1735550268778070, -273.1800572038742985, -316.3353852180827630 ) ) ;
#13833 = CARTESIAN_POINT ( 'NONE',  ( 756.1443688327750579, -237.6237781080505442, 314.3581564841659315 ) ) ;
#13832 = CARTESIAN_POINT ( 'NONE',  ( 751.6929314249750860, -366.9982390220557136, 318.8095938919659034 ) ) ;
#13834 = CARTESIAN_POINT ( 'NONE',  ( 790.0220218866281812, -247.0999726633344835, -363.2186876482849129 ) ) ;
#13835 = CARTESIAN_POINT ( 'NONE',  ( 755.0636971347428243, -268.2709662947833067, -341.7834795799807353 ) ) ;
#13836 = DIRECTION ( 'NONE',  ( -0.000000000000000000, 1.000000000000000000, -0.000000000000000000 ) ) ;
#13837 = CARTESIAN_POINT ( 'NONE',  ( 767.8955696845333705, -96.45278447660203369, -362.1676090361162323 ) ) ;
#13838 = CARTESIAN_POINT ( 'NONE',  ( 754.8072714833581358, -244.8164208402378961, 338.1981804954720587 ) ) ;
#13839 = CARTESIAN_POINT ( 'NONE',  ( 796.9462024416508257, -396.4527844766010389, 308.9653473494370246 ) ) ;
#13840 = CARTESIAN_POINT ( 'NONE',  ( 200.7583438952259485, 394.6698570112193920, -274.9999999999999432 ) ) ;
#13841 = CARTESIAN_POINT ( 'NONE',  ( 811.3240766477731540, -52.37269993606237506, -355.6651683502462902 ) ) ;
#13842 = DIRECTION ( 'NONE',  ( -1.000000000000000000, 0.000000000000000000, 0.000000000000000000 ) ) ;
#13843 = VECTOR ( 'NONE', #44048, 1000.000000000000000 ) ;
#13844 = DIRECTION ( 'NONE',  ( -0.000000000000000000, -0.7517448203044211352, 0.6594541114781783397 ) ) ;
#13845 = CARTESIAN_POINT ( 'NONE',  ( 804.6971507214547046, -219.2817908451527558, 344.0799538623459739 ) ) ;
#13846 = CARTESIAN_POINT ( 'NONE',  ( 755.0636971347428243, -124.2709662947837899, 341.7834795799807353 ) ) ;
#13847 = ORIENTED_EDGE ( 'NONE', *, *, #28565, .T. ) ;
#13848 = CARTESIAN_POINT ( 'NONE',  ( 802.5472867521000353, -4.372699936062523385, -350.8726784830461156 ) ) ;
#13849 = CARTESIAN_POINT ( 'NONE',  ( 748.9653473494365699, -74.63460265842030594, -356.9462024416520762 ) ) ;
#13850 = CARTESIAN_POINT ( 'NONE',  ( 770.0799878456142551, -301.9874144716867477, 362.9823548866085616 ) ) ;
#13851 = AXIS2_PLACEMENT_3D ( 'NONE', #43906, #44134, #26359 ) ;
#13852 = CARTESIAN_POINT ( 'NONE',  ( 756.5762568750052424, -435.1800572038737869, -348.7366044899774238 ) ) ;
#13853 = CARTESIAN_POINT ( 'NONE',  ( 771.3260364891663130, -19.64542720878974791, 306.0683387631859773 ) ) ;
#13854 = CARTESIAN_POINT ( 'NONE',  ( 815.2698199232961542, -208.8164208402380666, -342.5225473063383106 ) ) ;
#13855 = CARTESIAN_POINT ( 'NONE',  ( 751.9810565676468741, -170.0891481129654608, 360.9747183278973921 ) ) ;
#13856 = CARTESIAN_POINT ( 'NONE',  ( 804.4286716492782716, -65.36187538569306810, 345.3141322388244703 ) ) ;
#13857 = FACE_OUTER_BOUND ( 'NONE', #5231, .T. ) ;
#13858 = CARTESIAN_POINT ( 'NONE',  ( 744.9990715423526808, -258.3510508353231785, -341.2370466360926002 ) ) ;
#13859 = CARTESIAN_POINT ( 'NONE',  ( 810.4231160770870019, -432.5545181178793541, 321.9338519418446936 ) ) ;
#13860 = CARTESIAN_POINT ( 'NONE',  ( 747.2067596250078623, -291.1800572038741848, -352.2312462859687230 ) ) ;
#13861 = CARTESIAN_POINT ( 'NONE',  ( 809.6099558218720631, -452.9681489794449476, 335.1781210895659342 ) ) ;
#13862 = CARTESIAN_POINT ( 'NONE',  ( 783.0433043558608688, -360.8965053807773984, 315.1538015810313027 ) ) ;
#13863 = CARTESIAN_POINT ( 'NONE',  ( 763.2262854647970016, -56.63460265842036279, 309.2812353651462445 ) ) ;
#13864 = CARTESIAN_POINT ( 'NONE',  ( 805.9055244015594326, -27.62377810805120149, -315.8990559732753240 ) ) ;
#13865 = CARTESIAN_POINT ( 'NONE',  ( 762.1405469898971887, -385.5436935675102745, -357.8594530101015607 ) ) ;
#13866 = CARTESIAN_POINT ( 'NONE',  ( 798.7617431975189675, -27.62377810805120149, 323.0428371773161871 ) ) ;
#13867 = CARTESIAN_POINT ( 'NONE',  ( 781.7834795799800531, -202.8164208402380950, -315.0636971347436202 ) ) ;
#13868 = CARTESIAN_POINT ( 'NONE',  ( 807.5423716828161105, -33.07832356259662987, -362.2119215644372048 ) ) ;
#13869 = CARTESIAN_POINT ( 'NONE',  ( 804.1601925771018387, -199.4419599262324709, -346.5483106153029098 ) ) ;
#13870 = CARTESIAN_POINT ( 'NONE',  ( 748.3538107759620743, -160.7146871989598651, 355.8262568251490165 ) ) ;
#13871 = CARTESIAN_POINT ( 'NONE',  ( 762.1405469898973024, -1.543693567511449594, 357.8594530101016176 ) ) ;
#13872 = ORIENTED_EDGE ( 'NONE', *, *, #12547, .T. ) ;
#13873 = CARTESIAN_POINT ( 'NONE',  ( 775.9200461376533440, -191.8055962898689017, -315.3028492785443291 ) ) ;
#13874 = CARTESIAN_POINT ( 'NONE',  ( 758.0580252608178853, -198.4527844766017495, 328.0187753319985404 ) ) ;
#13875 = CARTESIAN_POINT ( 'NONE',  ( 811.6461892240364477, -28.71468719896028077, -324.1737431748509835 ) ) ;
#13876 = CARTESIAN_POINT ( 'NONE',  ( 759.9864689768902508, -314.0891481129650629, 354.9819416627836404 ) ) ;
#13877 = CARTESIAN_POINT ( 'NONE',  ( 1238.921997096861332, 579.9999999999998863, -360.0000000000000000 ) ) ;
#13878 = ORIENTED_EDGE ( 'NONE', *, *, #16833, .T. ) ;
#13879 = CARTESIAN_POINT ( 'NONE',  ( 786.6156483768007774, -49.44195992623295410, 315.5913626894246136 ) ) ;
#13880 = CARTESIAN_POINT ( 'NONE',  ( 809.0717654672305343, -292.9181544815162397, -360.1688906516309885 ) ) ;
#13881 = VECTOR ( 'NONE', #24179, 1000.000000000000000 ) ;
#13882 = CARTESIAN_POINT ( 'NONE',  ( 763.2262854647970016, -272.6346026584196807, 309.2812353651462445 ) ) ;
#13883 = CARTESIAN_POINT ( 'NONE',  ( 757.4527132478984868, -328.3726999360615650, 329.1273215169538844 ) ) ;
#13884 = CARTESIAN_POINT ( 'NONE',  ( 805.1016975059191054, -438.8965053807771710, 343.0745993439771837 ) ) ;
#13885 = EDGE_CURVE ( 'NONE', #4508, #35556, #1820, .T. ) ;
#13886 = CARTESIAN_POINT ( 'NONE',  ( 779.4763451958990572, -152.7363362996983938, -365.0264073115438919 ) ) ;
#13887 = CARTESIAN_POINT ( 'NONE',  ( 800.0135310231082713, -134.0891481129655745, -325.0180583372163028 ) ) ;
#13888 = CARTESIAN_POINT ( 'NONE',  ( 800.0135310231082713, -350.0891481129648923, -325.0180583372163028 ) ) ;
#13889 = VERTEX_POINT ( 'NONE', #14410 ) ;
#13890 = CARTESIAN_POINT ( 'NONE',  ( 758.8095938919642549, -248.0891481129651481, 311.6929314249763365 ) ) ;
#13891 = CARTESIAN_POINT ( 'NONE',  ( 805.0264073115434940, -342.3510508353228943, 339.4763451958999099 ) ) ;
#13892 = CARTESIAN_POINT ( 'NONE',  ( 999.9999999999992042, 249.5857864376267798, -200.4142135623730496 ) ) ;
#13893 = CARTESIAN_POINT ( 'NONE',  ( 772.4468031744293057, -129.8272453906075725, 363.8651313633793620 ) ) ;
#13894 = CARTESIAN_POINT ( 'NONE',  ( 795.1360043628807261, -20.08914811296592973, 360.2193346964456282 ) ) ;
#13895 = ORIENTED_EDGE ( 'NONE', *, *, #25313, .T. ) ;
#13896 = CARTESIAN_POINT ( 'NONE',  ( 802.2119215644370342, -366.0090635724250774, -367.5423716828165084 ) ) ;
#13897 = DIRECTION ( 'NONE',  ( 0.000000000000000000, -0.6438296778008192334, 0.7651688349527138167 ) ) ;
#13898 = CARTESIAN_POINT ( 'NONE',  ( 760.7433823573367135, -228.0090635724254753, 355.9930595647440441 ) ) ;
#13899 = CARTESIAN_POINT ( 'NONE',  ( 793.5525998758768083, -223.0999726633346256, 372.6845335610516941 ) ) ;
#13900 = CARTESIAN_POINT ( 'NONE',  ( 804.9511171171677688, -173.8055962898689302, 335.8780910478229202 ) ) ;
#13901 = CARTESIAN_POINT ( 'NONE',  ( 788.8264449731200330, -333.1800572038740142, -363.6646147819171233 ) ) ;
#13902 = DIRECTION ( 'NONE',  ( 1.000000000000000000, 0.000000000000000000, 0.000000000000000000 ) ) ;
#13903 = CARTESIAN_POINT ( 'NONE',  ( 755.8894580844503253, -207.8272453906073451, -332.3691319403863531 ) ) ;
#13904 = CARTESIAN_POINT ( 'NONE',  ( 767.7687537140311633, -23.90732993114773919, 372.7932403749916830 ) ) ;
#13905 = CARTESIAN_POINT ( 'NONE',  ( 745.0891759886404770, -76.27096629478394618, 342.4968714119734159 ) ) ;
#13906 = LINE ( 'NONE', #3515, #29881 ) ;
#13907 = CARTESIAN_POINT ( 'NONE',  ( 813.1304606946831655, -425.9073299311463643, -352.3570229623691716 ) ) ;
#13908 = DIRECTION ( 'NONE',  ( -1.000000000000000000, 0.000000000000000000, -0.000000000000000000 ) ) ;
#13909 = AXIS2_PLACEMENT_3D ( 'NONE', #7103, #34107, #6633 ) ;
#13910 = CARTESIAN_POINT ( 'NONE',  ( 815.3608509340175488, -338.7363362996978822, 341.2497674668889545 ) ) ;
#13911 = LINE ( 'NONE', #35366, #39751 ) ;
#13912 = CARTESIAN_POINT ( 'NONE',  ( 782.5225473063381969, -310.2709662947832499, 375.2698199232970637 ) ) ;
#13913 = CARTESIAN_POINT ( 'NONE',  ( 755.2512626584698410, -55.54369356751127640, -315.2512626584710915 ) ) ;
#13914 = ADVANCED_FACE ( 'NONE', ( #4005 ), #36723, .F. ) ;
#13915 = CARTESIAN_POINT ( 'NONE',  ( 764.8639956371174549, -296.0891481129650629, -319.7806653035542013 ) ) ;
#13916 = FACE_BOUND ( 'NONE', #40906, .T. ) ;
#13917 = CARTESIAN_POINT ( 'NONE',  ( 759.9864689768902508, -410.0891481129647218, 354.9819416627836404 ) ) ;
#13918 = CARTESIAN_POINT ( 'NONE',  ( 766.0291762391763086, -154.9181544815165523, 360.7704444035551319 ) ) ;
#13919 = CARTESIAN_POINT ( 'NONE',  ( 764.1737431748507561, -34.37269993606243901, -371.6461892240376415 ) ) ;
#13920 = CARTESIAN_POINT ( 'NONE',  ( 779.4709603349208464, -96.35105083532370429, -314.7162404726379918 ) ) ;
#13921 = CARTESIAN_POINT ( 'NONE',  ( 758.0141637701419768, -63.07832356259653750, 367.2620300519063790 ) ) ;
#13922 = CARTESIAN_POINT ( 'NONE',  ( 791.9812246680005501, -404.6346026584193396, 361.9419747391813189 ) ) ;
#13923 = DIRECTION ( 'NONE',  ( 0.000000000000000000, 0.000000000000000000, -1.000000000000000000 ) ) ;
#13924 = CARTESIAN_POINT ( 'NONE',  ( 771.2633955100217236, -431.9073299311464211, 363.4237431249939618 ) ) ;
#13925 = ORIENTED_EDGE ( 'NONE', *, *, #17371, .F. ) ;
#13926 = CARTESIAN_POINT ( 'NONE',  ( 767.8955696845333705, -48.45278447660219712, -362.1676090361162323 ) ) ;
#13927 = CARTESIAN_POINT ( 'NONE',  ( 761.2382568024794409, -375.6237781080501463, -356.9571628226838129 ) ) ;
#13929 = CARTESIAN_POINT ( 'NONE',  ( 791.9812246680005501, -212.6346026584198796, 361.9419747391813189 ) ) ;
#13928 = CARTESIAN_POINT ( 'NONE',  ( 765.0180583372156207, -216.9982390220562252, 360.0135310231089534 ) ) ;
#13930 = CARTESIAN_POINT ( 'NONE',  ( 788.7631598425961101, -385.4419599262319593, -305.7194118038759143 ) ) ;
#13931 = CARTESIAN_POINT ( 'NONE',  ( 794.9999999999993179, 205.0000000000000568, -255.0000000000000000 ) ) ;
#13932 = ORIENTED_EDGE ( 'NONE', *, *, #23265, .F. ) ;
#13933 = CARTESIAN_POINT ( 'NONE',  ( 762.1405469898971887, -409.5436935675101040, 357.8594530101015607 ) ) ;
#13934 = ORIENTED_EDGE ( 'NONE', *, *, #29702, .F. ) ;
#13935 = CARTESIAN_POINT ( 'NONE',  ( 804.7487373415286811, -259.5436935675106156, -364.7487373415288516 ) ) ;
#13936 = CARTESIAN_POINT ( 'NONE',  ( 777.5031285880264704, -142.8164208402382656, 374.9108240113588408 ) ) ;
#13937 = EDGE_LOOP ( 'NONE', ( #7058, #36807, #3376, #17272, #2863, #4914, #12835, #2912, #34704, #6768, #171, #9339 ) ) ;
#13938 = CARTESIAN_POINT ( 'NONE',  ( 811.6461892240364477, -196.7146871989598083, 324.1737431748509835 ) ) ;
#13939 = CARTESIAN_POINT ( 'NONE',  ( 792.1044303154646968, -204.4527844766016926, -317.8323909638837677 ) ) ;
#13940 = ORIENTED_EDGE ( 'NONE', *, *, #2313, .T. ) ;
#13941 = CIRCLE ( 'NONE', #41979, 2.749999999999863665 ) ;
#13942 = CARTESIAN_POINT ( 'NONE',  ( 804.6798772138708955, -351.7255117493284047, -334.6312213355107019 ) ) ;
#13943 = CARTESIAN_POINT ( 'NONE',  ( 762.3223304703356007, -7.543693567511430942, -322.3223304703362828 ) ) ;
#13944 = CARTESIAN_POINT ( 'NONE',  ( 775.9200461376533440, -215.8055962898687881, 315.3028492785443291 ) ) ;
#13945 = LINE ( 'NONE', #9786, #10771 ) ;
#13946 = DIRECTION ( 'NONE',  ( 0.000000000000000000, 0.6755902076156502511, 0.7372773368101330771 ) ) ;
#13947 = VERTEX_POINT ( 'NONE', #28728 ) ;
#13948 = CARTESIAN_POINT ( 'NONE',  ( 755.3028492785439312, -447.2817908451521021, -335.9200461376539693 ) ) ;
#13949 = LINE ( 'NONE', #24789, #12975 ) ;
#13950 = CARTESIAN_POINT ( 'NONE',  ( -959.5497976682736407, 120.6654763175833693, -209.9999999999999716 ) ) ;
#13951 = ORIENTED_EDGE ( 'NONE', *, *, #7772, .T. ) ;
#13952 = CARTESIAN_POINT ( 'NONE',  ( 810.4231160770870019, -264.5545181178798657, -321.9338519418446936 ) ) ;
#13953 = CARTESIAN_POINT ( 'NONE',  ( 757.7880784355613741, -138.0090635724257311, 312.4576283171834916 ) ) ;
#13955 = CARTESIAN_POINT ( 'NONE',  ( 768.0187753319979720, -224.6346026584198228, -318.0580252608186242 ) ) ;
#13954 = FACE_BOUND ( 'NONE', #14575, .T. ) ;
#13956 = ADVANCED_FACE ( 'NONE', ( #12243, #22848, #25239 ), #39349, .T. ) ;
#13957 = CARTESIAN_POINT ( 'NONE',  ( 772.3691319403857278, -407.2601417444137155, -315.8894580844506663 ) ) ;
#13958 = CARTESIAN_POINT ( 'NONE',  ( 786.4999999999993179, -32.84703287382739489, 757.2634078669103701 ) ) ;
#13959 = FACE_BOUND ( 'NONE', #29557, .T. ) ;
#13960 = CARTESIAN_POINT ( 'NONE',  ( 800.9840315886518738, -100.9181544815167513, -354.1144889064786412 ) ) ;
#13961 = ADVANCED_FACE ( 'NONE', ( #28243, #42589, #32187 ), #10706, .F. ) ;
#13962 = CARTESIAN_POINT ( 'NONE',  ( 768.9521613784389729, -393.8272453906067199, 373.2346286133773106 ) ) ;
#13963 = DIRECTION ( 'NONE',  ( 1.000000000000000000, 0.000000000000000000, -0.000000000000000000 ) ) ;
#13964 = CARTESIAN_POINT ( 'NONE',  ( 789.6640940660590786, -442.9180389616178672, -363.1300863558843162 ) ) ;
#13965 = CARTESIAN_POINT ( 'NONE',  ( 812.7932403749906598, -303.1800572038740711, -327.7687537140311633 ) ) ;
#13966 = CARTESIAN_POINT ( 'NONE',  ( -78.83651009197140525, 260.0000000000000568, -199.9999999999936051 ) ) ;
#13967 = CARTESIAN_POINT ( 'NONE',  ( 771.1735550268778070, 14.81994279612486309, 316.3353852180827630 ) ) ;
#13968 = CARTESIAN_POINT ( 'NONE',  ( 801.9419747391806368, -90.45278447660209054, -351.9812246680014027 ) ) ;
#13969 = CARTESIAN_POINT ( 'NONE',  ( 762.1177392798416577, -258.5545181178799226, 309.8865473780659272 ) ) ;
#13970 = CARTESIAN_POINT ( 'NONE',  ( 791.1614460488616487, -203.2601417444143124, -373.5763878283158874 ) ) ;
#13971 = CARTESIAN_POINT ( 'NONE',  ( 796.7737145352015204, -188.6346026584199365, 370.7187646348536987 ) ) ;
#13972 = CARTESIAN_POINT ( 'NONE',  ( 811.0346526505616112, -446.6346026584189985, -323.0537975583477532 ) ) ;
#13973 = EDGE_CURVE ( 'NONE', #37595, #38147, #14651, .T. ) ;
#13974 = EDGE_CURVE ( 'NONE', #5961, #43956, #35878, .T. ) ;
#13975 = CARTESIAN_POINT ( 'NONE',  ( 799.9999999999993179, 166.4563064324884465, -360.0000000000000000 ) ) ;
#13976 = CARTESIAN_POINT ( 'NONE',  ( 803.4237431249931660, -303.1800572038740711, 331.2633955100225194 ) ) ;
#13977 = CARTESIAN_POINT ( 'NONE',  ( 784.1219089521767955, -93.28179084515315367, 315.0488828828318333 ) ) ;
#13978 = CARTESIAN_POINT ( 'NONE',  ( 754.8072714833581358, -412.8164208402372992, -338.1981804954720587 ) ) ;
#13979 = VECTOR ( 'NONE', #30253, 1000.000000000000000 ) ;
#13980 = CARTESIAN_POINT ( 'NONE',  ( -784.4999999999993179, -544.8427095258973623, -369.9999999999999432 ) ) ;
#13981 = LINE ( 'NONE', #34979, #14415 ) ;
#13983 = CARTESIAN_POINT ( 'NONE',  ( 778.1981804954714335, -322.2709662947830225, 314.8072714833589885 ) ) ;
#13982 = CARTESIAN_POINT ( 'NONE',  ( 759.2295555964440155, -136.1692326535053894, 353.9708237608231229 ) ) ;
#13984 = ORIENTED_EDGE ( 'NONE', *, *, #44480, .F. ) ;
#13985 = CARTESIAN_POINT ( 'NONE',  ( 803.2186876482843445, -271.9874144716868045, -350.0220218866286928 ) ) ;
#13986 = CARTESIAN_POINT ( 'NONE',  ( 778.2165204200184689, -94.81642084023843609, 364.9363028652563230 ) ) ;
#13987 = CARTESIAN_POINT ( 'NONE',  ( 744.8212110874229666, -306.8965053807775689, -336.2046728542121627 ) ) ;
#13988 = CARTESIAN_POINT ( 'NONE',  ( -858.8365100919713768, 256.5000000000002274, -206.1189999999881479 ) ) ;
#13989 = CARTESIAN_POINT ( 'NONE',  ( 808.7758568127978833, -412.1692326535045936, 320.0363995740631822 ) ) ;
#13990 = ADVANCED_FACE ( 'NONE', ( #1386 ), #1603, .F. ) ;
#13991 = ORIENTED_EDGE ( 'NONE', *, *, #44755, .T. ) ;
#13992 = CARTESIAN_POINT ( 'NONE',  ( 759.7806653035534055, -294.9982390220560546, 324.8639956371180801 ) ) ;
#13993 = EDGE_CURVE ( 'NONE', #26697, #34351, #38109, .T. ) ;
#13994 = CARTESIAN_POINT ( 'NONE',  ( 804.9511171171677688, -53.80559628986930676, -335.8780910478229202 ) ) ;
#13995 = CARTESIAN_POINT ( 'NONE',  ( 791.9812246680005501, -164.6346026584200217, -361.9419747391813189 ) ) ;
#13996 = CARTESIAN_POINT ( 'NONE',  ( 759.9864689768902508, -218.0891481129653187, -354.9819416627836404 ) ) ;
#13997 = CARTESIAN_POINT ( 'NONE',  ( 771.2633955100217236, -407.9073299311465348, 363.4237431249939618 ) ) ;
#13998 = CARTESIAN_POINT ( 'NONE',  ( 792.2312462859673587, -155.9073299311473306, -307.2067596250082602 ) ) ;
#13999 = CARTESIAN_POINT ( 'NONE',  ( 765.0180583372156207, -96.99823902205660886, -360.0135310231089534 ) ) ;
#14000 = ORIENTED_EDGE ( 'NONE', *, *, #6611, .T. ) ;
#14001 = CARTESIAN_POINT ( 'NONE',  ( 799.2566176426618085, -384.0090635724249637, -324.0069404352559559 ) ) ;
#14003 = CARTESIAN_POINT ( 'NONE',  ( 755.8894580844503253, -423.8272453906067199, 332.3691319403863531 ) ) ;
#14002 = CARTESIAN_POINT ( 'NONE',  ( 755.0636971347428243, -124.2709662947837899, 341.7834795799807353 ) ) ;
#14004 = CARTESIAN_POINT ( 'NONE',  ( 783.0433043558608688, -120.8965053807781800, 315.1538015810313027 ) ) ;
#14007 = CARTESIAN_POINT ( 'NONE',  ( 744.9990715423526808, -402.3510508353228374, 341.2370466360926002 ) ) ;
#14006 = CYLINDRICAL_SURFACE ( 'NONE', #10007, 2.749999999999863665 ) ;
#14005 = CARTESIAN_POINT ( 'NONE',  ( 787.4999999999992042, -462.9681489794447202, 270.0000000000000568 ) ) ;
#14008 = ORIENTED_EDGE ( 'NONE', *, *, #28981, .T. ) ;
#14009 = CARTESIAN_POINT ( 'NONE',  ( 801.5560724626406000, -360.5545181178796383, -326.7756240680316182 ) ) ;
#14010 = CARTESIAN_POINT ( 'NONE',  ( 758.0580252608178853, -366.4527844766012095, -328.0187753319985404 ) ) ;
#14011 = CARTESIAN_POINT ( 'NONE',  ( 764.1737431748507561, -154.3726999360620198, -371.6461892240376415 ) ) ;
#14012 = EDGE_CURVE ( 'NONE', #32527, #24990, #29570, .T. ) ;
#14013 = CARTESIAN_POINT ( 'NONE',  ( 815.3608509340175488, -26.73633629969882008, 341.2497674668889545 ) ) ;
#14015 = CARTESIAN_POINT ( 'NONE',  ( -78.83651009197140525, 258.0940000000000509, -206.1189999999936049 ) ) ;
#14014 = CARTESIAN_POINT ( 'NONE',  ( 998.9999999999992042, 249.9999999999998863, -200.9999999999999432 ) ) ;
#14016 = EDGE_CURVE ( 'NONE', #33479, #38417, #8780, .T. ) ;
#14017 = CARTESIAN_POINT ( 'NONE',  ( 784.0799538623451781, -299.8055962898685038, -364.6971507214555572 ) ) ;
#14018 = FACE_OUTER_BOUND ( 'NONE', #40567, .T. ) ;
#14019 = CARTESIAN_POINT ( 'NONE',  ( 781.2370466360911223, -164.7363362996983938, -304.9990715423533629 ) ) ;
#14020 = CARTESIAN_POINT ( 'NONE',  ( 989.9999999999992042, -185.0721577059061929, 75.19946970736501157 ) ) ;
#14021 = DIRECTION ( 'NONE',  ( 0.000000000000000000, 0.000000000000000000, -1.000000000000000000 ) ) ;
#14022 = CARTESIAN_POINT ( 'NONE',  ( 799.2566176426618085, -384.0090635724249637, 324.0069404352559559 ) ) ;
#14023 = EDGE_CURVE ( 'NONE', #18427, #40312, #33680, .T. ) ;
#14024 = CARTESIAN_POINT ( 'NONE',  ( 752.7379699480933368, -324.0090635724251911, 361.9858362298580232 ) ) ;
#14025 = CARTESIAN_POINT ( 'NONE',  ( 792.2312462859673587, -203.9073299311471885, -307.2067596250082602 ) ) ;
#14026 = DIRECTION ( 'NONE',  ( 1.000000000000000000, 0.000000000000000000, 0.000000000000000000 ) ) ;
#14027 = CARTESIAN_POINT ( 'NONE',  ( 774.6858677611749044, 14.27448825067031812, -315.5713283507209894 ) ) ;
#14028 = CARTESIAN_POINT ( 'NONE',  ( 814.8207195650702488, -146.1908817542438896, 336.2433038121456548 ) ) ;
#14029 = CARTESIAN_POINT ( 'NONE',  ( 786.2056067578752163, -107.8055962898691433, -374.4686193811670023 ) ) ;
#14030 = CARTESIAN_POINT ( 'NONE',  ( 813.1304606946830518, -353.9073299311467053, -352.3570229623690580 ) ) ;
#14031 = CARTESIAN_POINT ( 'NONE',  ( -66.63011601220125613, -355.4967352946684969, -16.45562775363632113 ) ) ;
#14032 = CARTESIAN_POINT ( 'NONE',  ( 794.9999999999993179, 205.0000000000000568, -255.0000000000000000 ) ) ;
#14033 =( REPRESENTATION_RELATIONSHIP ('NONE','NONE', #39835, #36841 ) REPRESENTATION_RELATIONSHIP_WITH_TRANSFORMATION ( #1090 )SHAPE_REPRESENTATION_RELATIONSHIP( ) );
#14034 = CARTESIAN_POINT ( 'NONE',  ( 771.2633955100217236, -191.9073299311471885, 363.4237431249939618 ) ) ;
#14035 = VERTEX_POINT ( 'NONE', #18343 ) ;
#14036 = CARTESIAN_POINT ( 'NONE',  ( 747.6481478633932056, -445.0999726633338582, 353.4146539503763620 ) ) ;
#14037 = CARTESIAN_POINT ( 'NONE',  ( 801.9858362298568863, -363.0783235625955854, -312.7379699480935642 ) ) ;
#14038 = CARTESIAN_POINT ( 'NONE',  ( 751.9810565676468741, -146.0891481129655176, -360.9747183278973921 ) ) ;
#14039 = CARTESIAN_POINT ( 'NONE',  ( 814.9108240113580450, -424.2709662947829088, -337.5031285880265273 ) ) ;
#14040 = DIRECTION ( 'NONE',  ( -0.000000000000000000, 1.000000000000000000, -0.000000000000000000 ) ) ;
#14041 = CARTESIAN_POINT ( 'NONE',  ( 778.7502325331095108, -0.3510508353240099355, 304.6391490659818828 ) ) ;
#14042 = ORIENTED_EDGE ( 'NONE', *, *, #6577, .F. ) ;
#14043 = CARTESIAN_POINT ( 'NONE',  ( 765.0180583372156207, -264.9982390220561115, 360.0135310231089534 ) ) ;
#14044 = CARTESIAN_POINT ( 'NONE',  ( 771.2368401574024119, -181.4419599262325278, -374.2805881961240857 ) ) ;
#14045 = DIRECTION ( 'NONE',  ( -1.000000000000000000, -0.000000000000000000, -0.000000000000000000 ) ) ;
#14046 = CARTESIAN_POINT ( 'NONE',  ( 776.2433038121456548, -300.8965053807775689, 374.8207195650711014 ) ) ;
#14047 = CARTESIAN_POINT ( 'NONE',  ( 762.3223304703356007, -127.5436935675110561, 322.3223304703362828 ) ) ;
#14048 = ORIENTED_EDGE ( 'NONE', *, *, #37141, .T. ) ;
#14049 = CARTESIAN_POINT ( 'NONE',  ( 781.8018195045266339, -310.2709662947832499, 365.1927285166406705 ) ) ;
#14050 = CARTESIAN_POINT ( 'NONE',  ( 805.0032342141412300, -13.54369356751140785, -314.9967657858571783 ) ) ;
#14051 = CARTESIAN_POINT ( 'NONE',  ( 441.1634899080286232, 259.9999999999999432, -202.7499999999971010 ) ) ;
#14052 = VERTEX_POINT ( 'NONE', #32424 ) ;
#14053 = CARTESIAN_POINT ( 'NONE',  ( 744.6391490659812007, -422.7363362996975980, -338.7502325331110455 ) ) ;
#14054 = ORIENTED_EDGE ( 'NONE', *, *, #2947, .T. ) ;
#14055 = CARTESIAN_POINT ( 'NONE',  ( 762.1405469898971887, -25.54369356751136877, 357.8594530101015607 ) ) ;
#14056 = CARTESIAN_POINT ( 'NONE',  ( 800.0135310231082713, -254.0891481129652334, -325.0180583372163028 ) ) ;
#14058 = CARTESIAN_POINT ( 'NONE',  ( 786.2056067578752163, -251.8055962898686744, 374.4686193811670023 ) ) ;
#14057 = CARTESIAN_POINT ( 'NONE',  ( 812.7932403749906598, -351.1800572038740142, 327.7687537140311633 ) ) ;
#14059 = CARTESIAN_POINT ( 'NONE',  ( 749.8865473780648472, -68.53286901714197654, 322.1177392798429082 ) ) ;
#14060 = CARTESIAN_POINT ( 'NONE',  ( 796.1575198192839480, -246.0090635724253900, -359.4546378042384163 ) ) ;
#14061 = CARTESIAN_POINT ( 'NONE',  ( 795.1360043628807261, -260.0891481129650060, -360.2193346964456282 ) ) ;
#14062 = CARTESIAN_POINT ( 'NONE',  ( 804.9363028652555840, -448.2709662947827951, -338.2165204200192079 ) ) ;
#14063 = CARTESIAN_POINT ( 'NONE',  ( 805.1927285166397041, -256.8164208402379245, 341.8018195045277707 ) ) ;
#14064 = ORIENTED_EDGE ( 'NONE', *, *, #21274, .F. ) ;
#14065 = CARTESIAN_POINT ( 'NONE',  ( 808.3070685750230950, -378.9982390220555999, 361.1904061080339261 ) ) ;
#14067 = DIRECTION ( 'NONE',  ( 0.000000000000000000, -1.000000000000000000, 0.000000000000000000 ) ) ;
#14066 = DIRECTION ( 'NONE',  ( -1.000000000000000000, 1.892425610156518354E-16, -0.000000000000000000 ) ) ;
#14068 = CARTESIAN_POINT ( 'NONE',  ( 768.9521613784389729, -33.82724539060788516, -373.2346286133773106 ) ) ;
#14069 = DIRECTION ( 'NONE',  ( -0.000000000000000000, -0.000000000000000000, -1.000000000000000000 ) ) ;
#14070 = DIRECTION ( 'NONE',  ( 1.000000000000000000, 0.000000000000000000, 0.000000000000000000 ) ) ;
#14071 = CARTESIAN_POINT ( 'NONE',  ( 779.4763451958990572, -248.7363362996981380, 365.0264073115438919 ) ) ;
#14072 = CARTESIAN_POINT ( 'NONE',  ( 762.3223304703356007, -127.5436935675110561, 322.3223304703362828 ) ) ;
#14073 = VERTEX_POINT ( 'NONE', #43646 ) ;
#14074 = CARTESIAN_POINT ( 'NONE',  ( 790.9844846989617508, -22.37269993606246743, -317.2208543904092721 ) ) ;
#14075 = CARTESIAN_POINT ( 'NONE',  ( 777.5031285880264704, -94.81642084023843609, -374.9108240113588408 ) ) ;
#14076 = CARTESIAN_POINT ( 'NONE',  ( 754.8983024940795303, -306.8965053807775689, 336.9254006560228163 ) ) ;
#14077 = DIRECTION ( 'NONE',  ( 0.000000000000000000, 0.000000000000000000, 1.000000000000000000 ) ) ;
#14078 = CARTESIAN_POINT ( 'NONE',  ( 813.5763878283155464, -27.82724539060790292, 351.1614460488615350 ) ) ;
#14079 = CARTESIAN_POINT ( 'NONE',  ( 745.4481719005789273, -243.7255117493287742, -347.5162901302853129 ) ) ;
#14080 = CARTESIAN_POINT ( 'NONE',  ( 787.5162901302840055, -179.3618753856927128, 305.4481719005792684 ) ) ;
#14081 = CARTESIAN_POINT ( 'NONE',  ( 794.9819416627830151, -84.99823902205663728, 319.9864689768909898 ) ) ;
#14082 = CARTESIAN_POINT ( 'NONE',  ( 441.1634899080286232, 258.0939999999999372, -199.9999999999972431 ) ) ;
#14083 = CARTESIAN_POINT ( 'NONE',  ( 803.8556311672234642, -273.6237781080504305, -365.6418435158340117 ) ) ;
#14084 = CARTESIAN_POINT ( 'NONE',  ( 790.9844846989617508, 1.627300063937458408, 317.2208543904092721 ) ) ;
#14085 = CARTESIAN_POINT ( 'NONE',  ( 792.3570229623688874, -333.1800572038740142, -373.1304606946836202 ) ) ;
#14086 = CARTESIAN_POINT ( 'NONE',  ( -28.63011601220122415, -512.9681489794448908, -339.9999999999999432 ) ) ;
#14087 = CARTESIAN_POINT ( 'NONE',  ( 784.0799538623451781, -347.8055962898683333, 364.6971507214555572 ) ) ;
#14088 = CARTESIAN_POINT ( 'NONE',  ( 787.4397851343537695, -45.72551174932949181, 374.2001403089903988 ) ) ;
#14089 = CARTESIAN_POINT ( 'NONE',  ( 762.3223304703356007, -391.5436935675101608, -322.3223304703362828 ) ) ;
#14090 = CARTESIAN_POINT ( 'NONE',  ( 761.2382568024794409, -39.62377810805116951, 356.9571628226838129 ) ) ;
#14091 = CARTESIAN_POINT ( 'NONE',  ( 778.1981804954714335, -202.2709662947834772, -314.8072714833589885 ) ) ;
#14092 = CARTESIAN_POINT ( 'NONE',  ( 768.8385539511368734, -47.26014174441477422, -306.4236121716840557 ) ) ;
#14093 = CARTESIAN_POINT ( 'NONE',  ( 776.9566956441375396, -180.8965053807779952, -364.8461984189686405 ) ) ;
#14094 = CARTESIAN_POINT ( 'NONE',  ( 768.8385539511368734, -191.2601417444143976, 306.4236121716840557 ) ) ;
#14095 = CARTESIAN_POINT ( 'NONE',  ( 803.4237431249931660, -15.18005720387504631, 331.2633955100225194 ) ) ;
#14096 = EDGE_LOOP ( 'NONE', ( #41830, #18102, #4002, #35850 ) ) ;
#14097 = CARTESIAN_POINT ( 'NONE',  ( 772.3691319403857278, -191.2601417444143976, -315.8894580844506663 ) ) ;
#14098 = CARTESIAN_POINT ( 'NONE',  ( 762.3223304703356007, -199.5436935675108430, 322.3223304703362828 ) ) ;
#14099 = PRODUCT_DEFINITION_SHAPE ( 'NONE', 'NONE',  #23335 ) ;
#14100 = CARTESIAN_POINT ( 'NONE',  ( 773.7943932421234194, -47.80559628986931386, -305.5313806188329409 ) ) ;
#14101 = CARTESIAN_POINT ( 'NONE',  ( 767.8955696845334842, -312.4527844766013800, 362.1676090361161755 ) ) ;
#14102 = CARTESIAN_POINT ( 'NONE',  ( 759.0860845406687076, 19.76315572498245743, 318.4906424660488256 ) ) ;
#14103 = VERTEX_POINT ( 'NONE', #17870 ) ;
#14104 = CARTESIAN_POINT ( 'NONE',  ( 776.9566956441375396, -60.89650538077837894, 364.8461984189686405 ) ) ;
#14105 = CARTESIAN_POINT ( 'NONE',  ( 804.1009440267234822, -311.4636090269706870, -314.0944755984392600 ) ) ;
#14106 = CARTESIAN_POINT ( 'NONE',  ( 814.2001403089898304, -257.3618753856924286, 347.4397851343538264 ) ) ;
#14107 = CARTESIAN_POINT ( 'NONE',  ( 807.5423716828161105, 14.92167643740321381, 362.2119215644372048 ) ) ;
#14108 = CARTESIAN_POINT ( 'NONE',  ( 755.5913626894240451, -157.6454272087893287, -346.6156483768012890 ) ) ;
#14109 = CARTESIAN_POINT ( 'NONE',  ( 764.8639956371174549, -152.0891481129655460, -319.7806653035542013 ) ) ;
#14110 = AXIS2_PLACEMENT_3D ( 'NONE', #29184, #4691, #40929 ) ;
#14111 = CARTESIAN_POINT ( 'NONE',  ( 781.7834795799800531, -346.8164208402376971, -315.0636971347436202 ) ) ;
#14112 = ORIENTED_EDGE ( 'NONE', *, *, #42969, .T. ) ;
#14113 = CARTESIAN_POINT ( 'NONE',  ( 754.9967657858570647, -289.5436935675103882, 365.0032342141425374 ) ) ;
#14114 = CARTESIAN_POINT ( 'NONE',  ( -775.4999999999993179, -544.8427095258973623, -369.9999999999999432 ) ) ;
#14115 = CARTESIAN_POINT ( 'NONE',  ( 804.1601925771018387, -343.4419599262320162, 346.5483106153029098 ) ) ;
#14116 = PLANE ( 'NONE',  #32982 ) ;
#14117 = CARTESIAN_POINT ( 'NONE',  ( 787.5531968255692163, -141.8272453906075157, 316.1348686366205811 ) ) ;
#14118 = CARTESIAN_POINT ( 'NONE',  ( 759.9864689768902508, -2.089148112965993231, 354.9819416627836404 ) ) ;
#14119 = ORIENTED_EDGE ( 'NONE', *, *, #15376, .T. ) ;
#14120 = CARTESIAN_POINT ( 'NONE',  ( 814.4686193811664907, -387.2817908451522726, -346.2056067578752732 ) ) ;
#14121 = EDGE_CURVE ( 'NONE', #1648, #11148, #12015, .T. ) ;
#14122 = DIRECTION ( 'NONE',  ( 0.000000000000000000, 0.3826834323650838421, 0.9238795325112891810 ) ) ;
#14123 = CARTESIAN_POINT ( 'NONE',  ( 809.0717654672305343, -244.9181544815162681, 360.1688906516309885 ) ) ;
#14124 = CARTESIAN_POINT ( 'NONE',  ( 779.4709603349208464, -192.3510508353233774, 314.7162404726379918 ) ) ;
#14125 = CARTESIAN_POINT ( 'NONE',  ( 803.6646147819161570, -377.9073299311466485, -348.8264449731210561 ) ) ;
#14126 = FILL_AREA_STYLE_COLOUR ( '', #17835 ) ;
#14127 = CARTESIAN_POINT ( 'NONE',  ( 755.1538015810308480, -230.1908817542436338, -343.0433043558613804 ) ) ;
#14128 = CARTESIAN_POINT ( 'NONE',  ( 767.7687537140311633, 0.09267006885218045942, 372.7932403749916830 ) ) ;
#14129 = CARTESIAN_POINT ( 'NONE',  ( 801.1904061080336987, -68.08914811296575920, 368.3070685750235498 ) ) ;
#14130 = DIRECTION ( 'NONE',  ( -1.000000000000000000, 0.000000000000000000, 0.000000000000000000 ) ) ;
#14131 = CARTESIAN_POINT ( 'NONE',  ( 759.0252816721024374, -408.9982390220556567, -368.0189434323527280 ) ) ;
#14132 = CARTESIAN_POINT ( 'NONE',  ( 879.9999999999990905, 50.81038600091414281, 210.0000000000000000 ) ) ;
#14133 = CARTESIAN_POINT ( 'NONE',  ( 773.7305795820266212, -345.2817908451523863, 374.8230680027170365 ) ) ;
#14134 = DIRECTION ( 'NONE',  ( -5.551115123125783688E-16, 1.000000000000000000, 0.000000000000000000 ) ) ;
#14135 = CARTESIAN_POINT ( 'NONE',  ( 796.7737145352015204, -332.6346026584195101, 370.7187646348536987 ) ) ;
#14136 = CARTESIAN_POINT ( 'NONE',  ( 814.5518280994195948, -39.72551174932951312, -332.4837098697145734 ) ) ;
#14137 = CARTESIAN_POINT ( 'NONE',  ( 755.5713283507202505, -269.3618753856924286, -334.6858677611754729 ) ) ;
#14138 = DIRECTION ( 'NONE',  ( 0.000000000000000000, 0.000000000000000000, 1.000000000000000000 ) ) ;
#14139 = CARTESIAN_POINT ( 'NONE',  ( 759.7806653035534055, -414.9982390220555430, 324.8639956371180801 ) ) ;
#14140 = VECTOR ( 'NONE', #34457, 1000.000000000000000 ) ;
#14141 = CARTESIAN_POINT ( 'NONE',  ( 769.9779781133707957, -139.0999726633348530, 316.7813123517150871 ) ) ;
#14142 = CARTESIAN_POINT ( 'NONE',  ( 771.3260364891663130, -19.64542720878974791, -306.0683387631859773 ) ) ;
#14143 = CARTESIAN_POINT ( 'NONE',  ( 805.0264073115434940, -102.3510508353236901, -339.4763451958999099 ) ) ;
#14144 = CARTESIAN_POINT ( 'NONE',  ( 814.8230680027162407, -101.8055962898691718, 333.7305795820267917 ) ) ;
#14145 = CARTESIAN_POINT ( 'NONE',  ( 764.8639956371174549, -416.0891481129646650, 319.7806653035542581 ) ) ;
#14146 = LINE ( 'NONE', #11772, #7060 ) ;
#14147 = CARTESIAN_POINT ( 'NONE',  ( 789.5670355615794733, -453.0432664090020012, 363.0970091259334822 ) ) ;
#14149 = ORIENTED_EDGE ( 'NONE', *, *, #41924, .F. ) ;
#14148 = CARTESIAN_POINT ( 'NONE',  ( 770.0799878456142551, -109.9874144716873019, -362.9823548866085616 ) ) ;
#14150 = CARTESIAN_POINT ( 'NONE',  ( 771.1735550268778070, -81.18005720387481006, -316.3353852180827630 ) ) ;
#14151 = CARTESIAN_POINT ( 'NONE',  ( 804.1601925771018387, -391.4419599262317888, -346.5483106153029098 ) ) ;
#14153 = CARTESIAN_POINT ( 'NONE',  ( 804.6798772138710092, -231.7255117493288594, 334.6312213355106451 ) ) ;
#14152 = CARTESIAN_POINT ( 'NONE',  ( 801.9419747391806368, -234.4527844766016358, 351.9812246680014027 ) ) ;
#14154 = CARTESIAN_POINT ( 'NONE',  ( 744.8212110874229666, -402.8965053807773415, -336.2046728542121627 ) ) ;
#14155 = CARTESIAN_POINT ( 'NONE',  ( 800.1688906516307043, -442.1692326535044231, 369.0717654672308186 ) ) ;
#14156 = DIRECTION ( 'NONE',  ( -1.000000000000000000, -0.000000000000000000, 0.000000000000000000 ) ) ;
#14157 = ORIENTED_EDGE ( 'NONE', *, *, #27840, .T. ) ;
#14158 = CARTESIAN_POINT ( 'NONE',  ( 756.3353852180819104, -413.9073299311465348, 331.1735550268788302 ) ) ;
#14159 = EDGE_LOOP ( 'NONE', ( #23110, #31541, #26844, #24065 ) ) ;
#14160 = CARTESIAN_POINT ( 'NONE',  ( 814.2001403089898304, -257.3618753856924286, -347.4397851343538264 ) ) ;
#14161 = CARTESIAN_POINT ( 'NONE',  ( 812.7932403749906598, -159.1800572038746111, 327.7687537140311633 ) ) ;
#14162 = ORIENTED_EDGE ( 'NONE', *, *, #42537, .F. ) ;
#14163 = CARTESIAN_POINT ( 'NONE',  ( 800.2193346964446619, -234.9982390220561683, -355.1360043628816925 ) ) ;
#14164 = VERTEX_POINT ( 'NONE', #40195 ) ;
#14165 = CARTESIAN_POINT ( 'NONE',  ( 755.3201227861273992, -363.7255117493284047, -345.3687786644892981 ) ) ;
#14166 = CARTESIAN_POINT ( 'NONE',  ( 774.6312213355099630, -23.36187538569318889, -364.6798772138717482 ) ) ;
#14167 = CARTESIAN_POINT ( 'NONE',  ( 755.8398074228967971, -235.4419599262323857, 333.4516893846970333 ) ) ;
#14168 = DIRECTION ( 'NONE',  ( -0.000000000000000000, -0.000000000000000000, 1.000000000000000000 ) ) ;
#14169 = EDGE_CURVE ( 'NONE', #13298, #33885, #13782, .T. ) ;
#14170 = CARTESIAN_POINT ( 'NONE',  ( 799.9999999999993179, -512.9681489794448908, -339.9999999999999432 ) ) ;
#14171 = EDGE_LOOP ( 'NONE', ( #42328, #23959, #32172, #29110 ) ) ;
#14172 = CARTESIAN_POINT ( 'NONE',  ( 778.1981804954714335, -10.27096629478414691, -314.8072714833589885 ) ) ;
#14173 = CARTESIAN_POINT ( 'NONE',  ( -78.83651009197140525, 256.5000000000000568, -199.9999999999936051 ) ) ;
#14174 = DIRECTION ( 'NONE',  ( 0.000000000000000000, 0.000000000000000000, 1.000000000000000000 ) ) ;
#14175 = VERTEX_POINT ( 'NONE', #30455 ) ;
#14176 = CARTESIAN_POINT ( 'NONE',  ( 748.6759233522253680, -256.3726999360617924, -324.3348316497537098 ) ) ;
#14177 = CARTESIAN_POINT ( 'NONE',  ( 812.3518521366052028, -121.0999726633348956, 326.5853460496235243 ) ) ;
#14179 = CARTESIAN_POINT ( 'NONE',  ( 778.2165204200184689, -214.8164208402380666, -364.9363028652563230 ) ) ;
#14178 = DIRECTION ( 'NONE',  ( -1.880165489482579047E-16, -1.000000000000000000, -0.000000000000000000 ) ) ;
#14180 = CARTESIAN_POINT ( 'NONE',  ( 760.5453621957607311, -405.0783235625954148, -323.8424801807151425 ) ) ;
#14181 = CARTESIAN_POINT ( 'NONE',  ( 759.9999999999992042, -512.9681489794448908, -339.9999999999999432 ) ) ;
#14182 = CARTESIAN_POINT ( 'NONE',  ( 780.5236548040995785, -116.7363362996985217, -314.9735926884559944 ) ) ;
#14183 = CARTESIAN_POINT ( 'NONE',  ( 807.2620300519052989, -384.0090635724249637, 318.0141637701419768 ) ) ;
#14184 = DIRECTION ( 'NONE',  ( 0.000000000000000000, 0.000000000000000000, -1.000000000000000000 ) ) ;
#14185 = CARTESIAN_POINT ( 'NONE',  ( 764.3348316497523456, 25.28531280103955226, -308.6759233522265617 ) ) ;
#14186 = CARTESIAN_POINT ( 'NONE',  ( 744.7301800767020268, -316.8164208402377540, -337.4774526936615189 ) ) ;
#14187 = CARTESIAN_POINT ( 'NONE',  ( 759.9999999999992042, 205.0000000000000568, 350.0000000000000000 ) ) ;
#14188 = CARTESIAN_POINT ( 'NONE',  ( 756.3353852180819104, -5.907329931147798696, 331.1735550268788302 ) ) ;
#14189 = CARTESIAN_POINT ( 'NONE',  ( 765.0180583372156207, -72.99823902205667991, -360.0135310231089534 ) ) ;
#14190 = CARTESIAN_POINT ( 'NONE',  ( 809.0717654672305343, -244.9181544815162681, 360.1688906516309885 ) ) ;
#14191 = CARTESIAN_POINT ( 'NONE',  ( 798.0661480581538854, -194.5328690171415644, -309.5768839229118043 ) ) ;
#14192 = CARTESIAN_POINT ( 'NONE',  ( 751.6929314249748586, -222.9982390220561399, 318.8095938919659034 ) ) ;
#14193 = CARTESIAN_POINT ( 'NONE',  ( 795.1271208383656131, -452.8379544210779954, -371.6178728169206238 ) ) ;
#14194 = CARTESIAN_POINT ( 'NONE',  ( -858.8365100919713768, 260.0000000000002274, -191.9749999999881993 ) ) ;
#14195 = EDGE_CURVE ( 'NONE', #20161, #18157, #43224, .T. ) ;
#14196 = CARTESIAN_POINT ( 'NONE',  ( 774.6858677611749044, -297.7255117493286889, 315.5713283507209894 ) ) ;
#14197 = AXIS2_PLACEMENT_3D ( 'NONE', #10093, #27189, #23925 ) ;
#14198 = CARTESIAN_POINT ( 'NONE',  ( 804.1105419155481968, -99.82724539060768620, 347.6308680596136469 ) ) ;
#14199 = CARTESIAN_POINT ( 'NONE',  ( 800.2193346964447755, -450.9982390220554294, -355.1360043628815788 ) ) ;
#14200 = CARTESIAN_POINT ( 'NONE',  ( -598.8365100919716042, 260.0000000000001705, -199.9999999999899671 ) ) ;
#14201 = DIRECTION ( 'NONE',  ( -0.000000000000000000, -0.000000000000000000, -1.000000000000000000 ) ) ;
#14203 = CARTESIAN_POINT ( 'NONE',  ( 803.6646147819161570, -353.9073299311467053, 348.8264449731210561 ) ) ;
#14202 = CARTESIAN_POINT ( 'NONE',  ( 766.7756240680305382, -110.5328690171418629, 361.5560724626415663 ) ) ;
#14204 = ORIENTED_EDGE ( 'NONE', *, *, #18199, .T. ) ;
#14205 = CARTESIAN_POINT ( 'NONE',  ( 765.8855110935204493, -310.1692326535048778, -319.0159684113471599 ) ) ;
#14206 = CARTESIAN_POINT ( 'NONE',  ( 792.1044303154645831, -108.4527844766019911, 317.8323909638837677 ) ) ;
#14207 = CARTESIAN_POINT ( 'NONE',  ( 793.4146539503750546, -289.9874144716866908, -307.6481478633938877 ) ) ;
#14208 = DIRECTION ( 'NONE',  ( 1.000000000000000000, 0.000000000000000000, 0.000000000000000000 ) ) ;
#14209 = CARTESIAN_POINT ( 'NONE',  ( 778.7502325331095108, -408.3510508353227806, 304.6391490659818828 ) ) ;
#14210 = VERTEX_POINT ( 'NONE', #23061 ) ;
#14211 = CARTESIAN_POINT ( 'NONE',  ( 803.6646147819161570, -329.9073299311467053, 348.8264449731210561 ) ) ;
#14212 = CARTESIAN_POINT ( 'NONE',  ( 805.1016975059191054, -54.89650538077837183, -343.0745993439771837 ) ) ;
#14213 = CARTESIAN_POINT ( 'NONE',  ( 800.2193346964447755, -162.9982390220563673, -355.1360043628815788 ) ) ;
#14214 = CARTESIAN_POINT ( 'NONE',  ( 781.8018195045266339, -214.2709662947834488, -365.1927285166406705 ) ) ;
#14215 = CARTESIAN_POINT ( 'NONE',  ( 771.1735550268778070, -393.1800572038737300, 316.3353852180827630 ) ) ;
#14216 = EDGE_CURVE ( 'NONE', #26065, #45022, #44800, .T. ) ;
#14217 = CARTESIAN_POINT ( 'NONE',  ( 758.8095938919642549, -152.0891481129655460, -311.6929314249763365 ) ) ;
#14218 = CARTESIAN_POINT ( 'NONE',  ( 759.7806653035535192, -126.9982390220565094, -324.8639956371181370 ) ) ;
#14219 = ORIENTED_EDGE ( 'NONE', *, *, #6037, .F. ) ;
#14220 = CARTESIAN_POINT ( 'NONE',  ( 796.1575198192839480, -390.0090635724249069, -359.4546378042384163 ) ) ;
#14222 = CARTESIAN_POINT ( 'NONE',  ( 784.1219089521767955, -429.2817908451521021, 315.0488828828318333 ) ) ;
#14221 = CARTESIAN_POINT ( 'NONE',  ( 791.9812246680005501, -116.6346026584201780, 361.9419747391813189 ) ) ;
#14223 = CARTESIAN_POINT ( 'NONE',  ( 755.0488828828309806, -113.8055962898691149, 344.1219089521771934 ) ) ;
#14226 = CARTESIAN_POINT ( 'NONE',  ( 758.0141637701419768, -399.0783235625955285, 367.2620300519063790 ) ) ;
#14225 = PLANE ( 'NONE',  #15167 ) ;
#14224 = PLANE ( 'NONE',  #43937 ) ;
#14227 = EDGE_CURVE ( 'NONE', #37975, #44323, #41328, .T. ) ;
#14228 = ORIENTED_EDGE ( 'NONE', *, *, #20764, .F. ) ;
#14229 = CARTESIAN_POINT ( 'NONE',  ( 780.5236548040995785, -380.7363362996977116, -314.9735926884559944 ) ) ;
#14230 = CARTESIAN_POINT ( 'NONE',  ( 764.8639956371174549, -344.0891481129647786, -319.7806653035542013 ) ) ;
#14231 = AXIS2_PLACEMENT_3D ( 'NONE', #25546, #11696, #39659 ) ;
#14232 = CARTESIAN_POINT ( 'NONE',  ( 791.0478386215596629, -165.8272453906074873, -306.7653713866226326 ) ) ;
#14233 = CARTESIAN_POINT ( 'NONE',  ( 764.1737431748507561, -34.37269993606243901, 371.6461892240376415 ) ) ;
#14235 = CARTESIAN_POINT ( 'NONE',  ( 571.1634899080285095, 239.9999999999999716, -199.9999999999981526 ) ) ;
#14234 = CARTESIAN_POINT ( 'NONE',  ( 767.9999999999992042, 205.0000000000000568, -339.9999999999999432 ) ) ;
#14236 = CARTESIAN_POINT ( 'NONE',  ( 793.2243759319678702, -290.5328690171412518, -318.4439275373583200 ) ) ;
#14237 = CARTESIAN_POINT ( 'NONE',  ( 803.4237431249931660, -447.1800572038736732, -331.2633955100225194 ) ) ;
#14238 = CARTESIAN_POINT ( 'NONE',  ( 793.5525998758768083, -151.0999726633347677, -372.6845335610516941 ) ) ;
#14239 = CARTESIAN_POINT ( 'NONE',  ( -773.4999999999993179, -513.1383975375929367, -369.9999999999999432 ) ) ;
#14240 = DIRECTION ( 'NONE',  ( -0.000000000000000000, 1.000000000000000000, -0.000000000000000000 ) ) ;
#14241 = CARTESIAN_POINT ( 'NONE',  ( 793.0897708529556667, -366.5545181178795815, 361.3366627262616362 ) ) ;
#14242 = CARTESIAN_POINT ( 'NONE',  ( 764.1737431748507561, -322.3726999360615082, 371.6461892240376415 ) ) ;
#14243 = CARTESIAN_POINT ( 'NONE',  ( 777.5031285880264704, -214.8164208402380666, -374.9108240113588408 ) ) ;
#14244 = ADVANCED_FACE ( 'NONE', ( #16378 ), #37854, .F. ) ;
#14245 = CARTESIAN_POINT ( 'NONE',  ( 200.7583438952258348, 240.0000000000006253, -244.9999999999999716 ) ) ;
#14246 = LINE ( 'NONE', #44571, #39514 ) ;
#14247 = CARTESIAN_POINT ( 'NONE',  ( 776.2046728542105711, -140.1908817542438896, 304.8212110874238761 ) ) ;
#14248 = ADVANCED_FACE ( 'NONE', ( #27452 ), #20531, .F. ) ;
#14249 = CARTESIAN_POINT ( 'NONE',  ( 745.1769319972822814, -113.8055962898691149, -346.2694204179732083 ) ) ;
#14250 = CARTESIAN_POINT ( 'NONE',  ( 744.7301800767019131, -124.8164208402383508, 337.4774526936615757 ) ) ;
#14251 = CARTESIAN_POINT ( 'NONE',  ( 814.2001403089898304, -329.3618753856922581, -347.4397851343538264 ) ) ;
#14252 = DIRECTION ( 'NONE',  ( 1.892425610156518354E-16, 1.000000000000000000, -0.000000000000000000 ) ) ;
#14253 = CARTESIAN_POINT ( 'NONE',  ( 786.4999999999993179, -494.6608068873671300, -357.6536686473015720 ) ) ;
#14254 = EDGE_CURVE ( 'NONE', #41324, #38502, #44099, .T. ) ;
#14255 = CARTESIAN_POINT ( 'NONE',  ( 778.1981804954714335, -178.2709662947835625, 314.8072714833589885 ) ) ;
#14256 = CARTESIAN_POINT ( 'NONE',  ( 780.5236548040995785, 3.263663700301089765, 314.9735926884559944 ) ) ;
#14257 = CARTESIAN_POINT ( 'NONE',  ( 744.9990715423526808, -426.3510508353226669, -341.2370466360926002 ) ) ;
#14258 = CARTESIAN_POINT ( 'NONE',  ( 814.2001403089898304, -425.3618753856919170, -347.4397851343538264 ) ) ;
#14259 = CARTESIAN_POINT ( 'NONE',  ( -598.8365100919716042, 260.0000000000001705, -191.9749999999900183 ) ) ;
#14260 = CARTESIAN_POINT ( 'NONE',  ( 808.7758568127978833, 19.83076734649410966, 320.0363995740631822 ) ) ;
#14261 = ORIENTED_EDGE ( 'NONE', *, *, #12591, .T. ) ;
#14262 = VECTOR ( 'NONE', #28313, 1000.000000000000227 ) ;
#14263 = CARTESIAN_POINT ( 'NONE',  ( 747.3154664389472828, -187.9874144716870603, -326.4474001241230781 ) ) ;
#14264 = CARTESIAN_POINT ( 'NONE',  ( 776.2433038121456548, -324.8965053807775121, 374.8207195650711014 ) ) ;
#14265 = CARTESIAN_POINT ( 'NONE',  ( 778.2165204200184689, -118.8164208402383508, 364.9363028652563230 ) ) ;
#14266 =( GEOMETRIC_REPRESENTATION_CONTEXT ( 3 ) GLOBAL_UNCERTAINTY_ASSIGNED_CONTEXT ( ( #33338 ) ) GLOBAL_UNIT_ASSIGNED_CONTEXT ( ( #12966, #8602, #22669 ) ) REPRESENTATION_CONTEXT ( 'NONE', 'WORKASPACE' ) );
#14267 = ORIENTED_EDGE ( 'NONE', *, *, #14801, .T. ) ;
#14268 = EDGE_CURVE ( 'NONE', #29782, #30209, #23374, .T. ) ;
#14269 = CARTESIAN_POINT ( 'NONE',  ( 759.9864689768902508, -290.0891481129650629, 354.9819416627836404 ) ) ;
#14270 = ADVANCED_FACE ( 'NONE', ( #33710, #2059, #16152 ), #40866, .F. ) ;
#14271 = CARTESIAN_POINT ( 'NONE',  ( 792.2312462859673587, -59.90732993114762905, -307.2067596250082602 ) ) ;
#14272 = CARTESIAN_POINT ( 'NONE',  ( 815.2698199232962679, -88.81642084023843609, 342.5225473063383674 ) ) ;
#14273 = ORIENTED_EDGE ( 'NONE', *, *, #2706, .F. ) ;
#14274 = CARTESIAN_POINT ( 'NONE',  ( 762.1177392798416577, -450.5545181178793541, -309.8865473780659272 ) ) ;
#14275 = ORIENTED_EDGE ( 'NONE', *, *, #15051, .T. ) ;
#14276 = CARTESIAN_POINT ( 'NONE',  ( 792.1044303154645831, -12.45278447660232146, 317.8323909638837677 ) ) ;
#14277 = CARTESIAN_POINT ( 'NONE',  ( 800.0135310231082713, -278.0891481129651197, -325.0180583372163028 ) ) ;
#14278 = EDGE_CURVE ( 'NONE', #1429, #16430, #20973, .T. ) ;
#14280 = CARTESIAN_POINT ( 'NONE',  ( 812.6845335610512393, -295.9874144716866908, 353.5525998758768651 ) ) ;
#14279 = CARTESIAN_POINT ( 'NONE',  ( 813.1304606946831655, -377.9073299311465917, 352.3570229623691716 ) ) ;
#14281 = EDGE_CURVE ( 'NONE', #11197, #17401, #18953, .T. ) ;
#14282 = CARTESIAN_POINT ( 'NONE',  ( 786.2056067578752163, -83.80559628986920018, 374.4686193811670023 ) ) ;
#14283 = CARTESIAN_POINT ( 'NONE',  ( 804.8461984189677878, -266.1908817542435486, -336.9566956441385628 ) ) ;
#14284 = CARTESIAN_POINT ( 'NONE',  ( 756.5762568750052424, -243.1800572038743269, -348.7366044899774238 ) ) ;
#14285 = CARTESIAN_POINT ( 'NONE',  ( 792.1044303154646968, -444.4527844766009821, -317.8323909638837677 ) ) ;
#14286 = CARTESIAN_POINT ( 'NONE',  ( 756.3353852180819104, -101.9073299311474727, -331.1735550268788302 ) ) ;
#14287 = FACE_OUTER_BOUND ( 'NONE', #29742, .T. ) ;
#14288 = CARTESIAN_POINT ( 'NONE',  ( 811.0346526505616112, -398.6346026584193396, 323.0537975583477532 ) ) ;
#14290 = DIRECTION ( 'NONE',  ( -0.000000000000000000, -0.000000000000000000, 1.000000000000000000 ) ) ;
#14289 = CARTESIAN_POINT ( 'NONE',  ( 879.9999999999990905, -419.8175818341089780, -210.0000000000000000 ) ) ;
#14291 = CARTESIAN_POINT ( 'NONE',  ( 746.4236121716829757, -39.82724539060786384, -328.8385539511384650 ) ) ;
#14292 = DIRECTION ( 'NONE',  ( 0.000000000000000000, -1.000000000000000000, 0.000000000000000000 ) ) ;
#14293 = CARTESIAN_POINT ( 'NONE',  ( 441.1634899080286232, 240.0000000000000000, -199.9999999999972431 ) ) ;
#14294 = CARTESIAN_POINT ( 'NONE',  ( 796.1575198192839480, -270.0090635724253048, 359.4546378042384163 ) ) ;
#14295 = APPLICATION_CONTEXT ( 'automotive_design' ) ;
#14296 = CARTESIAN_POINT ( 'NONE',  ( 785.3141322388236176, -117.7255117493292715, 364.4286716492789537 ) ) ;
#14297 = VERTEX_POINT ( 'NONE', #28613 ) ;
#14298 = CARTESIAN_POINT ( 'NONE',  ( 760.7433823573367135, -12.00906357242613609, -355.9930595647440441 ) ) ;
#14299 = AXIS2_PLACEMENT_3D ( 'NONE', #24860, #43333, #38977 ) ;
#14300 = CARTESIAN_POINT ( 'NONE',  ( 796.7737145352015204, -116.6346026584201780, -370.7187646348536987 ) ) ;
#14301 = AXIS2_PLACEMENT_3D ( 'NONE', #4854, #33050, #29355 ) ;
#14302 = CARTESIAN_POINT ( 'NONE',  ( 776.9566956441375396, -300.8965053807775689, 364.8461984189686405 ) ) ;
#14303 = DIRECTION ( 'NONE',  ( -0.000000000000000000, 1.000000000000000000, -0.000000000000000000 ) ) ;
#14304 = CARTESIAN_POINT ( 'NONE',  ( 809.0717654672305343, -28.91815448151699286, 360.1688906516309885 ) ) ;
#14305 = CARTESIAN_POINT ( 'NONE',  ( 782.5225473063381969, -238.2709662947833920, -375.2698199232970637 ) ) ;
#14306 = CARTESIAN_POINT ( 'NONE',  ( 808.3070685750230950, -186.9982390220563104, 361.1904061080339261 ) ) ;
#14307 = CARTESIAN_POINT ( 'NONE',  ( 781.7834795799800531, -82.81642084023846451, 315.0636971347436202 ) ) ;
#14308 = CARTESIAN_POINT ( 'NONE',  ( 989.9999999999992042, 56.60618624968560653, -350.0000000000000000 ) ) ;
#14309 = CARTESIAN_POINT ( 'NONE',  ( 814.8230680027162407, -293.8055962898685607, -333.7305795820267917 ) ) ;
#14310 = VECTOR ( 'NONE', #1222, 1000.000000000000000 ) ;
#14311 = CARTESIAN_POINT ( 'NONE',  ( 752.7379699480933368, -444.0090635724249069, 361.9858362298580232 ) ) ;
#14312 = CARTESIAN_POINT ( 'NONE',  ( 808.0189434323515343, -326.0891481129649492, -319.0252816721025511 ) ) ;
#14313 = FACE_BOUND ( 'NONE', #37627, .T. ) ;
#14314 = CARTESIAN_POINT ( 'NONE',  ( 763.2154366446407039, -357.6237781080501463, 321.4292242960311228 ) ) ;
#14315 = CARTESIAN_POINT ( 'NONE',  ( 782.4968714119720516, -34.81642084023861372, 305.0891759886411023 ) ) ;
#14316 = CARTESIAN_POINT ( 'NONE',  ( 797.8594530101008786, -397.5436935675100472, -322.1405469898980982 ) ) ;
#14317 = CARTESIAN_POINT ( 'NONE',  ( 776.9566956441375396, -36.89650538077844288, 364.8461984189686405 ) ) ;
#14318 = CARTESIAN_POINT ( 'NONE',  ( 798.0661480581538854, -98.53286901714187707, -309.5768839229118043 ) ) ;
#14319 = CARTESIAN_POINT ( 'NONE',  ( 798.0661480581538854, -218.5328690171414792, 309.5768839229118043 ) ) ;
#14320 = CARTESIAN_POINT ( 'NONE',  ( 756.5762568750052424, -27.18005720387500901, 348.7366044899774238 ) ) ;
#14321 = ADVANCED_FACE ( 'NONE', ( #10141 ), #39019, .T. ) ;
#14322 = ORIENTED_EDGE ( 'NONE', *, *, #33474, .T. ) ;
#14323 = CARTESIAN_POINT ( 'NONE',  ( 785.3687786644884454, -83.36187538569296862, -315.3201227861279676 ) ) ;
#14324 = CARTESIAN_POINT ( 'NONE',  ( 783.0433043558608688, -216.8965053807778816, -315.1538015810313027 ) ) ;
#14325 = CARTESIAN_POINT ( 'NONE',  ( 805.1927285166397041, -184.8164208402380950, 341.8018195045277707 ) ) ;
#14326 = CARTESIAN_POINT ( 'NONE',  ( 744.9990715423526808, -18.35105083532395298, -341.2370466360926002 ) ) ;
#14327 = CARTESIAN_POINT ( 'NONE',  ( 755.5713283507202505, -341.3618753856922012, 334.6858677611754729 ) ) ;
#14328 = CARTESIAN_POINT ( 'NONE',  ( 807.0960494954803153, -452.9681489794450613, -341.9322302743943851 ) ) ;
#14329 = CARTESIAN_POINT ( 'NONE',  ( 779.9999999999992042, 166.4563064324884465, 329.9999999999999432 ) ) ;
#14330 = VECTOR ( 'NONE', #29914, 999.9999999999998863 ) ;
#14331 = VERTEX_POINT ( 'NONE', #3678 ) ;
#14332 = CARTESIAN_POINT ( 'NONE',  ( 795.9930595647434757, -51.07832356259657303, 320.7433823573372820 ) ) ;
#14333 = CARTESIAN_POINT ( 'NONE',  ( 745.1792804349281596, -350.1908817542433212, -343.7566961878542884 ) ) ;
#14334 = EDGE_CURVE ( 'NONE', #17860, #18427, #10592, .T. ) ;
#14335 = CARTESIAN_POINT ( 'NONE',  ( 745.0891759886404770, -268.2709662947833067, 342.4968714119734159 ) ) ;
#14336 = CARTESIAN_POINT ( 'NONE',  ( 813.2346286133761168, 18.73985825558501972, 328.9521613784389160 ) ) ;
#14337 = CARTESIAN_POINT ( 'NONE',  ( 766.9102291470427417, -138.5545181178802636, -318.6633372737382501 ) ) ;
#14338 = CARTESIAN_POINT ( 'NONE',  ( 794.9819416627830151, -132.9982390220564810, -319.9864689768909898 ) ) ;
#14339 = CARTESIAN_POINT ( 'NONE',  ( 756.5762568750052424, -363.1800572038739006, -348.7366044899774238 ) ) ;
#14340 = EDGE_LOOP ( 'NONE', ( #35232, #8951, #31012, #27389 ) ) ;
#14341 = CARTESIAN_POINT ( 'NONE',  ( 792.2312462859673587, -299.9073299311468759, 307.2067596250082602 ) ) ;
#14342 = VECTOR ( 'NONE', #26745, 1000.000000000000000 ) ;
#14343 = CARTESIAN_POINT ( 'NONE',  ( 804.6401732501814195, -455.9581923679652391, 357.6484231659003967 ) ) ;
#14344 = CARTESIAN_POINT ( 'NONE',  ( 769.1273215169530886, -334.7146871989593251, 317.4527132478988847 ) ) ;
#14345 = CARTESIAN_POINT ( 'NONE',  ( -728.8365100919714905, 260.0000000000001705, -199.9999999999890861 ) ) ;
#14346 = VECTOR ( 'NONE', #13063, 1000.000000000000000 ) ;
#14347 = CARTESIAN_POINT ( 'NONE',  ( 793.9708237608222134, -142.9181544815166376, 319.2295555964448681 ) ) ;
#14348 = CARTESIAN_POINT ( 'NONE',  ( 757.8323909638827445, -26.63460265842045871, 352.1044303154654358 ) ) ;
#14349 = VERTEX_POINT ( 'NONE', #17069 ) ;
#14350 = CARTESIAN_POINT ( 'NONE',  ( 797.8822607201568644, -390.5545181178794678, -370.1134526219340160 ) ) ;
#14351 = CARTESIAN_POINT ( 'NONE',  ( 815.2698199232962679, 7.183579159761249500, -342.5225473063383674 ) ) ;
#14352 = CARTESIAN_POINT ( 'NONE',  ( 811.3240766477731540, -220.3726999360618208, 355.6651683502462902 ) ) ;
#14353 = CARTESIAN_POINT ( 'NONE',  ( 783.0433043558608688, -192.8965053807779668, 315.1538015810313027 ) ) ;
#14354 = CARTESIAN_POINT ( 'NONE',  ( 758.0580252608178853, -366.4527844766012095, -328.0187753319985404 ) ) ;
#14355 = CARTESIAN_POINT ( 'NONE',  ( 797.8594530101008786, 10.45630643248850866, 322.1405469898980982 ) ) ;
#14356 = CARTESIAN_POINT ( 'NONE',  ( 701.1634899080286232, 239.9999999999999147, -202.7499999999988916 ) ) ;
#14357 = CARTESIAN_POINT ( 'NONE',  ( 787.5531968255692163, -237.8272453906072599, -316.1348686366205811 ) ) ;
#14358 = CIRCLE ( 'NONE', #35749, 12.00000000000001066 ) ;
#14359 = CARTESIAN_POINT ( 'NONE',  ( 815.2698199232961542, -16.81642084023866701, 342.5225473063383106 ) ) ;
#14360 = PLANE ( 'NONE',  #6272 ) ;
#14361 = CARTESIAN_POINT ( 'NONE',  ( 814.5518280994195948, -399.7255117493283478, -332.4837098697145166 ) ) ;
#14362 = AXIS2_PLACEMENT_3D ( 'NONE', #2587, #36793, #44169 ) ;
#14363 = CARTESIAN_POINT ( 'NONE',  ( -789.9999999999992042, 205.0000000000000568, -319.9999999999999432 ) ) ;
#14364 = AXIS2_PLACEMENT_3D ( 'NONE', #996, #28737, #39139 ) ;
#14365 = CARTESIAN_POINT ( 'NONE',  ( 773.7305795820266212, -369.2817908451523294, 374.8230680027170365 ) ) ;
#14366 = CARTESIAN_POINT ( 'NONE',  ( -789.9999999999992042, 205.0000000000000568, -360.0000000000000000 ) ) ;
#14367 = CARTESIAN_POINT ( 'NONE',  ( 751.9810565676468741, -338.0891481129649492, 360.9747183278973921 ) ) ;
#14368 = CARTESIAN_POINT ( 'NONE',  ( 800.9747183278959710, -60.99823902205671544, -311.9810565676471583 ) ) ;
#14369 = CARTESIAN_POINT ( 'NONE',  ( 794.9819416627830151, -276.9982390220559978, -319.9864689768909898 ) ) ;
#14370 = LINE ( 'NONE', #28451, #4080 ) ;
#14371 = CARTESIAN_POINT ( 'NONE',  ( 785.3141322388236176, -429.7255117493282910, 364.4286716492789537 ) ) ;
#14372 = CARTESIAN_POINT ( 'NONE',  ( 754.7162404726377645, -206.7363362996982801, 339.4709603349214717 ) ) ;
#14373 = CARTESIAN_POINT ( 'NONE',  ( 815.3608509340175488, -50.73633629969874193, -341.2497674668889545 ) ) ;
#14374 = CARTESIAN_POINT ( 'NONE',  ( 761.2382568024794409, -87.62377810805102740, -356.9571628226838129 ) ) ;
#14375 = CARTESIAN_POINT ( 'NONE',  ( 747.3154664389472828, -115.9874144716872877, 326.4474001241230781 ) ) ;
#14376 = CARTESIAN_POINT ( 'NONE',  ( 785.3687786644885591, -419.3618753856918602, 315.3201227861280813 ) ) ;
#14377 = CIRCLE ( 'NONE', #40905, 9.999999999999980460 ) ;
#14378 = CARTESIAN_POINT ( 'NONE',  ( 810.1134526219336749, -152.5328690171416781, 357.8822607201570349 ) ) ;
#14379 = CARTESIAN_POINT ( 'NONE',  ( 771.2633955100217236, 0.09267006885218045942, -363.4237431249939618 ) ) ;
#14381 = VERTEX_POINT ( 'NONE', #34837 ) ;
#14380 = CARTESIAN_POINT ( 'NONE',  ( 795.9930595647434757, -99.07832356259642381, -320.7433823573372820 ) ) ;
#14382 = CARTESIAN_POINT ( 'NONE',  ( 781.7834795799800531, -106.8164208402383935, -315.0636971347436202 ) ) ;
#14383 = VECTOR ( 'NONE', #4270, 1000.000000000000000 ) ;
#14384 = CARTESIAN_POINT ( 'NONE',  ( 758.6633372737375112, -404.5328690171409107, -326.9102291470432533 ) ) ;
#14386 = CARTESIAN_POINT ( 'NONE',  ( 800.2193346964446619, -234.9982390220561683, 355.1360043628816925 ) ) ;
#14385 = CARTESIAN_POINT ( 'NONE',  ( 781.8018195045266339, -214.2709662947834488, 365.1927285166406705 ) ) ;
#14387 = CARTESIAN_POINT ( 'NONE',  ( 812.6845335610512393, -391.9874144716864066, -353.5525998758768651 ) ) ;
#14388 = CARTESIAN_POINT ( 'NONE',  ( 879.9999999999992042, 430.0000000000002842, -320.0000000000000568 ) ) ;
#14389 = EDGE_LOOP ( 'NONE', ( #25327, #28409, #718, #804, #33351, #7200 ) ) ;
#14390 = CARTESIAN_POINT ( 'NONE',  ( 758.0580252608178853, -414.4527844766010389, 328.0187753319985404 ) ) ;
#14391 = EDGE_LOOP ( 'NONE', ( #21314, #3770 ) ) ;
#14392 = CARTESIAN_POINT ( 'NONE',  ( 792.3570229623688874, -261.1800572038741848, -373.1304606946836202 ) ) ;
#14393 = CARTESIAN_POINT ( 'NONE',  ( 777.5031285880264704, -166.8164208402382087, 374.9108240113588408 ) ) ;
#14394 = CONICAL_SURFACE ( 'NONE', #1837, 8.025000000000003908, 0.7853981633974428389 ) ;
#14395 = CARTESIAN_POINT ( 'NONE',  ( 761.4292242960306112, -281.4636090269706870, 323.2154366446414429 ) ) ;
#14396 = ORIENTED_EDGE ( 'NONE', *, *, #14961, .T. ) ;
#14397 = CARTESIAN_POINT ( 'NONE',  ( 788.7631598425961101, -193.4419599262325278, 305.7194118038759143 ) ) ;
#14398 = CARTESIAN_POINT ( 'NONE',  ( 802.1676090361155502, -254.6346026584197091, -327.8955696845344505 ) ) ;
#14399 = AXIS2_PLACEMENT_3D ( 'NONE', #14082, #42029, #28258 ) ;
#14400 = VERTEX_POINT ( 'NONE', #31381 ) ;
#14401 = CARTESIAN_POINT ( 'NONE',  ( 803.6646147819161570, -353.9073299311467053, -348.8264449731210561 ) ) ;
#14402 = CARTESIAN_POINT ( 'NONE',  ( 762.3223304703356007, -31.54369356751135456, -322.3223304703362828 ) ) ;
#14403 = VECTOR ( 'NONE', #35136, 1000.000000000000000 ) ;
#14404 = CARTESIAN_POINT ( 'NONE',  ( 784.0799538623451781, -227.8055962898687596, 364.6971507214555572 ) ) ;
#14405 = CYLINDRICAL_SURFACE ( 'NONE', #22555, 9.999999999999980460 ) ;
#14406 = FACE_OUTER_BOUND ( 'NONE', #7190, .T. ) ;
#14407 = ORIENTED_EDGE ( 'NONE', *, *, #44162, .T. ) ;
#14408 = CARTESIAN_POINT ( 'NONE',  ( 781.8018195045266339, -22.27096629478410250, -365.1927285166406705 ) ) ;
#14409 = LINE ( 'NONE', #34726, #12869 ) ;
#14410 = CARTESIAN_POINT ( 'NONE',  ( 787.4999999999992042, -462.9681489794447771, 309.9999999999998863 ) ) ;
#14411 = ORIENTED_EDGE ( 'NONE', *, *, #39421, .F. ) ;
#14412 = CARTESIAN_POINT ( 'NONE',  ( 773.7305795820266212, -273.2817908451526137, -374.8230680027170365 ) ) ;
#14413 = VECTOR ( 'NONE', #21404, 1000.000000000000114 ) ;
#14414 = CARTESIAN_POINT ( 'NONE',  ( 804.1009440267234822, -143.4636090269711701, 314.0944755984392600 ) ) ;
#14415 = VECTOR ( 'NONE', #9819, 1000.000000000000000 ) ;
#14417 = CARTESIAN_POINT ( 'NONE',  ( 756.5762568750052424, -243.1800572038743269, -348.7366044899774238 ) ) ;
#14416 = LINE ( 'NONE', #28732, #36423 ) ;
#14418 = CARTESIAN_POINT ( 'NONE',  ( 760.5453621957607311, -381.0783235625954717, -323.8424801807151425 ) ) ;
#14419 = CARTESIAN_POINT ( 'NONE',  ( 571.1634899080285095, 259.9999999999999432, -208.0249999999981014 ) ) ;
#14420 = CARTESIAN_POINT ( 'NONE',  ( 790.9844846989617508, -118.3726999360621619, -317.2208543904092721 ) ) ;
#14421 = VECTOR ( 'NONE', #34534, 1000.000000000000000 ) ;
#14422 = CARTESIAN_POINT ( 'NONE',  ( 989.9999999999992042, 239.9999999999998863, -350.0000000000000000 ) ) ;
#14423 = CARTESIAN_POINT ( 'NONE',  ( 811.6461892240364477, -4.714687198960358039, -324.1737431748509835 ) ) ;
#14424 = CARTESIAN_POINT ( 'NONE',  ( 815.2698199232962679, -304.8164208402376971, -342.5225473063383674 ) ) ;
#14425 = FACE_OUTER_BOUND ( 'NONE', #16829, .T. ) ;
#14426 = CARTESIAN_POINT ( 'NONE',  ( 755.0636971347428243, -4.270966294784170003, 341.7834795799807353 ) ) ;
#14427 = CARTESIAN_POINT ( 'NONE',  ( 814.4686193811664907, -267.2817908451526137, 346.2056067578752732 ) ) ;
#14428 = CARTESIAN_POINT ( 'NONE',  ( 758.0141637701419768, -207.0783235625960685, -367.2620300519063790 ) ) ;
#14429 = CARTESIAN_POINT ( 'NONE',  ( 792.3570229623688874, -213.1800572038743553, 373.1304606946836202 ) ) ;
#14430 = CARTESIAN_POINT ( 'NONE',  ( 759.0252816721024374, -432.9982390220555999, -368.0189434323527280 ) ) ;
#14431 = PLANE ( 'NONE',  #10644 ) ;
#14432 = CARTESIAN_POINT ( 'NONE',  ( 788.8264449731200330, -309.1800572038740711, 363.6646147819171233 ) ) ;
#14433 = CARTESIAN_POINT ( 'NONE',  ( 793.0897708529556667, -78.55451811788046257, 361.3366627262616362 ) ) ;
#14434 = ADVANCED_FACE ( 'NONE', ( #3200, #35521 ), #42016, .F. ) ;
#14435 = CARTESIAN_POINT ( 'NONE',  ( 769.0155153010367712, -82.37269993606227558, 362.7791456095907279 ) ) ;
#14436 = CARTESIAN_POINT ( 'NONE',  ( 805.0264073115434940, 17.64894916467593688, -339.4763451958999099 ) ) ;
#14437 = ADVANCED_BREP_SHAPE_REPRESENTATION ( '', ( #17465, #26858 ), #41617 ) ;
#14438 = VECTOR ( 'NONE', #10521, 1000.000000000000000 ) ;
#14439 = LINE ( 'NONE', #795, #16618 ) ;
#14440 = DIRECTION ( 'NONE',  ( -1.000000000000000000, -0.000000000000000000, -0.000000000000000000 ) ) ;
#14442 = CARTESIAN_POINT ( 'NONE',  ( 794.9819416627830151, -348.9982390220558273, 319.9864689768909898 ) ) ;
#14441 = CARTESIAN_POINT ( 'NONE',  ( 758.6633372737375112, -164.5328690171416781, 326.9102291470432533 ) ) ;
#14443 = EDGE_LOOP ( 'NONE', ( #33044, #37887, #18026, #18432 ) ) ;
#14444 = CARTESIAN_POINT ( 'NONE',  ( 772.3691319403857278, -311.2601417444139429, -315.8894580844506663 ) ) ;
#14445 = CARTESIAN_POINT ( 'NONE',  ( 759.9864689768902508, -122.0891481129656171, 354.9819416627836404 ) ) ;
#14446 = CARTESIAN_POINT ( 'NONE',  ( 746.7653713866222915, -305.2601417444139429, -351.0478386215610271 ) ) ;
#14447 = CARTESIAN_POINT ( 'NONE',  ( 911.9999999999992042, 154.9999999999998863, 359.9749999999999659 ) ) ;
#14448 = CARTESIAN_POINT ( 'NONE',  ( 813.9316612368132837, -415.4419599262318457, 348.6739635108323228 ) ) ;
#14449 = VERTEX_POINT ( 'NONE', #11060 ) ;
#14450 = CARTESIAN_POINT ( 'NONE',  ( 785.3141322388236176, -333.7255117493286320, 364.4286716492789537 ) ) ;
#14451 = AXIS2_PLACEMENT_3D ( 'NONE', #8647, #19466, #19036 ) ;
#14452 =( BOUNDED_SURFACE ( )  B_SPLINE_SURFACE ( 3, 2, ( 
 ( #6794, #44695, #23874, #13967, #10262, #3101, #13744, #37994, #16974, #31050, #17436, #45149, #13510, #27583, #41688, #10042, #31516, #28040, #785, #39833, #25252, #561, #39362, #322, #21565, #18356, #7493, #42821, #10964, #36118, #8176, #35890, #17666, #22241, #42355, #36338, #29193, #28256, #14426, #32437, #24803, #14188, #11405, #7716, #22029, #7961, #31728, #43043, #10724, #25033, #32199, #14885, #96, #21797, #14664, #4264, #28505, #35648, #28963, #4020, #11182, #39143, #4483, #38923, #25493, #7275, #21346, #35422, #3794, #43272, #17885, #42603, #39605, #31952, #18121, #18575, #32658, #1000, #15103, #28740, #11643, #25721, #43712, #25932, #9301, #12088, #26165, #12749, #33322, #16222, #43943, #40039, #1232, #26394, #1452, #19689, #43492, #19455, #8395, #44394, #8847, #40279, #40495, #33781, #4696, #1666, #11859, #8633, #22464, #22695, #12319, #36572, #36794, #9061, #4926, #1897, #15553, #19024, #40707, #33116, #5360, #22915, #29420, #15771, #16005, #37005, #5151, #19235, #32887, #29857, #15338, #33548, #30086, #12532, #5598, #44170, #26829, #29633, #26607, #23129, #37232, #2132, #30299, #40935, #23369, #18797, #19919, #34638, #14550, #3690, #13856, #3457, #45500, #37472, #35083, #24450, #3909, #42481, #18004, #32077, #20991, #213, #445, #11071, #7381, #17777, #31624, #30463, #45258, #27932, #42028, #31843, #20759, #17084, #2995, #10374, #38554, #21457, #17552, #31162, #6910, #5834, #14307, #35313, #28629, #13619, #14081, #28379, #28156, #10153, #10847, #24918, #24683, #39032, #35535, #41805, #27701, #38337, #24229, #6683, #34851, #3215, #17306, #42707, #31395, #42248, #10605, #38800, #7157, #21233, #11763, #32544, #21683, #18682, #890, #19137, #39943, #40152, #1120, #32772, #5046, #11295, #25829, #29740, #42930, #14992, #22584, #18465, #43819, #32323, #18919, #15662, #39492, #25139, #33225, #11974, #39252, #7605, #15232, #8287, #1564, #29079, #18247, #35776, #43167, #4153, #677, #11534, #4590, #14778, #28849, #8518, #25374, #7848, #29322, #29533, #25616, #36454, #36011, #21926, #36686, #33014, #39728, #4375, #8076, #43396, #15456, #4818, #22139, #36228, #22350, #1353, #43607, #26040, #44762, #37120, #16582, #37819, #41292, #16814, #30421, #40395, #44519, #26283, #5258, #36905, #22813, #2474, #34350, #33671, #8746, #30665, #19350, #26726, #6168, #9643, #12878, #33433, #2719, #20258, #34108, #5940, #1778, #9185, #23708, #5478, #13119, #44061, #9418, #23027, #12427, #27199, #26506, #26964, #2246, #15890, #23260, #23486, #41060, #30201, #40827, #29975, #44291, #40607, #33892, #2020, #20030, #30892, #5722, #12205, #8958, #12646, #19576, #37361, #37586, #16115, #19809, #16340, #24868, #27418, #41515, #21411, #10546, #20707, #10325, #6634, #44987, #41984, #31340, #10795, #3643, #38985, #7335, #27886, #7104, #35487, #17951, #14255, #24623, #38500, #6853, #6414, #34800, #3163, #38744, #27643, #23937, #9865, #17253, #45448, #38287, #13808, #28102, #3861, #20933, #24399, #35030, #41753, #3407, #45681, #17500, #31578, #14034, #17730, #13343, #42198, #38058, #20496, #34586, #2942, #17031, #31107, #10104, #21184, #45205, #13567, #35264, #31794, #163, #28322, #24180, #42423, #42663, #25321, #7557, #36641, #39434, #7788, #40098, #14942, #43553, #25560, #21634, #28575, #8021, #28801, #1304, #25092, #1066, #35716, #25990, #36180, #21868, #22090, #15400, #32021, #29026, #39206, #35956, #4095, #4323, #39674, #18192, #42879, #32720, #32267, #11026, #25781, #4540, #36400, #22303, #393, #11709, #625, #18414, #14727, #4996, #32493, #843, #8460, #43111, #11919, #18633, #11246, #11480, #15176, #29265, #29482, #43341, #39892, #8234, #22531, #4762, #18866, #32958, #14498, #19089, #16066, #26233, #22974, #40346, #8908, #26676, #5208, #12381, #23436, #19297, #16290, #29923, #33381, #9369, #1726, #19758, #9129, #43769, #30149, #30372, #37305, #37070, #33616, #1514, #5423, #15609, #40771, #40560, #26900, #19985, #12598, #27150, #8698, #19517, #44008, #1968, #5667, #15830, #12820, #26458, #44703, #29693, #12149, #41237, #44464, #44239, #23196, #33844, #33177, #2198, #41008, #30603, #37537, #13064, #9596, #5896, #34061, #23656, #37767, #2422, #16523, #22763, #36858, #13290, #27591, #10053, #17444, #34531, #30838, #2660, #24123, #41696, #45156, #20656, #34976, #28264, #13752, #34748, #27832, #2889, #38231, #6801, #6578, #31286, #13518, #24567, #42364, #24346, #6116, #10731, #44932, #24811, #17675, #16758, #20879, #27367, #41462, #45628, #41927, #10492, #42142, #20207, #31525, #9815, #3108, #23882, #34289, #17198, #45390, #14196, #10269, #31736, #38450, #38004, #6358, #3351, #16981, #21128, #20440, #13976, #31057, #103, #28047, #38684, #7042, #35212, #3587, #35898, #330, #42827, #14432, #28746, #792, #25039, #32206, #43281, #39149, #36125, #4028, #7501, #29202, #21573, #39613, #28970, #17891, #4272, #4490, #11415, #11188, #7724, #21352, #25260, #35430, #14892, #14670, #1008, #39841, #32444, #1242, #28513, #39370, #18127, #21803, #25500, #35655, #32665, #568, #18806, #3801, #31959, #15346, #18582, #18363, #43053, #7969, #38931, #22036, #15114, #4704, #11652, #32896, #29426, #25728, #8183, #43499, #11866, #22248, #36345, #7282, #42610, #10970, #1672, #29866, #37241, #8640, #4936, #22472, #43949, #15777, #19241, #40503, #9068, #2356, #33556, #8854, #1904, #22703, #12328, #26614, #26401, #5366, #33328, #44401, #16455, #44176, #25939, #30538, #19032, #44640, #37480, #36579, #36801, #40046, #5604, #23135, #8403, #33123, #16013, #2139, #22921, #43718, #30307, #19698, #12540, #12755, #26835, #29639, #1459, #26173, #12094, #15559, #40285, #5157, #37013, #33788, #19461, #30094, #16228, #40713, #40944, #9307, #23377, #5841, #19927, #34002, #34471, #6979, #27765, #27989, #34695, #20600, #38618, #44873, #45324, #17610, #30782, #2831, #10434, #6290, #31679, #20144, #6743, #3524, #27313, #13001, #21064, #45564, #27089, #41181, #3053, #41867, #35147, #20375, #6054, #9535, #16923, #23599, #37705, #31003, #38173, #2596, #34221, #42084, #16697, #13235, #6522, #17378, #45101, #24288, #23820, #41406, #24510, #20818, #13458, #9756, #27527, #17143, #3283, #38394, #41627, #37932, #9986, #24055, #31227, #13686, #13917, #10211, #31461, #34918, #29141, #4649, #18310, #28211, #32389, #14139, #38868, #24753, #10669, #36073, #22199, #21515, #42305, #4440, #7223, #14618, #25674, #43225, #740, #21294, #36290, #39787, #21984, #39559, #35372, #42768, #11596, #15053, #25200, #3747, #7442, #18744, #14371, #46, #8135, #32607, #17834, #31902, #35842, #14839, #274, #39092, #28452, #42551, #35594, #10913, #24981, #3970, #39312, #18065, #32147, #510, #28690, #11129, #7666, #18526, #21744, #11357, #4217, #28911, #42993, #7914, #25437, #949, #40224, #26345, #23085, #12486, #19192, #33070, #22412, #4878, #22870, #11816, #19643, #12041, #37184 ),
 ( #26563, #39997, #29810, #30257, #2084, #12269, #25885, #8584, #1185, #44120, #30038, #9257, #8346, #40449, #9014, #22648, #18980, #5548, #40661, #19411, #33735, #16176, #36516, #1409, #15512, #29592, #43669, #26108, #36746, #5104, #44349, #33278, #1624, #12705, #37430, #26785, #8803, #33499, #15723, #29377, #36962, #43889, #40890, #1849, #23327, #5315, #15955, #5786, #32834, #15293, #43449, #37650, #41354, #17316, #13184, #24460, #27034, #13630, #2304, #3226, #27941, #9485, #45052, #24239, #27266, #31174, #30731, #42038, #34865, #27713, #9704, #5999, #23768, #13406, #10163, #45270, #6230, #20092, #23547, #34167, #9929, #44587, #6693, #44825, #38348, #45513, #31407, #38568, #38124, #16403, #6476, #33953, #12948, #41133, #30483, #20772, #10384, #37881, #2539, #13866, #16643, #34416, #19875, #20321, #20553, #2783, #16875, #30958, #41818, #27478, #41576, #24002, #34649, #3008, #17096, #45725, #14317, #21000, #18260, #4164, #29700, #14090, #14563, #28858, #42493, #24694, #11306, #686, #39260, #39502, #7859, #10617, #31633, #7168, #38812, #42258, #28165, #35321, #21241, #14786, #3699, #17786, #32333, #12157, #42939, #28637, #7615, #28391, #3470, #458, #10859, #1520, #21692, #21938, #42716, #11080, #32554, #31851, #35785, #26240, #223, #24927, #4386, #39041, #6922, #7390, #25384, #43775, #21466, #35093, #15615, #36023, #17561, #35544, #25148, #18475, #3919, #18014, #32086, #40352, #1974, #16763, #20212, #16072, #19764, #29930, #30843, #34296, #16528, #34067, #1733, #37311, #37773, #9601, #33850, #33388, #30156, #8704, #5901, #37543, #44939, #15838, #2203, #30612, #44246, #12387, #44709, #2427, #26907, #27155, #41244, #44014, #19303, #40566, #26465, #8914, #22982, #37077, #5429, #13069, #19524, #33623, #19990, #13296, #23661, #16296, #41014, #12604, #36864, #30377, #26682, #2667, #9374, #6122, #44470, #12827, #22770, #40779, #23441, #5216, #9135, #23202, #5673, #20661, #31966, #34536, #21133, #17899, #41704, #336, #7287, #14202, #41467, #9820, #17449, #42147, #3807, #34753, #20447, #27372, #3114, #23888, #21360, #17204, #6806, #16986, #38010, #10738, #35436, #31063, #20885, #31741, #31291, #38690, #38238, #6364, #42369, #35217, #45396, #45161, #13759, #34980, #17681, #7049, #27837, #27596, #13523, #10058, #31532, #2895, #28270, #6584, #110, #24128, #24816, #41932, #45633, #10277, #13982, #24351, #38455, #3358, #28054, #38936, #10498, #24573, #3593, #43288, #42616, #4277, #4710, #22254, #39620, #10976, #18135, #29209, #32213, #22041, #11420, #25046, #32449, #18587, #7974, #21809, #18369, #28520, #35904, #39156, #43058, #25267, #15119, #39846, #28978, #18813, #7507, #797, #42833, #14897, #36133, #575, #1016, #28753, #32904, #21579, #35662, #1249, #32671, #39377, #25507, #11195, #14441, #4495, #11657, #4035, #14676, #7731, #25733, #8188, #36352, #15352, #29431, #24963, #21276, #3508, #17593, #17127, #31443, #13900, #35356, #38380, #34681, #6509, #27974, #45549, #3265, #24495, #38852, #32128, #31664, #38602, #31, #6728, #42069, #10652, #10419, #35129, #17359, #28432, #494, #28196, #9969, #14599, #3039, #28672, #21498, #20587, #20802, #24732, #31212, #45307, #3730, #14124, #14353, #256, #24038, #17818, #13668, #6959, #27749, #38159, #21043, #42289, #18047, #7204, #35576, #31886, #41851, #10196, #42530, #34899, #39076, #24274, #10895, #7425, #3954, #1167, #32590, #18728, #12023, #42751, #39772, #4200, #933, #18292, #15036, #4632, #28893, #36057, #1393, #42975, #39981, #7897, #35821, #32367, #8330, #1610, #22393, #32816, #29363, #4421, #39294, #36275, #18510, #36730, #11801, #26090, #15276, #43433, #22631, #11340, #25870, #15709, #14820, #29124, #40204, #43208, #11112, #722, #36497, #33264, #25419, #25182, #5088, #29577, #7648, #21727, #4860, #18961, #19179, #11579, #39540, #21971, #25659, #8120, #22181, #33056, #15497, #43653, #8565, #13164, #37864, #19397, #9237, #34148, #37168, #41112, #40647, #6210, #44807, #37630, #19622, #1828, #5527, #23308, #20073, #9465, #16159, #30020, #33482, #15936, #19855, #8787, #16624, #9000, #2518, #9685, #27243, #34394, #2286, #12251, #16385, #43872, #22855, #36948, #40435, #30710, #20303, #33718, #26330, #41335, #5301, #44333, #23749, #2765, #30464, #44106, #29792, #12470, #5981, #23528, #26549, #26768, #23070, #2067, #37409, #30241, #12688, #40873, #5767, #27013, #33935, #44566, #12927, #38794, #6677, #34632, #21227, #10601, #3450, #3685, #17772, #20538, #41558, #17076, #2989, #6459, #38103, #45252, #31154, #24675, #23983, #13388, #7150, #6903, #35308, #31838, #16859, #42243, #27460, #10148, #13611, #21452, #24223, #38331, #24912, #45494, #28372, #10369, #27695, #9911, #38549, #41798, #208, #20754, #31620, #34844, #10840, #20982, #3209, #35078, #14302, #30939, #13850, #17299, #31389, #27928, #42023, #24445, #17547, #45723, #42474, #14076, #28151, #39026, #7376, #35529, #45032, #4586, #39721, #28621, #886, #15228, #22133, #21918, #18459, #32069, #36006, #441, #25611, #25369, #11756, #4810, #43161, #11968, #11067, #4369, #28844, #32539, #36222, #4147, #43389, #671, #29527, #14543, #42703, #26036, #29315, #39483, #14988, #11290, #3904, #29075, #11528, #15451, #8280, #43602, #40149, #8071, #25823, #8512, #22580, #18914, #39935, #18677, #32768, #25134, #7843, #1113, #22344, #32315, #39248, #7600, #36447, #33007, #42924, #1347, #17999, #21678, #35769, #18241, #14773, #3465, #24689, #21463, #10613, #220, #14087, #39257, #42936, #39038, #20768, #25381, #45509, #11303, #32329, #31404, #17558, #35541, #39498, #28162, #42255, #28855, #3696, #683, #14314, #10380, #17313, #42488, #31630, #35782, #13862, #3916, #42034, #14783, #24924, #38808, #10855, #4160, #34859, #17783, #27938, #7164, #24456, #21238, #28386, #6917, #35318, #25145, #20997, #18011, #8363, #35090, #11077, #31848, #32083, #7387, #38563, #453, #14557, #28634, #42713, #7612, #3223, #21689, #18255, #29540, #29328, #15669, #8753, #1359, #15896, #14999, #39948, #32779, #8293, #26049, #8083, #1571, #4595, #33443, #36018, #4381, #29982, #19144, #43402, #18926, #15239, #7855, #4824, #22357, #19357, #12211, #1786, #44069, #36462, #29749, #12434, #26513, #22819, #33231, #15462, #43615, #29086, #11768, #25836, #43827, #36234, #32550, #18471, #33021, #11981, #1126, #40160, #36694, #21933, #8525, #22590, #5053, #18690, #26290, #40403, #36911, #5265, #896, #43173, #11541, #25623, #39734, #22145, #19583, #17039, #6423, #5486, #37369, #41301, #2028, #37129, #34358, #30673, #44995, #30901, #40614, #20267, #33678, #33900, #16122, #34116, #13351, #2727, #26972, #40836, #30208, #12653, #44770, #44298, #27426, #19817, #41523, #20506, #23946, #45213, #13129, #23034, #27207, #8965, #26733, #9194, #23269, #9875, #31117, #16349, #5731, #38066, #2254, #9427, #34594, #2951, #9651, #30429, #13576, #44529, #16823, #12887 ),
 ( #41069, #23494, #37594, #5948, #20039, #2483, #16591, #23716, #37827, #6178, #38990, #35271, #14260, #35038, #24189, #21191, #3414, #21638, #42429, #42669, #3649, #17736, #7563, #13815, #28328, #32273, #45455, #17508, #25097, #20942, #631, #34809, #21416, #18197, #41990, #27653, #35725, #14503, #41762, #10112, #31799, #10800, #4102, #31586, #20715, #38296, #45688, #6642, #3170, #14041, #7111, #17261, #31348, #11031, #27893, #10333, #170, #32028, #28110, #7340, #38509, #24406, #39211, #35492, #42206, #6860, #10554, #24874, #24632, #3867, #38753, #17958, #399, #28581, #18639, #35961, #4545, #22308, #848, #8027, #19095, #14948, #11924, #25567, #29031, #5002, #43118, #15408, #4768, #39441, #11714, #25995, #32963, #32725, #29271, #42884, #1073, #11252, #36405, #36185, #22537, #16231, #8239, #23380, #21873, #15182, #39679, #43348, #1309, #11487, #8467, #22095, #40947, #25326, #7797, #37483, #40103, #25785, #39897, #18872, #14733, #29487, #43558, #26838, #33184, #9310, #5844, #36646, #2142, #19930, #34005, #30310, #44404, #12759, #28806, #4329, #18419, #32498, #13690, #30785, #27092, #44643, #20378, #37935, #41409, #16927, #31232, #24514, #9990, #31007, #24059, #44876, #6293, #3058, #34475, #27531, #9759, #20822, #38623, #20604, #2359, #6983, #41184, #21068, #13921, #13004, #13238, #17147, #9538, #23602, #41871, #38177, #6748, #38398, #16458, #27769, #37708, #23824, #6057, #30541, #2835, #45105, #10439, #13462, #27993, #41631, #20148, #34224, #6525, #27316, #17382, #2599, #45328, #16700, #42088, #10215, #3287, #34699, #24292, #34923, #31464, #45569, #35598, #7671, #35376, #28916, #31906, #15059, #17614, #31683, #11600, #744, #10917, #514, #42555, #35151, #32151, #21521, #953, #39563, #29145, #43229, #18069, #42997, #25678, #8139, #4444, #14843, #28694, #42773, #42309, #24986, #39096, #11363, #17839, #14144, #50, #7446, #3975, #28456, #14622, #18314, #39791, #11133, #25205, #39315, #278, #21749, #35846, #4221, #32393, #25442, #7918, #3528, #21988, #28215, #10673, #24757, #38872, #7227, #21298, #14375, #36077, #3751, #18530, #32612, #12273, #26566, #12489, #22203, #1852, #32838, #15515, #43453, #26788, #29595, #43673, #30260, #5107, #33739, #15726, #11820, #18750, #43894, #18983, #37188, #15297, #36965, #25888, #16179, #26348, #12044, #40452, #5552, #36295, #19195, #29381, #26114, #40001, #40228, #29814, #8349, #8587, #40664, #22417, #19414, #33073, #36520, #9018, #4881, #22874, #8806, #1189, #33282, #33504, #5319, #22651, #36749, #4653, #1627, #1412, #15959, #30042, #44123, #23088, #19646, #2088, #44352, #12709, #40893, #41821, #12951, #33956, #9488, #27037, #44591, #30486, #37654, #23551, #3011, #2307, #41136, #6479, #13870, #20556, #16878, #41579, #16647, #5790, #2786, #30734, #3231, #24006, #24242, #30961, #45055, #34868, #6002, #9933, #27945, #20095, #44828, #6696, #2543, #9261, #16406, #17099, #45517, #34170, #23330, #17320, #10166, #37433, #19879, #13410, #38128, #31410, #13187, #27269, #41358, #9708, #23771, #37884, #6234, #34419, #20324, #27481, #38351, #34652, #31179, #45274, #13633, #27716, #20775, #7170, #4389, #11310, #4166, #31854, #14094, #3702, #35546, #32336, #21694, #28395, #42260, #31636, #28168, #32090, #21006, #28861, #21244, #690, #21940, #25387, #902, #14565, #24463, #28640, #10388, #35097, #3473, #6925, #14788, #18480, #17789, #38571, #42942, #17564, #10863, #36026, #39506, #42718, #3, #32558, #15005, #18262, #35789, #10620, #39044, #7862, #42042, #21468, #24697, #226, #38815, #7618, #39262, #35324, #14319, #3922, #42495, #24930, #11082, #7394, #18017, #460, #25152, #22363, #33683, #36241, #22823, #19588, #43407, #2033, #8970, #15900, #43178, #11547, #19149, #43833, #5493, #36468, #22152, #29093, #4830, #25630, #23039, #18933, #8532, #18695, #39740, #12439, #37134, #32785, #22596, #33449, #33028, #40408, #39955, #8090, #44073, #36917, #1365, #1135, #15469, #36699, #19364, #8757, #29547, #29335, #15246, #11773, #33235, #4601, #29987, #8299, #1793, #25843, #26519, #43623, #1576, #11990, #15676, #26056, #40167, #5057, #29756, #40619, #12217, #26296, #5271, #20510, #12658, #30678, #41766, #45218, #34363, #26738, #6646, #10117, #38070, #9879, #23274, #13134, #13580, #31122, #41306, #9200, #23499, #30212, #27429, #13355, #38300, #37377, #23720, #6429, #5953, #33905, #34598, #23951, #2734, #2956, #17043, #19822, #40840, #16355, #2258, #5735, #30435, #44534, #12894, #27659, #26978, #41078, #41527, #20720, #24193, #37832, #16827, #37600, #9434, #9657, #20043, #34814, #30906, #16127, #6182, #20272, #44303, #45000, #34121, #2487, #16596, #44776, #27212, #10560, #25333, #28811, #24637, #28332, #38514, #31354, #32279, #11257, #6866, #42435, #7568, #38758, #14508, #14046, #39447, #18203, #11035, #7115, #20946, #21195, #10804, #39216, #28586, #35275, #3417, #35043, #17512, #38994, #27898, #35730, #28116, #21644, #42891, #635, #7804, #21421, #45459, #35497, #17265, #41994, #10337, #13819, #4108, #21879, #3653, #24410, #14737, #31590, #17741, #3175, #45693, #3871, #42210, #31804, #173, #25101, #42672, #14264, #24879, #7344, #17963, #32032, #405, #43353, #4336, #1526, #33190, #12393, #29038, #43565, #12163, #25791, #8034, #40358, #29707, #22545, #22777, #36871, #39686, #14954, #36190, #22100, #25573, #11493, #18643, #4552, #43783, #43123, #32732, #15623, #40573, #26247, #11934, #36651, #11720, #32505, #29493, #39905, #29937, #5010, #5222, #26001, #40111, #15845, #1078, #19101, #8919, #15191, #8246, #33396, #29276, #35968, #22313, #8710, #26472, #36413, #18425, #44020, #19311, #854, #4774, #18879, #32970, #8474, #1314, #1742, #15415, #2903, #5438, #19531, #45170, #34304, #44477, #34074, #30385, #22989, #19996, #9381, #34543, #27380, #16994, #31070, #5907, #30852, #13530, #41711, #38018, #2676, #16537, #30620, #30162, #12834, #26914, #16771, #5680, #1980, #33630, #41022, #23448, #16302, #37549, #6129, #27604, #44717, #2435, #13078, #19771, #27163, #23668, #41251, #9607, #37781, #41476, #37082, #20220, #16078, #44253, #12612, #26689, #40786, #9143, #33857, #44948, #23211, #37322, #13304, #9828, #23898, #6373, #2211, #20455, #20669, #3365, #31298, #14683, #17457, #31540, #18142, #38698, #21587, #3602, #45404, #6591, #31748, #6814, #25053, #3122, #24824, #13768, #4044, #14209, #45641, #119, #39165, #10067, #7057, #17211, #13989, #27845, #28061, #17689, #41939, #42154, #14448, #10284, #7294, #20892, #24358, #345, #38462, #10746, #28277, #34760, #21141, #21369, #42378, #10505, #24581, #38246, #35224, #34990, #38944, #35445, #17906, #10984, #3814, #32222, #31974, #582, #35669, #28528, #42623, #7515, #28760, #24135, #36359, #29217, #32914, #1257, #42840, #4718, #39386, #25514, #4284, #36595, #39628, #7982, #8417, #18594, #25950, #15128, #18375, #7740, #43297, #28985, #43512 ),
 ( #39854, #11664, #21818, #32678, #18822, #25740, #22049, #4502, #25276, #36140, #35911, #8195, #1025, #15360, #29438, #22262, #22485, #32455, #11879, #11428, #40057, #11204, #803, #14903, #43066, #18298, #20806, #34906, #14826, #3959, #14128, #3735, #35, #38384, #35360, #24741, #4206, #42755, #32376, #729, #21282, #499, #28900, #11347, #7654, #18052, #31890, #262, #45553, #28200, #42294, #32134, #21051, #17363, #3271, #10658, #38858, #31668, #7209, #21503, #42981, #14359, #17823, #28439, #35134, #42538, #39082, #10902, #24968, #7430, #11118, #6732, #35581, #31449, #13904, #27978, #21732, #14606, #42073, #10422, #24499, #28678, #25187, #38607, #39299, #35829, #6966, #3513, #17597, #32823, #39548, #36737, #22640, #1838, #18517, #33063, #1617, #15284, #43213, #29802, #19185, #12032, #12258, #26339, #29129, #4429, #25665, #11587, #15043, #939, #8126, #39778, #33271, #32596, #22189, #5095, #30029, #15716, #1400, #26100, #1175, #21976, #18970, #29369, #19404, #40212, #40442, #15504, #29584, #5308, #36282, #8575, #44113, #4638, #43440, #22862, #18736, #25425, #11808, #43881, #15947, #25877, #7905, #33490, #8794, #36062, #39990, #43660, #36955, #8338, #22401, #36505, #4868, #19862, #35260, #38110, #33942, #37637, #2074, #40654, #41563, #21180, #16166, #5988, #16864, #2294, #23756, #23315, #3639, #27465, #20309, #16392, #30248, #30471, #20080, #2772, #37870, #44575, #12695, #44340, #26775, #2527, #37176, #45040, #37419, #30945, #6465, #9917, #17726, #30719, #9007, #44814, #26556, #5535, #19632, #23077, #13395, #31789, #12934, #33727, #23988, #40881, #27022, #12477, #41121, #9245, #9474, #23536, #5776, #34155, #16631, #13171, #27252, #34402, #41343, #9692, #6218, #11475, #39428, #7784, #7331, #21629, #4091, #25555, #28570, #24864, #42418, #18187, #35712, #39202, #14723, #29022, #22299, #21862, #28797, #35952, #42659, #32262, #839, #620, #25316, #7553, #18629, #36396, #18410, #159, #4758, #38981, #18862, #11705, #10789, #11022, #14938, #21407, #35482, #39669, #4318, #4536, #36176, #14250, #8017, #3856, #42875, #17947, #28318, #11242, #32489, #8230, #43106, #25777, #22086, #32017, #389, #32716, #25088, #15171, #14491, #1062, #29260, #39888, #43337, #22759, #8904, #2195, #32952, #29919, #40094, #36854, #8455, #5205, #40556, #19083, #26228, #37302, #33173, #30146, #43765, #1510, #23193, #15605, #33612, #22971, #11915, #44004, #44236, #5420, #19293, #1723, #15396, #33378, #29477, #37067, #8694, #40768, #33841, #26455, #41005, #22526, #15827, #12145, #12378, #19513, #29689, #26671, #40342, #12817, #43549, #25986, #9365, #12594, #1964, #16063, #36636, #16287, #23433, #4991, #9126, #5663, #19755, #30368, #44460, #37534, #26897, #5893, #1298, #37764, #27364, #13515, #10266, #45386, #6352, #20203, #9593, #6113, #10048, #44699, #6798, #44929, #24343, #45624, #3347, #24564, #38228, #2418, #6574, #34058, #13060, #27147, #30599, #38447, #42138, #41459, #16518, #20876, #41234, #34528, #13971, #17440, #20653, #23653, #10489, #28044, #41922, #13749, #34283, #16978, #31521, #34973, #45153, #2656, #9812, #16754, #31283, #17195, #38680, #30835, #27588, #19982, #23879, #13287, #37999, #27827, #34745, #20436, #2886, #31054, #41692, #24117, #3105, #42360, #28261, #35426, #7279, #788, #100, #10728, #4268, #11647, #18359, #14667, #39366, #14429, #3584, #565, #28509, #1004, #21800, #22032, #28743, #42824, #32661, #38928, #7720, #25724, #24807, #42607, #4486, #326, #7038, #14192, #14888, #43276, #21349, #21124, #15108, #39608, #35208, #17671, #11185, #35893, #29196, #10967, #3797, #31732, #25036, #17888, #31956, #39146, #32202, #7497, #21568, #43048, #35652, #4023, #18124, #11409, #25256, #32440, #28966, #36121, #25496, #7965, #18578, #19692, #16008, #33550, #1236, #36796, #37235, #9063, #19237, #32891, #1455, #8179, #5362, #37008, #16224, #15342, #1668, #30090, #29635, #11862, #44172, #1899, #26397, #26609, #40709, #43495, #18801, #40042, #25935, #29423, #8399, #22467, #36575, #12535, #4930, #19027, #19457, #44396, #23131, #15773, #40498, #15555, #36341, #33324, #43714, #33784, #8849, #5600, #29860, #43945, #2135, #33119, #22917, #12751, #12090, #26168, #30302, #40281, #39837, #8635, #22244, #4700, #22698, #5153, #12323, #13681, #40938, #9303, #16919, #41623, #3279, #20139, #19923, #26831, #34216, #17373, #6739, #2591, #6284, #16450, #23372, #10207, #34913, #30534, #20371, #31223, #16692, #38169, #37701, #31457, #41862, #34691, #30778, #44633, #44869, #34466, #45320, #6518, #13231, #27084, #12997, #41177, #30999, #5837, #27760, #6050, #38390, #20814, #45559, #37476, #45096, #33998, #13454, #2351, #9531, #23595, #9752, #2827, #27308, #41402, #27523, #23816, #9980, #37927, #24050, #20596, #3049, #13912, #18523, #38614, #36070, #25434, #24506, #10665, #14613, #21059, #10429, #7662, #3966, #18306, #4213, #27985, #39307, #6974, #7218, #35143, #32604, #21290, #35367, #21981, #42545, #39556, #7437, #3520, #17605, #35590, #24748, #28908, #31674, #28686, #42, #7911, #18061, #3742, #32142, #42989, #42080, #10909, #14135, #17830, #28207, #31898, #21510, #42301, #270, #32384, #38864, #11125, #14367, #28447, #736, #24977, #42764, #506, #39088, #25194, #21740, #35837, #14835, #11353, #4435, #18977, #29137, #22645, #22410, #8800, #1845, #40222, #9012, #8133, #33068, #25883, #1407, #19190, #1181, #40446, #43447, #26561, #43220, #11593, #23083, #12266, #36514, #12038, #8344, #946, #43667, #15510, #12483, #5313, #40659, #37181, #29590, #22868, #5544, #19638, #15953, #26343, #8581, #36743, #22195, #4875, #26106, #36960, #29375, #25671, #39784, #5102, #33276, #39995, #1622, #29807, #15049, #15721, #19409, #43887, #33496, #36288, #30036, #44118, #4647, #11814, #18742, #32831, #15291, #23544, #27030, #2535, #16872, #10160, #41351, #16640, #9701, #16400, #37647, #34411, #5996, #13180, #41129, #6473, #24236, #6226, #33732, #38345, #12702, #6690, #45267, #44346, #30480, #2780, #40887, #30254, #27475, #23765, #38120, #23998, #2081, #13403, #26782, #9481, #9254, #16173, #20089, #34164, #41814, #30728, #13626, #27261, #23322, #37426, #37878, #44583, #3003, #5783, #30954, #19872, #27710, #20318, #44822, #45048, #17091, #33950, #41573, #2301, #9925, #12944, #20549, #34646, #31170, #36733, #2070, #29580, #40650, #8569, #43656, #33721, #12027, #44109, #33486, #22397, #40438, #9003, #15940, #15712, #12254, #25873, #29797, #39985, #19400, #33267, #5530, #44336, #36951, #5770, #4864, #43875, #22635, #26334, #30024, #26094, #37172, #40207, #23311, #8333, #36500, #19858, #23073, #1613, #8790, #5091, #43436, #22858, #5304, #9240, #16162, #37414, #33938, #1832, #19627, #2290, #16388, #12691, #12473, #30244, #26552, #26771, #40877, #11804, #18965, #33059, #1396, #15500, #41802, #2992, #2769, #45036, #12930, #16862, #27017, #6463, #6214 ),
 ( #34847, #10371, #42025, #13391, #38334, #24447, #3453, #45496, #10151, #23986, #38107, #37633, #20306, #34398, #24226, #13167, #9469, #41116, #30942, #27463, #23752, #41561, #13615, #6906, #20541, #9915, #34635, #27247, #17080, #31157, #45255, #27698, #37867, #3211, #20985, #6680, #30467, #35080, #23531, #44570, #38551, #5984, #41338, #20756, #20076, #34151, #17302, #31391, #13853, #27930, #2522, #16627, #30714, #44810, #9688, #22136, #10842, #39028, #25613, #443, #29077, #11069, #7152, #14078, #39250, #14304, #32541, #10603, #32319, #38796, #11530, #21680, #7378, #7602, #888, #17549, #14546, #24679, #21454, #21230, #35531, #25136, #3687, #24915, #21921, #28153, #7845, #39724, #3906, #40078, #36009, #42245, #32072, #43164, #14990, #35771, #35310, #8073, #36224, #39486, #11292, #17774, #28624, #31622, #31840, #42705, #210, #18001, #28375, #28846, #14775, #42477, #4149, #18244, #4372, #673, #42926, #18461, #25371, #36902, #37116, #5475, #8282, #29317, #4813, #22347, #39939, #25826, #33011, #18916, #44056, #43392, #36450, #1774, #9181, #15885, #12201, #5255, #11970, #1116, #43815, #26037, #44287, #19346, #19571, #26280, #40392, #30197, #1351, #33430, #23256, #15454, #40150, #2016, #43604, #4588, #11759, #12424, #40824, #29529, #18679, #12643, #33667, #32770, #15230, #8743, #29972, #26723, #8514, #22581, #36683, #5043, #19134, #33222, #1560, #29736, #15659, #22810, #16112, #26503, #40604, #8955, #23024, #44757, #2938, #2470, #45443, #6629, #45201, #27194, #9414, #13115, #30888, #27639, #17025, #23703, #37583, #26958, #23482, #27414, #16337, #24175, #16577, #41747, #17249, #20703, #41980, #9861, #19806, #23933, #5718, #30418, #44515, #34795, #13563, #41287, #5937, #9639, #44982, #10100, #31102, #37815, #20027, #41057, #34104, #41511, #12875, #38283, #30659, #3158, #31336, #13804, #10321, #38052, #33889, #6410, #2242, #6164, #20254, #34345, #27882, #37357, #2714, #16808, #13337, #20492, #34580, #4316, #7782, #42657, #20928, #14936, #18408, #618, #18185, #31574, #21405, #21859, #39426, #3854, #17496, #31787, #38496, #35710, #21627, #837, #45676, #32014, #14721, #14247, #42192, #28795, #32260, #11020, #11240, #25314, #28097, #3402, #24617, #10541, #14028, #38738, #7098, #21178, #42873, #35258, #3637, #4088, #29020, #35950, #387, #25086, #157, #35026, #17945, #28316, #32487, #39200, #43104, #14489, #28568, #24393, #17724, #7551, #6848, #42416, #10787, #24862, #38979, #7329, #35480, #5203, #1962, #25775, #16061, #37064, #44002, #25553, #39666, #1506, #26226, #33610, #4756, #4534, #11473, #18860, #30144, #5418, #32950, #36634, #1060, #8015, #40554, #19511, #15169, #4989, #15825, #1296, #22757, #22297, #22084, #18627, #40340, #32714, #36174, #15603, #15394, #33171, #26453, #29258, #8453, #43335, #29474, #11702, #43547, #19081, #39886, #11913, #29917, #8228, #8692, #36394, #25984, #1721, #40092, #12143, #29687, #22524, #43763, #36852, #19290, #33376, #12376, #8902, #22969, #26669, #20201, #19980, #6350, #45151, #37762, #6572, #5661, #30597, #23431, #44697, #16752, #44458, #37997, #41003, #24115, #40766, #9124, #20651, #9810, #34056, #9591, #5891, #44234, #41232, #13058, #10046, #2884, #38226, #34743, #27145, #20434, #3103, #17193, #13513, #23877, #6111, #34281, #19753, #2416, #16516, #34526, #26895, #23191, #37300, #23651, #2654, #37532, #30833, #27362, #12592, #44927, #13285, #41457, #9363, #16976, #31052, #27586, #41690, #33839, #2193, #16285, #30366, #12815, #35891, #10264, #7718, #42822, #41920, #28042, #31954, #38445, #27825, #25034, #21347, #35650, #21566, #31281, #10965, #24341, #24562, #6796, #4266, #38678, #7036, #39364, #14190, #11183, #24805, #20874, #34971, #7277, #42136, #563, #21122, #45384, #42605, #28507, #21798, #3345, #38926, #7495, #35206, #17438, #4021, #39144, #17886, #18122, #32200, #31519, #45622, #13969, #10487, #3582, #17669, #31730, #98, #14665, #28259, #42358, #28741, #13747, #25254, #35424, #324, #10726, #3795, #14427, #39834, #12321, #33117, #33323, #40040, #25933, #43944, #4484, #4928, #22916, #36119, #8177, #15772, #11645, #37006, #25494, #12089, #8848, #32659, #18357, #26396, #5152, #32438, #786, #8397, #1453, #40497, #25722, #11407, #14886, #22242, #28964, #43046, #36339, #43493, #7963, #39606, #1667, #22030, #18576, #11860, #22697, #4698, #29634, #29194, #1002, #29859, #26167, #18799, #15106, #32889, #22465, #8634, #43713, #1233, #43274, #15340, #29421, #36573, #19025, #19236, #15554, #36795, #40280, #34464, #9978, #23593, #33549, #37698, #19456, #44171, #30088, #16007, #41400, #27520, #26830, #1898, #9749, #12534, #19920, #30996, #2825, #6048, #26608, #41621, #45094, #27306, #44867, #40708, #2349, #16917, #20369, #30532, #9062, #13229, #6283, #44631, #13452, #23130, #37474, #30301, #5835, #20137, #5599, #23814, #2133, #24048, #37234, #19691, #5361, #16690, #40937, #16448, #12750, #33783, #12995, #33996, #16223, #37925, #44395, #9302, #27082, #23370, #41175, #9529, #34214, #30776, #2589, #40, #45317, #13910, #42078, #3740, #20812, #17138, #34689, #10427, #27983, #31455, #6972, #21288, #14611, #14133, #21057, #28205, #34911, #24504, #38863, #38612, #17603, #45557, #10907, #28684, #10663, #38167, #42761, #31221, #11123, #3964, #3047, #3277, #7215, #13679, #27758, #31896, #42299, #42543, #28445, #6516, #17828, #41860, #35140, #10205, #20594, #3518, #31672, #504, #24746, #18059, #35365, #24282, #38388, #268, #17370, #7435, #6737, #14365, #24974, #32140, #39086, #21508, #35588, #40219, #25192, #22193, #32382, #29135, #734, #15047, #32829, #11351, #18521, #29588, #25432, #22406, #36067, #39554, #15508, #7909, #25880, #15289, #4211, #36286, #36512, #43445, #43218, #39782, #7660, #11591, #21738, #1179, #944, #32601, #39305, #4873, #18975, #2248, #18303, #29373, #1405, #25669, #42987, #43664, #33066, #11812, #12036, #26104, #28906, #14832, #21979, #4433, #8130, #4643, #18740, #39993, #9187, #8341, #23262, #37363, #30423, #5724, #19811, #33894, #16343, #35835, #44522, #34352, #6855, #27645, #27887, #34588, #20498, #38503, #44764, #45207, #17502, #30667, #2721, #10327, #6171, #31580, #20033, #6636, #3409, #27201, #12880, #20937, #45450, #26966, #41062, #2944, #41756, #35032, #20260, #5942, #9420, #16816, #23488, #37588, #30894, #38060, #2477, #34110, #41985, #16584, #13121, #6416, #17256, #44989, #24182, #23710, #41295, #24401, #20709, #13345, #9645, #27420, #17033, #3165, #38289, #41517, #37821, #9869, #23939, #31111, #13570, #13810, #10106, #31342, #34803, #29027, #4541, #18193, #28104, #32268, #14036, #38747, #24627, #10548, #35957, #22091, #21412, #42201, #4324, #7106, #14499, #25561, #43114, #626, #21186, #36181, #39675, #21869, #39437, #35265, #42664, #11482, #14944, #25093, #3644, #14728, #17731, #8022, #4097, #35488, #21635, #18635, #45683, #11027, #31795 ),
 ( #35719, #3863, #7790, #844, #39207, #165, #14256, #32024, #24869, #394, #28802, #28324, #18415, #42424, #10796, #38986, #7336, #17952, #11248, #28576, #7559, #42880, #25322, #32494, #19090, #44240, #37072, #12599, #26677, #15610, #40561, #40772, #5668, #1969, #44009, #26234, #40347, #39893, #8462, #36642, #12382, #15401, #11710, #29266, #4997, #22532, #25991, #1515, #15832, #9130, #8699, #29694, #22764, #29483, #33178, #33383, #43770, #12151, #40099, #5424, #23197, #5209, #32721, #37306, #25782, #1069, #15177, #43342, #43554, #1727, #8235, #22304, #26459, #36859, #19519, #22975, #36401, #8909, #4764, #19298, #18867, #32959, #29924, #33617, #1305, #16067, #11920, #30150, #9370, #16291, #41463, #16524, #34749, #12821, #6359, #33845, #26902, #44466, #30373, #10054, #41928, #41239, #2199, #24124, #41009, #34291, #45391, #3110, #38005, #23437, #10270, #13753, #41698, #13519, #37538, #16759, #17199, #31287, #44933, #5897, #27151, #19986, #31059, #16982, #24347, #34062, #27368, #38232, #9597, #2423, #6579, #27592, #20441, #20657, #27833, #30605, #44704, #13065, #23657, #37768, #6117, #20208, #2661, #38451, #30839, #13292, #45157, #19759, #9816, #23883, #34532, #2890, #3353, #7283, #17676, #42828, #14433, #32208, #35431, #21353, #28747, #10494, #331, #39371, #42143, #31737, #570, #3588, #7725, #45629, #25040, #6802, #7044, #20880, #11189, #14671, #17445, #31526, #31960, #42611, #34977, #42365, #38686, #13977, #24812, #28048, #24568, #28515, #21574, #10733, #104, #21129, #35213, #3802, #25262, #14198, #39150, #28265, #7502, #38932, #17893, #10971, #35656, #4030, #18129, #41605, #38373, #27742, #34449, #2571, #37686, #20125, #38152, #27071, #34893, #27293, #6721, #27967, #31436, #6952, #20580, #30516, #21036, #34201, #23800, #45542, #41387, #2335, #9515, #41845, #38595, #16677, #16435, #42063, #3259, #44618, #12983, #6501, #17121, #24488, #9735, #41164, #23581, #37912, #6033, #10412, #6266, #27507, #30763, #44854, #13893, #13216, #20353, #9962, #20796, #2812, #13660, #16903, #30984, #17351, #10189, #45081, #13437, #24032, #34676, #3033, #24265, #31206, #45302, #24724, #7198, #25176, #14117, #21965, #14347, #39533, #15030, #18505, #39766, #7642, #17587, #21721, #3501, #28190, #42283, #25, #25413, #11572, #10889, #31658, #7890, #10645, #3946, #29118, #32584, #35814, #38845, #25653, #43201, #11334, #28887, #21269, #32121, #926, #4413, #14593, #35348, #42523, #3724, #716, #32360, #8114, #17812, #42744, #36051, #24956, #31878, #35123, #42967, #4193, #250, #28424, #39070, #7418, #21492, #35569, #18041, #486, #28666, #11106, #39287, #18286, #14814, #19390, #26762, #33477, #29787, #8782, #29572, #18722, #15702, #43648, #16154, #36943, #37163, #43866, #12246, #2062, #8324, #22850, #30236, #5296, #5521, #26325, #40430, #44328, #22388, #1823, #40868, #39975, #12017, #19617, #15492, #22174, #29356, #15931, #12683, #36492, #36269, #4625, #8995, #32809, #1162, #30015, #44101, #15270, #26085, #43428, #11796, #40199, #25865, #4855, #8560, #1605, #18955, #33051, #33713, #1388, #22624, #12465, #26544, #36725, #40642, #5083, #19174, #33259, #23063, #44802, #27008, #16619, #2760, #45246, #34627, #41331, #9460, #44561, #41107, #45028, #33930, #41793, #34142, #13606, #34839, #38326, #13845, #27455, #37405, #41552, #23303, #2281, #16380, #19849, #27689, #31384, #30706, #5762, #10143, #30457, #23744, #3203, #6672, #9905, #12922, #45488, #17294, #31149, #2984, #23523, #6205, #20747, #24218, #34389, #37625, #13159, #5976, #20533, #6454, #27923, #20067, #16854, #9231, #27238, #2513, #9680, #17071, #23978, #37856, #20298, #30934, #13382, #38099, #45718, #31615, #17541, #24670, #42238, #35763, #35073, #14071, #39242, #881, #7595, #3899, #28616, #3680, #38544, #35523, #17767, #42469, #14538, #10594, #4142, #38788, #21914, #24439, #6896, #18456, #21671, #31832, #7371, #203, #42018, #39021, #28367, #7839, #666, #36001, #4365, #24907, #18235, #32535, #14984, #11285, #32310, #17992, #32064, #3445, #14294, #10835, #14767, #7144, #20976, #28144, #21447, #436, #35303, #42698, #25129, #10364, #11062, #28839, #42919, #21222, #25362, #39479, #18910, #8507, #22340, #1767, #5469, #1554, #29069, #33661, #8067, #19564, #40599, #39717, #25819, #29732, #36218, #25607, #22804, #19130, #33425, #19340, #43157, #8738, #22129, #36441, #4582, #2010, #4805, #33003, #37111, #11963, #8948, #22576, #18673, #32762, #5038, #39931, #44050, #1109, #43811, #15224, #23018, #33218, #1342, #15652, #12418, #11524, #26032, #29311, #15447, #43385, #29523, #36678, #11752, #43597, #15878, #8275, #26275, #40143, #12195, #29967, #40387, #36897, #5251, #26499, #13109, #27408, #34338, #34098, #30654, #44281, #2465, #12638, #37810, #37576, #23926, #17021, #9634, #24170, #23248, #16569, #41051, #37351, #26717, #9856, #6159, #20488, #6405, #16107, #41505, #40818, #9408, #5712, #20699, #23476, #5931, #38279, #44751, #27632, #23698, #19799, #9171, #20247, #12868, #31098, #33883, #30881, #2236, #10095, #2709, #20022, #16802, #45197, #30191, #27190, #16331, #41281, #30413, #44977, #13331, #44508, #38047, #34574, #26951, #2934, #13559, #41742, #6624, #34790, #3848, #38974, #27877, #152, #14483, #21400, #21173, #17718, #31330, #35253, #45438, #24857, #24612, #11014, #4079, #42408, #11235, #10317, #3631, #28092, #31781, #35474, #3398, #42652, #45670, #28790, #13800, #41974, #25308, #28562, #38729, #14241, #10536, #3153, #28310, #10780, #14714, #7545, #42868, #39420, #7324, #25081, #7774, #21852, #18179, #39195, #17940, #32008, #24388, #7092, #379, #21621, #31570, #38492, #6844, #35705, #32255, #42186, #613, #17244, #20924, #35020, #17492, #14022, #18622, #39882, #36629, #25770, #29468, #29253, #8687, #12371, #8448, #35944, #40546, #14932, #26447, #1715, #833, #32709, #4983, #43331, #11464, #8896, #11697, #8223, #43995, #18854, #15819, #43541, #25548, #32483, #11908, #1055, #5198, #29015, #19076, #39661, #29909, #40087, #22292, #25979, #19283, #4311, #32945, #43098, #36388, #22078, #4750, #22518, #36169, #1290, #40335, #4530, #33165, #15161, #1501, #26219, #15599, #29681, #43759, #12137, #22751, #36846, #33370, #18403, #37525, #5409, #40994, #19505, #44689, #44449, #30826, #23869, #16507, #31045, #30137, #9355, #2186, #23424, #41226, #23184, #16744, #19746, #2877, #33602, #1954, #45144, #34273, #12806, #34049, #30357, #22963, #19973, #5884, #34518, #27355, #16968, #13503, #2406, #44920, #27577, #42292, #37986, #2647, #30588, #13048, #44225, #26887, #27137, #13278, #5653, #16055, #12583, #9583, #23643, #16278, #37754, #6103, #37057, #20193, #41450, #9801, #33833, #6341, #20425, #26660, #40757, #9115, #37292, #32819, #28897, #10654, #15280, #35358, #1171, #22185, #21279, #7427, #11344, #17820, #7206, #4425, #725, #15040, #936, #24736, #36060, #3732, #35825 ),
 ( #3956, #32131, #18733, #39296, #36278, #4203, #259, #31888, #32372, #21500, #25662, #14355, #25422, #28435, #4635, #14823, #496, #42978, #39775, #38854, #7651, #42533, #14602, #10897, #28674, #18295, #24965, #18049, #29126, #39079, #7901, #35578, #42753, #43211, #11115, #39544, #21974, #25184, #21730, #18513, #32593, #11583, #8123, #29366, #25570, #35727, #29274, #29035, #15412, #8471, #1076, #15620, #14735, #39683, #32502, #8031, #25789, #7801, #1312, #4333, #33187, #4105, #18200, #29704, #18876, #43121, #18641, #14951, #7565, #4548, #22098, #19098, #11929, #1523, #43779, #36188, #29490, #12160, #26244, #22541, #32967, #15188, #43351, #28809, #11490, #32729, #43562, #35966, #32276, #633, #11717, #39903, #851, #8242, #36410, #21641, #22311, #4771, #25998, #18422, #40108, #36649, #5007, #42888, #11255, #25330, #39445, #21876, #44714, #20216, #6126, #23207, #2432, #34300, #13301, #9604, #5904, #33854, #2208, #1738, #16075, #44250, #19993, #22986, #19307, #36868, #12610, #30159, #33627, #9139, #23445, #16768, #16299, #37319, #30382, #37080, #26686, #41019, #40783, #19768, #1978, #13075, #30849, #12831, #40355, #44945, #33393, #8707, #2673, #5219, #5434, #9379, #15842, #29934, #34070, #44474, #27160, #30617, #22774, #16534, #44017, #5677, #12390, #26469, #26910, #37546, #40570, #41248, #8917, #23665, #19528, #37777, #3362, #24132, #42373, #20452, #42151, #2900, #21366, #31537, #17208, #17454, #10742, #27377, #24355, #34540, #31295, #16991, #45400, #34986, #13527, #20666, #31745, #27600, #24577, #38243, #41708, #17686, #10064, #28058, #45638, #6370, #38459, #38695, #13986, #13765, #41936, #9825, #27842, #23894, #10502, #3118, #35221, #28274, #20889, #35442, #31067, #10281, #6588, #6810, #7054, #34757, #21138, #3599, #7291, #38015, #45165, #3811, #116, #14206, #24821, #38941, #17903, #31970, #341, #41472, #36527, #23093, #43678, #26571, #8592, #4040, #10981, #36756, #11201, #30047, #7512, #29820, #35666, #9023, #19200, #4886, #5111, #44129, #14445, #12049, #21583, #18988, #18139, #33080, #22658, #579, #7736, #19419, #14680, #12279, #25273, #28757, #5324, #42837, #15731, #33287, #39162, #26121, #26354, #1632, #1417, #29600, #42620, #15520, #25050, #43901, #40235, #22879, #15966, #40458, #37193, #32218, #8811, #39383, #36971, #33511, #21815, #1858, #12494, #40668, #5559, #19651, #33745, #28525, #23557, #13194, #9494, #2095, #44833, #34176, #13639, #6484, #27722, #41826, #30739, #9940, #10171, #20780, #17104, #13417, #41366, #9713, #9265, #37659, #6008, #27487, #30491, #26793, #44357, #20101, #2548, #41141, #16653, #30966, #24249, #23777, #27274, #37890, #44596, #6242, #2792, #20330, #34425, #16884, #20564, #38357, #45061, #16184, #6703, #40898, #30265, #12713, #23333, #12956, #41584, #37437, #5797, #24011, #38133, #34658, #3018, #19883, #31186, #45280, #33960, #2312, #16411, #27043, #34874, #42265, #11314, #14792, #10625, #14325, #24469, #17327, #18267, #42946, #38576, #28402, #39266, #24702, #465, #8, #25391, #4172, #42723, #38822, #6930, #7176, #42500, #25156, #14569, #21249, #35101, #21013, #3478, #24934, #13874, #21698, #14098, #7622, #28865, #32340, #39511, #7398, #31414, #21472, #3237, #27950, #42046, #45521, #35794, #7867, #35329, #10393, #696, #17568, #3707, #31640, #28172, #35550, #17793, #31859, #230, #11086, #28645, #10868, #39049, #3926, #18021, #32098, #15010, #29338, #36031, #33239, #19153, #44078, #29097, #29551, #43838, #11777, #39745, #26300, #15680, #8535, #8761, #22828, #25634, #906, #22156, #8095, #11552, #43183, #4604, #36245, #29761, #18699, #32789, #1580, #26524, #12222, #43626, #22600, #43410, #18485, #15473, #25848, #15906, #36703, #36922, #11994, #26060, #1797, #1140, #5061, #40623, #15249, #39957, #19369, #8303, #21945, #22367, #40411, #12444, #36471, #4394, #29991, #5276, #32562, #4833, #18936, #33453, #33031, #1369, #40171, #33689, #5957, #20276, #27216, #26984, #23502, #37140, #41083, #5498, #30683, #30438, #16832, #9883, #2492, #17046, #16131, #9437, #33909, #37604, #41310, #9205, #2738, #5739, #34602, #19592, #2038, #31125, #34368, #44539, #20046, #16358, #8974, #34125, #16599, #20513, #13359, #2959, #45222, #44782, #30910, #13584, #27664, #23954, #45004, #13138, #9660, #30218, #12898, #23724, #27433, #37381, #44308, #12662, #37837, #6186, #2261, #41531, #38075, #23042, #6434, #26742, #40844, #19826, #23280, #42439, #31593, #21198, #35047, #14512, #18206, #14269, #41771, #638, #20724, #32283, #7571, #6650, #38518, #10808, #3179, #38303, #35500, #31808, #408, #32037, #10120, #21424, #34817, #3422, #17269, #14740, #17517, #45696, #4113, #24642, #21648, #35278, #31357, #45463, #17744, #6870, #11038, #13823, #24883, #27901, #35734, #176, #14049, #28337, #25104, #24196, #38761, #41997, #28119, #10340, #42214, #3656, #24414, #10565, #28590, #20950, #38997, #7118, #7347, #3874, #17967, #42675, #39219, #7807, #39451, #19106, #5226, #4558, #11260, #33193, #25336, #43360, #8715, #12167, #1318, #21884, #19316, #22781, #5015, #22550, #35974, #25794, #26250, #43786, #8250, #4339, #36194, #42894, #40115, #26005, #33399, #18429, #36417, #1529, #18648, #858, #15625, #36654, #15420, #29709, #40362, #32509, #14958, #29044, #43129, #11497, #25577, #39692, #8039, #36876, #22105, #32738, #8479, #1745, #28814, #4779, #29497, #1083, #15197, #22316, #29282, #11725, #43569, #39909, #18882, #32975, #11938, #1985, #2440, #20461, #33633, #37326, #13309, #9148, #34549, #22993, #9613, #6380, #30167, #15849, #41481, #2682, #29940, #44023, #5910, #30626, #38024, #23217, #8923, #12396, #5686, #26475, #9834, #19777, #41025, #5442, #40577, #44953, #23903, #19537, #9385, #20225, #33861, #27169, #26694, #37086, #30858, #23674, #2214, #16083, #16307, #23452, #6134, #41257, #30390, #44257, #12616, #40790, #20000, #44482, #16778, #12839, #34312, #26920, #27386, #37552, #34077, #16543, #44722, #13085, #37786, #38704, #27609, #45648, #14215, #21147, #20898, #17463, #31075, #34996, #45174, #24587, #24364, #10753, #3822, #42159, #10991, #10072, #3372, #27851, #31545, #35229, #3128, #42384, #45411, #28534, #13534, #41716, #25059, #28284, #38467, #13997, #10289, #2908, #28065, #10511, #14456, #7300, #42629, #39171, #7064, #24830, #7521, #21595, #17912, #38950, #3608, #17695, #24143, #6820, #31756, #21375, #31304, #38252, #6597, #125, #35451, #41948, #31980, #351, #16999, #20675, #34766, #17217, #13773, #39632, #36364, #25519, #15134, #28989, #8422, #12111, #8200, #35675, #40306, #14690, #26191, #1474, #588, #32459, #4725, #42845, #32228, #29444, #25746, #40062, #25955, #4051, #15364, #28766, #43070, #11209, #8658, #11435, #7987, #43733, #18598, #15574, #29225, #25281, #39392, #11669, #807, #4956, #7745, #18828, #21822, #29656, #39859, #22054, #22267, #19048, #18149, #32684, #35916, #36144 ) ),
 .UNSPECIFIED., .T., .F., .T. ) 
 B_SPLINE_SURFACE_WITH_KNOTS ( ( 4, 3, 4 ),
 ( 3, 2, 2, 2, 2, 2, 2, 2, 2, 2, 2, 2, 2, 2, 2, 2, 2, 2, 2, 2, 2, 2, 2, 2, 2, 2, 2, 2, 2, 2, 2, 2, 2, 2, 2, 2, 2, 2, 2, 2, 2, 2, 2, 2, 2, 2, 2, 2, 2, 2, 2, 2, 2, 2, 2, 2, 2, 2, 2, 2, 2, 2, 2, 2, 2, 2, 2, 2, 2, 2, 2, 2, 2, 2, 2, 2, 2, 2, 2, 2, 2, 2, 2, 2, 2, 2, 2, 2, 2, 2, 2, 2, 2, 2, 2, 2, 2, 2, 2, 2, 2, 2, 2, 2, 2, 2, 2, 2, 2, 2, 2, 2, 2, 2, 2, 2, 2, 2, 2, 2, 2, 2, 2, 2, 2, 2, 2, 2, 2, 2, 2, 2, 2, 2, 2, 2, 2, 2, 2, 2, 2, 2, 2, 2, 2, 2, 2, 2, 2, 2, 2, 2, 2, 2, 2, 2, 2, 2, 2, 2, 2, 2, 2, 2, 2, 2, 2, 2, 2, 2, 2, 2, 2, 2, 2, 2, 2, 2, 2, 2, 2, 2, 2, 2, 2, 2, 2, 2, 2, 2, 2, 2, 2, 2, 2, 2, 2, 2, 2, 2, 2, 2, 2, 2, 2, 2, 2, 2, 2, 2, 2, 2, 2, 2, 2, 2, 2, 2, 2, 2, 2, 2, 2, 2, 2, 2, 2, 2, 2, 2, 2, 2, 2, 2, 2, 2, 2, 2, 2, 2, 2, 2, 2, 2, 2, 2, 2, 2, 2, 2, 2, 2, 2, 2, 2, 2, 2, 2, 2, 2, 2, 2, 2, 2, 2, 2, 2, 2, 2, 2, 2, 2, 2, 2, 2, 2, 2, 2, 2, 2, 2, 2, 2, 2, 2, 2, 2, 2, 2, 2, 2, 2, 2, 2, 2, 2, 2, 2, 2, 2, 2, 2, 2, 2, 2, 2, 2, 2, 2, 2, 2, 2, 2, 2, 2, 2, 2, 2, 2, 2, 2, 2, 2, 2, 2, 2, 2, 2, 2, 2, 2, 2, 2, 2, 2, 2, 2, 2, 2, 2, 2, 2, 2, 2, 2, 2, 2, 2, 2, 2, 2, 2, 2, 2, 2, 2, 2, 2, 2, 2, 2, 2, 2, 2, 2, 2, 2, 2, 2, 2, 2, 2, 2, 2, 2, 2, 2, 2, 2, 2, 2, 2, 2, 2, 2, 2, 2, 2, 2, 2, 2, 2, 2, 2, 2, 2, 2, 2, 2, 2, 2, 2, 2, 2, 2, 2, 2, 2, 2, 2, 2, 2, 2, 2, 2, 2, 2, 2, 2, 2, 2, 2, 2, 2, 2, 2, 2, 2, 2, 2, 2, 3 ),
 ( 0.000000000000000000, 0.5000000000000000000, 1.000000000000000000 ),
 ( 0.000000000000000000, 0.002272727272727272617, 0.004545454545454545234, 0.006818181818181817851, 0.009090909090909090468, 0.01136363636363636395, 0.01363636363636363570, 0.01590909090909090745, 0.01818181818181818094, 0.02045454545454545442, 0.02272727272727272790, 0.02500000000000000139, 0.02727272727272727140, 0.02954545454545454489, 0.03181818181818181490, 0.03409090909090908839, 0.03636363636363636187, 0.03863636363636363535, 0.04090909090909090884, 0.04318181818181818232, 0.04545454545454545581, 0.04772727272727272929, 0.05000000000000000278, 0.05227272727272726932, 0.05454545454545454281, 0.05681818181818181629, 0.05909090909090908977, 0.06136363636363636326, 0.06363636363636362980, 0.06590909090909090329, 0.06818181818181817677, 0.07045454545454545026, 0.07272727272727272374, 0.07499999999999999722, 0.07727272727272727071, 0.07954545454545454419, 0.08181818181818181768, 0.08409090909090909116, 0.08636363636363636465, 0.08863636363636363813, 0.09090909090909091161, 0.09318181818181818510, 0.09545454545454545858, 0.09772727272727273207, 0.1000000000000000056, 0.1022727272727272790, 0.1045454545454545386, 0.1068181818181818121, 0.1090909090909090856, 0.1113636363636363591, 0.1136363636363636326, 0.1159090909090909061, 0.1181818181818181795, 0.1204545454545454530, 0.1227272727272727265, 0.1250000000000000000, 0.1272727272727272596, 0.1295454545454545470, 0.1318181818181818066, 0.1340909090909090939, 0.1363636363636363535, 0.1386363636363636409, 0.1409090909090909005, 0.1431818181818181879, 0.1454545454545454475, 0.1477272727272727348, 0.1499999999999999944, 0.1522727272727272818, 0.1545454545454545414, 0.1568181818181818288, 0.1590909090909090884, 0.1613636363636363757, 0.1636363636363636354, 0.1659090909090909227, 0.1681818181818181823, 0.1704545454545454419, 0.1727272727272727293, 0.1749999999999999889, 0.1772727272727272763, 0.1795454545454545359, 0.1818181818181818232, 0.1840909090909090828, 0.1863636363636363702, 0.1886363636363636298, 0.1909090909090909172, 0.1931818181818181768, 0.1954545454545454641, 0.1977272727272727237, 0.2000000000000000111, 0.2022727272727272707, 0.2045454545454545581, 0.2068181818181818177, 0.2090909090909090773, 0.2113636363636363646, 0.2136363636363636243, 0.2159090909090909116, 0.2181818181818181712, 0.2204545454545454586, 0.2227272727272727182, 0.2250000000000000056, 0.2272727272727272652, 0.2295454545454545525, 0.2318181818181818121, 0.2340909090909090995, 0.2363636363636363591, 0.2386363636363636465, 0.2409090909090909061, 0.2431818181818181934, 0.2454545454545454530, 0.2477272727272727404, 0.2500000000000000000, 0.2522727272727272596, 0.2545454545454545192, 0.2568181818181818343, 0.2590909090909090939, 0.2613636363636363535, 0.2636363636363636131, 0.2659090909090909283, 0.2681818181818181879, 0.2704545454545454475, 0.2727272727272727071, 0.2750000000000000222, 0.2772727272727272818, 0.2795454545454545414, 0.2818181818181818010, 0.2840909090909091161, 0.2863636363636363757, 0.2886363636363636354, 0.2909090909090908950, 0.2931818181818181546, 0.2954545454545454697, 0.2977272727272727293, 0.2999999999999999889, 0.3022727272727272485, 0.3045454545454545636, 0.3068181818181818232, 0.3090909090909090828, 0.3113636363636363424, 0.3136363636363636576, 0.3159090909090909172, 0.3181818181818181768, 0.3204545454545454364, 0.3227272727272727515, 0.3250000000000000111, 0.3272727272727272707, 0.3295454545454545303, 0.3318181818181818454, 0.3340909090909091050, 0.3363636363636363646, 0.3386363636363636243, 0.3409090909090908839, 0.3431818181818181990, 0.3454545454545454586, 0.3477272727272727182, 0.3499999999999999778, 0.3522727272727272929, 0.3545454545454545525, 0.3568181818181818121, 0.3590909090909090717, 0.3613636363636363869, 0.3636363636363636465, 0.3659090909090909061, 0.3681818181818181657, 0.3704545454545454808, 0.3727272727272727404, 0.3750000000000000000, 0.3772727272727272596, 0.3795454545454545192, 0.3818181818181818343, 0.3840909090909090939, 0.3863636363636363535, 0.3886363636363636131, 0.3909090909090909283, 0.3931818181818181879, 0.3954545454545454475, 0.3977272727272727071, 0.4000000000000000222, 0.4022727272727272818, 0.4045454545454545414, 0.4068181818181818010, 0.4090909090909091161, 0.4113636363636363757, 0.4136363636363636354, 0.4159090909090908950, 0.4181818181818181546, 0.4204545454545454697, 0.4227272727272727293, 0.4249999999999999889, 0.4272727272727272485, 0.4295454545454545636, 0.4318181818181818232, 0.4340909090909090828, 0.4363636363636363424, 0.4386363636363636576, 0.4409090909090909172, 0.4431818181818181768, 0.4454545454545454364, 0.4477272727272727515, 0.4500000000000000111, 0.4522727272727272707, 0.4545454545454545303, 0.4568181818181818454, 0.4590909090909091050, 0.4613636363636363646, 0.4636363636363636243, 0.4659090909090908839, 0.4681818181818181990, 0.4704545454545454586, 0.4727272727272727182, 0.4749999999999999778, 0.4772727272727272929, 0.4795454545454545525, 0.4818181818181818121, 0.4840909090909090717, 0.4863636363636363869, 0.4886363636363636465, 0.4909090909090909061, 0.4931818181818181657, 0.4954545454545454808, 0.4977272727272727404, 0.5000000000000000000, 0.5022727272727273151, 0.5045454545454545192, 0.5068181818181818343, 0.5090909090909090384, 0.5113636363636363535, 0.5136363636363636687, 0.5159090909090908728, 0.5181818181818181879, 0.5204545454545455030, 0.5227272727272727071, 0.5250000000000000222, 0.5272727272727272263, 0.5295454545454545414, 0.5318181818181818565, 0.5340909090909090606, 0.5363636363636363757, 0.5386363636363636909, 0.5409090909090908950, 0.5431818181818182101, 0.5454545454545454142, 0.5477272727272727293, 0.5500000000000000444, 0.5522727272727272485, 0.5545454545454545636, 0.5568181818181817677, 0.5590909090909090828, 0.5613636363636363980, 0.5636363636363636020, 0.5659090909090909172, 0.5681818181818182323, 0.5704545454545454364, 0.5727272727272727515, 0.5749999999999999556, 0.5772727272727272707, 0.5795454545454545858, 0.5818181818181817899, 0.5840909090909091050, 0.5863636363636363091, 0.5886363636363636243, 0.5909090909090909394, 0.5931818181818181435, 0.5954545454545454586, 0.5977272727272727737, 0.5999999999999999778, 0.6022727272727272929, 0.6045454545454544970, 0.6068181818181818121, 0.6090909090909091272, 0.6113636363636363313, 0.6136363636363636465, 0.6159090909090909616, 0.6181818181818181657, 0.6204545454545454808, 0.6227272727272726849, 0.6250000000000000000, 0.6272727272727273151, 0.6295454545454545192, 0.6318181818181818343, 0.6340909090909090384, 0.6363636363636363535, 0.6386363636363636687, 0.6409090909090908728, 0.6431818181818181879, 0.6454545454545455030, 0.6477272727272727071, 0.6500000000000000222, 0.6522727272727272263, 0.6545454545454545414, 0.6568181818181818565, 0.6590909090909090606, 0.6613636363636363757, 0.6636363636363636909, 0.6659090909090908950, 0.6681818181818182101, 0.6704545454545454142, 0.6727272727272727293, 0.6750000000000000444, 0.6772727272727272485, 0.6795454545454545636, 0.6818181818181817677, 0.6840909090909090828, 0.6863636363636363980, 0.6886363636363636020, 0.6909090909090909172, 0.6931818181818182323, 0.6954545454545454364, 0.6977272727272727515, 0.6999999999999999556, 0.7022727272727272707, 0.7045454545454545858, 0.7068181818181817899, 0.7090909090909091050, 0.7113636363636363091, 0.7136363636363636243, 0.7159090909090909394, 0.7181818181818181435, 0.7204545454545454586, 0.7227272727272727737, 0.7249999999999999778, 0.7272727272727272929, 0.7295454545454544970, 0.7318181818181818121, 0.7340909090909091272, 0.7363636363636363313, 0.7386363636363636465, 0.7409090909090909616, 0.7431818181818181657, 0.7454545454545454808, 0.7477272727272726849, 0.7500000000000000000, 0.7522727272727273151, 0.7545454545454545192, 0.7568181818181818343, 0.7590909090909090384, 0.7613636363636363535, 0.7636363636363636687, 0.7659090909090908728, 0.7681818181818181879, 0.7704545454545455030, 0.7727272727272727071, 0.7750000000000000222, 0.7772727272727272263, 0.7795454545454545414, 0.7818181818181818565, 0.7840909090909090606, 0.7863636363636363757, 0.7886363636363636909, 0.7909090909090908950, 0.7931818181818182101, 0.7954545454545454142, 0.7977272727272727293, 0.8000000000000000444, 0.8022727272727272485, 0.8045454545454545636, 0.8068181818181817677, 0.8090909090909090828, 0.8113636363636363980, 0.8136363636363636020, 0.8159090909090909172, 0.8181818181818182323, 0.8204545454545454364, 0.8227272727272727515, 0.8249999999999999556, 0.8272727272727272707, 0.8295454545454545858, 0.8318181818181817899, 0.8340909090909091050, 0.8363636363636363091, 0.8386363636363636243, 0.8409090909090909394, 0.8431818181818181435, 0.8454545454545454586, 0.8477272727272727737, 0.8499999999999999778, 0.8522727272727272929, 0.8545454545454544970, 0.8568181818181818121, 0.8590909090909091272, 0.8613636363636363313, 0.8636363636363636465, 0.8659090909090909616, 0.8681818181818181657, 0.8704545454545454808, 0.8727272727272726849, 0.8750000000000000000, 0.8772727272727273151, 0.8795454545454545192, 0.8818181818181818343, 0.8840909090909090384, 0.8863636363636363535, 0.8886363636363636687, 0.8909090909090908728, 0.8931818181818181879, 0.8954545454545455030, 0.8977272727272727071, 0.9000000000000000222, 0.9022727272727272263, 0.9045454545454545414, 0.9068181818181818565, 0.9090909090909090606, 0.9113636363636363757, 0.9136363636363636909, 0.9159090909090908950, 0.9181818181818182101, 0.9204545454545454142, 0.9227272727272727293, 0.9250000000000000444, 0.9272727272727272485, 0.9295454545454545636, 0.9318181818181817677, 0.9340909090909090828, 0.9363636363636363980, 0.9386363636363636020, 0.9409090909090909172, 0.9431818181818182323, 0.9454545454545454364, 0.9477272727272727515, 0.9499999999999999556, 0.9522727272727272707, 0.9545454545454545858, 0.9568181818181817899, 0.9590909090909091050, 0.9613636363636363091, 0.9636363636363636243, 0.9659090909090909394, 0.9681818181818181435, 0.9704545454545454586, 0.9727272727272727737, 0.9749999999999999778, 0.9772727272727272929, 0.9781254700864303597 ),
 .UNSPECIFIED. ) 
 GEOMETRIC_REPRESENTATION_ITEM ( )  RATIONAL_B_SPLINE_SURFACE ( (
 ( 1.000000000000000000, 0.9898214418809326842, 1.000000000000000000, 0.9898214418809326842, 1.000000000000000000, 0.9898214418809326842, 1.000000000000000000, 0.9898214418809326842, 1.000000000000000000, 0.9898214418809326842, 1.000000000000000000, 0.9898214418809326842, 1.000000000000000000, 0.9898214418809326842, 1.000000000000000000, 0.9898214418809326842, 1.000000000000000000, 0.9898214418809326842, 1.000000000000000000, 0.9898214418809326842, 1.000000000000000000, 0.9898214418809326842, 1.000000000000000000, 0.9898214418809326842, 1.000000000000000000, 0.9898214418809326842, 1.000000000000000000, 0.9898214418809326842, 1.000000000000000000, 0.9898214418809326842, 1.000000000000000000, 0.9898214418809326842, 1.000000000000000000, 0.9898214418809326842, 1.000000000000000000, 0.9898214418809326842, 1.000000000000000000, 0.9898214418809326842, 1.000000000000000000, 0.9898214418809326842, 1.000000000000000000, 0.9898214418809326842, 1.000000000000000000, 0.9898214418809326842, 1.000000000000000000, 0.9898214418809326842, 1.000000000000000000, 0.9898214418809326842, 1.000000000000000000, 0.9898214418809326842, 1.000000000000000000, 0.9898214418809326842, 1.000000000000000000, 0.9898214418809326842, 1.000000000000000000, 0.9898214418809326842, 1.000000000000000000, 0.9898214418809326842, 1.000000000000000000, 0.9898214418809326842, 1.000000000000000000, 0.9898214418809326842, 1.000000000000000000, 0.9898214418809326842, 1.000000000000000000, 0.9898214418809326842, 1.000000000000000000, 0.9898214418809326842, 1.000000000000000000, 0.9898214418809326842, 1.000000000000000000, 0.9898214418809326842, 1.000000000000000000, 0.9898214418809326842, 1.000000000000000000, 0.9898214418809326842, 1.000000000000000000, 0.9898214418809326842, 1.000000000000000000, 0.9898214418809326842, 1.000000000000000000, 0.9898214418809326842, 1.000000000000000000, 0.9898214418809326842, 1.000000000000000000, 0.9898214418809326842, 1.000000000000000000, 0.9898214418809326842, 1.000000000000000000, 0.9898214418809326842, 1.000000000000000000, 0.9898214418809326842, 1.000000000000000000, 0.9898214418809326842, 1.000000000000000000, 0.9898214418809326842, 1.000000000000000000, 0.9898214418809326842, 1.000000000000000000, 0.9898214418809326842, 1.000000000000000000, 0.9898214418809326842, 1.000000000000000000, 0.9898214418809326842, 1.000000000000000000, 0.9898214418809326842, 1.000000000000000000, 0.9898214418809326842, 1.000000000000000000, 0.9898214418809326842, 1.000000000000000000, 0.9898214418809326842, 1.000000000000000000, 0.9898214418809326842, 1.000000000000000000, 0.9898214418809326842, 1.000000000000000000, 0.9898214418809326842, 1.000000000000000000, 0.9898214418809326842, 1.000000000000000000, 0.9898214418809326842, 1.000000000000000000, 0.9898214418809326842, 1.000000000000000000, 0.9898214418809326842, 1.000000000000000000, 0.9898214418809326842, 1.000000000000000000, 0.9898214418809326842, 1.000000000000000000, 0.9898214418809326842, 1.000000000000000000, 0.9898214418809326842, 1.000000000000000000, 0.9898214418809326842, 1.000000000000000000, 0.9898214418809326842, 1.000000000000000000, 0.9898214418809326842, 1.000000000000000000, 0.9898214418809326842, 1.000000000000000000, 0.9898214418809326842, 1.000000000000000000, 0.9898214418809326842, 1.000000000000000000, 0.9898214418809326842, 1.000000000000000000, 0.9898214418809326842, 1.000000000000000000, 0.9898214418809326842, 1.000000000000000000, 0.9898214418809326842, 1.000000000000000000, 0.9898214418809326842, 1.000000000000000000, 0.9898214418809326842, 1.000000000000000000, 0.9898214418809326842, 1.000000000000000000, 0.9898214418809326842, 1.000000000000000000, 0.9898214418809326842, 1.000000000000000000, 0.9898214418809326842, 1.000000000000000000, 0.9898214418809326842, 1.000000000000000000, 0.9898214418809326842, 1.000000000000000000, 0.9898214418809326842, 1.000000000000000000, 0.9898214418809326842, 1.000000000000000000, 0.9898214418809326842, 1.000000000000000000, 0.9898214418809326842, 1.000000000000000000, 0.9898214418809326842, 1.000000000000000000, 0.9898214418809326842, 1.000000000000000000, 0.9898214418809326842, 1.000000000000000000, 0.9898214418809326842, 1.000000000000000000, 0.9898214418809326842, 1.000000000000000000, 0.9898214418809326842, 1.000000000000000000, 0.9898214418809326842, 1.000000000000000000, 0.9898214418809326842, 1.000000000000000000, 0.9898214418809326842, 1.000000000000000000, 0.9898214418809326842, 1.000000000000000000, 0.9898214418809326842, 1.000000000000000000, 0.9898214418809326842, 1.000000000000000000, 0.9898214418809326842, 1.000000000000000000, 0.9898214418809326842, 1.000000000000000000, 0.9898214418809326842, 1.000000000000000000, 0.9898214418809326842, 1.000000000000000000, 0.9898214418809326842, 1.000000000000000000, 0.9898214418809326842, 1.000000000000000000, 0.9898214418809326842, 1.000000000000000000, 0.9898214418809326842, 1.000000000000000000, 0.9898214418809326842, 1.000000000000000000, 0.9898214418809326842, 1.000000000000000000, 0.9898214418809326842, 1.000000000000000000, 0.9898214418809326842, 1.000000000000000000, 0.9898214418809326842, 1.000000000000000000, 0.9898214418809326842, 1.000000000000000000, 0.9898214418809326842, 1.000000000000000000, 0.9898214418809326842, 1.000000000000000000, 0.9898214418809326842, 1.000000000000000000, 0.9898214418809326842, 1.000000000000000000, 0.9898214418809326842, 1.000000000000000000, 0.9898214418809326842, 1.000000000000000000, 0.9898214418809326842, 1.000000000000000000, 0.9898214418809326842, 1.000000000000000000, 0.9898214418809326842, 1.000000000000000000, 0.9898214418809326842, 1.000000000000000000, 0.9898214418809326842, 1.000000000000000000, 0.9898214418809326842, 1.000000000000000000, 0.9898214418809326842, 1.000000000000000000, 0.9898214418809326842, 1.000000000000000000, 0.9898214418809326842, 1.000000000000000000, 0.9898214418809326842, 1.000000000000000000, 0.9898214418809326842, 1.000000000000000000, 0.9898214418809326842, 1.000000000000000000, 0.9898214418809326842, 1.000000000000000000, 0.9898214418809326842, 1.000000000000000000, 0.9898214418809326842, 1.000000000000000000, 0.9898214418809326842, 1.000000000000000000, 0.9898214418809326842, 1.000000000000000000, 0.9898214418809326842, 1.000000000000000000, 0.9898214418809326842, 1.000000000000000000, 0.9898214418809326842, 1.000000000000000000, 0.9898214418809326842, 1.000000000000000000, 0.9898214418809326842, 1.000000000000000000, 0.9898214418809326842, 1.000000000000000000, 0.9898214418809326842, 1.000000000000000000, 0.9898214418809326842, 1.000000000000000000, 0.9898214418809326842, 1.000000000000000000, 0.9898214418809326842, 1.000000000000000000, 0.9898214418809326842, 1.000000000000000000, 0.9898214418809326842, 1.000000000000000000, 0.9898214418809326842, 1.000000000000000000, 0.9898214418809326842, 1.000000000000000000, 0.9898214418809326842, 1.000000000000000000, 0.9898214418809326842, 1.000000000000000000, 0.9898214418809326842, 1.000000000000000000, 0.9898214418809326842, 1.000000000000000000, 0.9898214418809326842, 1.000000000000000000, 0.9898214418809326842, 1.000000000000000000, 0.9898214418809326842, 1.000000000000000000, 0.9898214418809326842, 1.000000000000000000, 0.9898214418809326842, 1.000000000000000000, 0.9898214418809326842, 1.000000000000000000, 0.9898214418809326842, 1.000000000000000000, 0.9898214418809326842, 1.000000000000000000, 0.9898214418809326842, 1.000000000000000000, 0.9898214418809326842, 1.000000000000000000, 0.9898214418809326842, 1.000000000000000000, 0.9898214418809326842, 1.000000000000000000, 0.9898214418809326842, 1.000000000000000000, 0.9898214418809326842, 1.000000000000000000, 0.9898214418809326842, 1.000000000000000000, 0.9898214418809326842, 1.000000000000000000, 0.9898214418809326842, 1.000000000000000000, 0.9898214418809326842, 1.000000000000000000, 0.9898214418809326842, 1.000000000000000000, 0.9898214418809326842, 1.000000000000000000, 0.9898214418809326842, 1.000000000000000000, 0.9898214418809326842, 1.000000000000000000, 0.9898214418809326842, 1.000000000000000000, 0.9898214418809326842, 1.000000000000000000, 0.9898214418809326842, 1.000000000000000000, 0.9898214418809326842, 1.000000000000000000, 0.9898214418809326842, 1.000000000000000000, 0.9898214418809326842, 1.000000000000000000, 0.9898214418809326842, 1.000000000000000000, 0.9898214418809326842, 1.000000000000000000, 0.9898214418809326842, 1.000000000000000000, 0.9898214418809326842, 1.000000000000000000, 0.9898214418809326842, 1.000000000000000000, 0.9898214418809326842, 1.000000000000000000, 0.9898214418809326842, 1.000000000000000000, 0.9898214418809326842, 1.000000000000000000, 0.9898214418809326842, 1.000000000000000000, 0.9898214418809326842, 1.000000000000000000, 0.9898214418809326842, 1.000000000000000000, 0.9898214418809326842, 1.000000000000000000, 0.9898214418809326842, 1.000000000000000000, 0.9898214418809326842, 1.000000000000000000, 0.9898214418809326842, 1.000000000000000000, 0.9898214418809326842, 1.000000000000000000, 0.9898214418809326842, 1.000000000000000000, 0.9898214418809326842, 1.000000000000000000, 0.9898214418809326842, 1.000000000000000000, 0.9898214418809326842, 1.000000000000000000, 0.9898214418809326842, 1.000000000000000000, 0.9898214418809326842, 1.000000000000000000, 0.9898214418809326842, 1.000000000000000000, 0.9898214418809326842, 1.000000000000000000, 0.9898214418809326842, 1.000000000000000000, 0.9898214418809326842, 1.000000000000000000, 0.9898214418809326842, 1.000000000000000000, 0.9898214418809326842, 1.000000000000000000, 0.9898214418809326842, 1.000000000000000000, 0.9898214418809326842, 1.000000000000000000, 0.9898214418809326842, 1.000000000000000000, 0.9898214418809326842, 1.000000000000000000, 0.9898214418809326842, 1.000000000000000000, 0.9898214418809326842, 1.000000000000000000, 0.9898214418809326842, 1.000000000000000000, 0.9898214418809326842, 1.000000000000000000, 0.9898214418809326842, 1.000000000000000000, 0.9898214418809326842, 1.000000000000000000, 0.9898214418809326842, 1.000000000000000000, 0.9898214418809326842, 1.000000000000000000, 0.9898214418809326842, 1.000000000000000000, 0.9898214418809326842, 1.000000000000000000, 0.9898214418809326842, 1.000000000000000000, 0.9898214418809326842, 1.000000000000000000, 0.9898214418809326842, 1.000000000000000000, 0.9898214418809326842, 1.000000000000000000, 0.9898214418809326842, 1.000000000000000000, 0.9898214418809326842, 1.000000000000000000, 0.9898214418809326842, 1.000000000000000000, 0.9898214418809326842, 1.000000000000000000, 0.9898214418809326842, 1.000000000000000000, 0.9898214418809326842, 1.000000000000000000, 0.9898214418809326842, 1.000000000000000000, 0.9898214418809326842, 1.000000000000000000, 0.9898214418809326842, 1.000000000000000000, 0.9898214418809326842, 1.000000000000000000, 0.9898214418809326842, 1.000000000000000000, 0.9898214418809326842, 1.000000000000000000, 0.9898214418809326842, 1.000000000000000000, 0.9898214418809326842, 1.000000000000000000, 0.9898214418809326842, 1.000000000000000000, 0.9898214418809326842, 1.000000000000000000, 0.9898214418809326842, 1.000000000000000000, 0.9898214418809326842, 1.000000000000000000, 0.9898214418809326842, 1.000000000000000000, 0.9898214418809326842, 1.000000000000000000, 0.9898214418809326842, 1.000000000000000000, 0.9898214418809326842, 1.000000000000000000, 0.9898214418809326842, 1.000000000000000000, 0.9898214418809326842, 1.000000000000000000, 0.9898214418809326842, 1.000000000000000000, 0.9898214418809326842, 1.000000000000000000, 0.9898214418809326842, 1.000000000000000000, 0.9898214418809326842, 1.000000000000000000, 0.9898214418809326842, 1.000000000000000000, 0.9898214418809326842, 1.000000000000000000, 0.9898214418809326842, 1.000000000000000000, 0.9898214418809326842, 1.000000000000000000, 0.9898214418809326842, 1.000000000000000000, 0.9898214418809326842, 1.000000000000000000, 0.9898214418809326842, 1.000000000000000000, 0.9898214418809326842, 1.000000000000000000, 0.9898214418809326842, 1.000000000000000000, 0.9898214418809326842, 1.000000000000000000, 0.9898214418809326842, 1.000000000000000000, 0.9898214418809326842, 1.000000000000000000, 0.9898214418809326842, 1.000000000000000000, 0.9898214418809326842, 1.000000000000000000, 0.9898214418809326842, 1.000000000000000000, 0.9898214418809326842, 1.000000000000000000, 0.9898214418809326842, 1.000000000000000000, 0.9898214418809326842, 1.000000000000000000, 0.9898214418809326842, 1.000000000000000000, 0.9898214418809326842, 1.000000000000000000, 0.9898214418809326842, 1.000000000000000000, 0.9898214418809326842, 1.000000000000000000, 0.9898214418809326842, 1.000000000000000000, 0.9898214418809326842, 1.000000000000000000, 0.9898214418809326842, 1.000000000000000000, 0.9898214418809326842, 1.000000000000000000, 0.9898214418809326842, 1.000000000000000000, 0.9898214418809326842, 1.000000000000000000, 0.9898214418809326842, 1.000000000000000000, 0.9898214418809326842, 1.000000000000000000, 0.9898214418809326842, 1.000000000000000000, 0.9898214418809326842, 1.000000000000000000, 0.9898214418809326842, 1.000000000000000000, 0.9898214418809326842, 1.000000000000000000, 0.9898214418809326842, 1.000000000000000000, 0.9898214418809326842, 1.000000000000000000, 0.9898214418809326842, 1.000000000000000000, 0.9898214418809326842, 1.000000000000000000, 0.9898214418809326842, 1.000000000000000000, 0.9898214418809326842, 1.000000000000000000, 0.9898214418809326842, 1.000000000000000000, 0.9898214418809326842, 1.000000000000000000, 0.9898214418809326842, 1.000000000000000000, 0.9898214418809326842, 1.000000000000000000, 0.9898214418809326842, 1.000000000000000000, 0.9898214418809326842, 1.000000000000000000, 0.9898214418809326842, 1.000000000000000000, 0.9898214418809326842, 1.000000000000000000, 0.9898214418809326842, 1.000000000000000000, 0.9898214418809326842, 1.000000000000000000, 0.9898214418809326842, 1.000000000000000000, 0.9898214418809326842, 1.000000000000000000, 0.9898214418809326842, 1.000000000000000000, 0.9898214418809326842, 1.000000000000000000, 0.9898214418809326842, 1.000000000000000000, 0.9898214418809326842, 1.000000000000000000, 0.9898214418809326842, 1.000000000000000000, 0.9898214418809326842, 1.000000000000000000, 0.9898214418809326842, 1.000000000000000000, 0.9898214418809326842, 1.000000000000000000, 0.9898214418809326842, 1.000000000000000000, 0.9898214418809326842, 1.000000000000000000, 0.9898214418809326842, 1.000000000000000000, 0.9898214418809326842, 1.000000000000000000, 0.9898214418809326842, 1.000000000000000000, 0.9898214418809326842, 1.000000000000000000, 0.9898214418809326842, 1.000000000000000000, 0.9898214418809326842, 1.000000000000000000, 0.9898214418809326842, 1.000000000000000000, 0.9898214418809326842, 1.000000000000000000, 0.9898214418809326842, 1.000000000000000000, 0.9898214418809326842, 1.000000000000000000, 0.9898214418809326842, 1.000000000000000000, 0.9898214418809326842, 1.000000000000000000, 0.9898214418809326842, 1.000000000000000000, 0.9898214418809326842, 1.000000000000000000, 0.9898214418809326842, 1.000000000000000000, 0.9898214418809326842, 1.000000000000000000, 0.9898214418809326842, 1.000000000000000000, 0.9898214418809326842, 1.000000000000000000, 0.9898214418809326842, 1.000000000000000000, 0.9898214418809326842, 1.000000000000000000, 0.9898214418809326842, 1.000000000000000000, 0.9898214418809326842, 1.000000000000000000, 0.9898214418809326842, 1.000000000000000000, 0.9898214418809326842, 1.000000000000000000, 0.9898214418809326842, 1.000000000000000000, 0.9898214418809326842, 1.000000000000000000, 0.9898214418809326842, 1.000000000000000000, 0.9898214418809326842, 1.000000000000000000, 0.9898214418809326842, 1.000000000000000000, 0.9898214418809326842, 1.000000000000000000, 0.9898214418809326842, 1.000000000000000000, 0.9898214418809326842, 1.000000000000000000, 0.9898214418809326842, 1.000000000000000000, 0.9898214418809326842, 1.000000000000000000, 0.9898214418809326842, 1.000000000000000000, 0.9898214418809326842, 1.000000000000000000, 0.9898214418809326842, 1.000000000000000000, 0.9898214418809326842, 1.000000000000000000, 0.9898214418809326842, 1.000000000000000000, 0.9898214418809326842, 1.000000000000000000, 0.9898214418809326842, 1.000000000000000000, 0.9898214418809326842, 1.000000000000000000, 0.9898214418809326842, 1.000000000000000000, 0.9898214418809326842, 1.000000000000000000, 0.9898214418809326842, 1.000000000000000000, 0.9898214418809326842, 1.000000000000000000, 0.9898214418809326842, 1.000000000000000000, 0.9898214418809326842, 1.000000000000000000, 0.9898214418809326842, 1.000000000000000000, 0.9898214418809326842, 1.000000000000000000, 0.9898214418809326842, 1.000000000000000000, 0.9898214418809326842, 1.000000000000000000, 0.9898214418809326842, 1.000000000000000000, 0.9898214418809326842, 1.000000000000000000, 0.9898214418809326842, 1.000000000000000000, 0.9898214418809326842, 1.000000000000000000, 0.9898214418809326842, 1.000000000000000000, 0.9898214418809326842, 1.000000000000000000, 0.9898214418809326842, 1.000000000000000000, 0.9898214418809326842, 1.000000000000000000, 0.9898214418809326842, 1.000000000000000000, 0.9898214418809326842, 1.000000000000000000, 0.9898214418809326842, 1.000000000000000000, 0.9898214418809326842, 1.000000000000000000, 0.9898214418809326842, 1.000000000000000000, 0.9898214418809326842, 1.000000000000000000, 0.9898214418809326842, 1.000000000000000000, 0.9898214418809326842, 1.000000000000000000, 0.9898214418809326842, 1.000000000000000000, 0.9898214418809326842, 1.000000000000000000, 0.9898214418809326842, 1.000000000000000000, 0.9898214418809326842, 1.000000000000000000, 0.9898214418809326842, 1.000000000000000000, 0.9898214418809326842, 1.000000000000000000, 0.9898214418809326842, 1.000000000000000000, 0.9898214418809326842, 1.000000000000000000, 0.9898214418809326842, 1.000000000000000000, 0.9898214418809326842, 1.000000000000000000, 0.9898214418809326842, 1.000000000000000000, 0.9898214418809326842, 1.000000000000000000, 0.9898214418809326842, 1.000000000000000000, 0.9898214418809326842, 1.000000000000000000, 0.9898214418809326842, 1.000000000000000000, 0.9898214418809326842, 1.000000000000000000, 0.9898214418809326842, 1.000000000000000000, 0.9898214418809326842, 1.000000000000000000, 0.9898214418809326842, 1.000000000000000000, 0.9898214418809326842, 1.000000000000000000, 0.9898214418809326842, 1.000000000000000000, 0.9898214418809326842, 1.000000000000000000, 0.9898214418809326842, 1.000000000000000000, 0.9898214418809326842, 1.000000000000000000, 0.9898214418809326842, 1.000000000000000000, 0.9898214418809326842, 1.000000000000000000, 0.9898214418809326842, 1.000000000000000000, 0.9898214418809326842, 1.000000000000000000, 0.9898214418809326842, 1.000000000000000000, 0.9898214418809326842, 1.000000000000000000, 0.9898214418809326842, 1.000000000000000000, 0.9898214418809326842, 1.000000000000000000, 0.9898214418809326842, 1.000000000000000000, 0.9898214418809326842, 1.000000000000000000, 0.9898214418809326842, 1.000000000000000000, 0.9898214418809326842, 1.000000000000000000, 0.9898214418809326842, 1.000000000000000000, 0.9898214418809326842, 1.000000000000000000, 0.9898214418809326842, 1.000000000000000000, 0.9898214418809326842, 1.000000000000000000, 0.9898214418809326842, 1.000000000000000000, 0.9898214418809326842, 1.000000000000000000, 0.9961809353924466759, 0.9952277490961531914),
 ( 0.3333333333333333703, 0.3299404806269776169, 0.3333333333333333703, 0.3299404806269776169, 0.3333333333333333703, 0.3299404806269776169, 0.3333333333333333703, 0.3299404806269776169, 0.3333333333333333703, 0.3299404806269776169, 0.3333333333333333703, 0.3299404806269776169, 0.3333333333333333703, 0.3299404806269776169, 0.3333333333333333703, 0.3299404806269776169, 0.3333333333333333703, 0.3299404806269776169, 0.3333333333333333703, 0.3299404806269776169, 0.3333333333333333703, 0.3299404806269776169, 0.3333333333333333703, 0.3299404806269776169, 0.3333333333333333703, 0.3299404806269776169, 0.3333333333333333703, 0.3299404806269776169, 0.3333333333333333703, 0.3299404806269776169, 0.3333333333333333703, 0.3299404806269776169, 0.3333333333333333703, 0.3299404806269776169, 0.3333333333333333703, 0.3299404806269776169, 0.3333333333333333703, 0.3299404806269776169, 0.3333333333333333703, 0.3299404806269776169, 0.3333333333333333703, 0.3299404806269776169, 0.3333333333333333703, 0.3299404806269776169, 0.3333333333333333703, 0.3299404806269776169, 0.3333333333333333703, 0.3299404806269776169, 0.3333333333333333703, 0.3299404806269776169, 0.3333333333333333703, 0.3299404806269776169, 0.3333333333333333703, 0.3299404806269776169, 0.3333333333333333703, 0.3299404806269776169, 0.3333333333333333703, 0.3299404806269776169, 0.3333333333333333703, 0.3299404806269776169, 0.3333333333333333703, 0.3299404806269776169, 0.3333333333333333703, 0.3299404806269776169, 0.3333333333333333703, 0.3299404806269776169, 0.3333333333333333703, 0.3299404806269776169, 0.3333333333333333703, 0.3299404806269776169, 0.3333333333333333703, 0.3299404806269776169, 0.3333333333333333703, 0.3299404806269776169, 0.3333333333333333703, 0.3299404806269776169, 0.3333333333333333703, 0.3299404806269776169, 0.3333333333333333703, 0.3299404806269776169, 0.3333333333333333703, 0.3299404806269776169, 0.3333333333333333703, 0.3299404806269776169, 0.3333333333333333703, 0.3299404806269776169, 0.3333333333333333703, 0.3299404806269776169, 0.3333333333333333703, 0.3299404806269776169, 0.3333333333333333703, 0.3299404806269776169, 0.3333333333333333703, 0.3299404806269776169, 0.3333333333333333703, 0.3299404806269776169, 0.3333333333333333703, 0.3299404806269776169, 0.3333333333333333703, 0.3299404806269776169, 0.3333333333333333703, 0.3299404806269776169, 0.3333333333333333703, 0.3299404806269776169, 0.3333333333333333703, 0.3299404806269776169, 0.3333333333333333703, 0.3299404806269776169, 0.3333333333333333703, 0.3299404806269776169, 0.3333333333333333703, 0.3299404806269776169, 0.3333333333333333703, 0.3299404806269776169, 0.3333333333333333703, 0.3299404806269776169, 0.3333333333333333703, 0.3299404806269776169, 0.3333333333333333703, 0.3299404806269776169, 0.3333333333333333703, 0.3299404806269776169, 0.3333333333333333703, 0.3299404806269776169, 0.3333333333333333703, 0.3299404806269776169, 0.3333333333333333703, 0.3299404806269776169, 0.3333333333333333703, 0.3299404806269776169, 0.3333333333333333703, 0.3299404806269776169, 0.3333333333333333703, 0.3299404806269776169, 0.3333333333333333703, 0.3299404806269776169, 0.3333333333333333703, 0.3299404806269776169, 0.3333333333333333703, 0.3299404806269776169, 0.3333333333333333703, 0.3299404806269776169, 0.3333333333333333703, 0.3299404806269776169, 0.3333333333333333703, 0.3299404806269776169, 0.3333333333333333703, 0.3299404806269776169, 0.3333333333333333703, 0.3299404806269776169, 0.3333333333333333703, 0.3299404806269776169, 0.3333333333333333703, 0.3299404806269776169, 0.3333333333333333703, 0.3299404806269776169, 0.3333333333333333703, 0.3299404806269776169, 0.3333333333333333703, 0.3299404806269776169, 0.3333333333333333703, 0.3299404806269776169, 0.3333333333333333703, 0.3299404806269776169, 0.3333333333333333703, 0.3299404806269776169, 0.3333333333333333703, 0.3299404806269776169, 0.3333333333333333703, 0.3299404806269776169, 0.3333333333333333703, 0.3299404806269776169, 0.3333333333333333703, 0.3299404806269776169, 0.3333333333333333703, 0.3299404806269776169, 0.3333333333333333703, 0.3299404806269776169, 0.3333333333333333703, 0.3299404806269776169, 0.3333333333333333703, 0.3299404806269776169, 0.3333333333333333703, 0.3299404806269776169, 0.3333333333333333703, 0.3299404806269776169, 0.3333333333333333703, 0.3299404806269776169, 0.3333333333333333703, 0.3299404806269776169, 0.3333333333333333703, 0.3299404806269776169, 0.3333333333333333703, 0.3299404806269776169, 0.3333333333333333703, 0.3299404806269776169, 0.3333333333333333703, 0.3299404806269776169, 0.3333333333333333703, 0.3299404806269776169, 0.3333333333333333703, 0.3299404806269776169, 0.3333333333333333703, 0.3299404806269776169, 0.3333333333333333703, 0.3299404806269776169, 0.3333333333333333703, 0.3299404806269776169, 0.3333333333333333703, 0.3299404806269776169, 0.3333333333333333703, 0.3299404806269776169, 0.3333333333333333703, 0.3299404806269776169, 0.3333333333333333703, 0.3299404806269776169, 0.3333333333333333703, 0.3299404806269776169, 0.3333333333333333703, 0.3299404806269776169, 0.3333333333333333703, 0.3299404806269776169, 0.3333333333333333703, 0.3299404806269776169, 0.3333333333333333703, 0.3299404806269776169, 0.3333333333333333703, 0.3299404806269776169, 0.3333333333333333703, 0.3299404806269776169, 0.3333333333333333703, 0.3299404806269776169, 0.3333333333333333703, 0.3299404806269776169, 0.3333333333333333703, 0.3299404806269776169, 0.3333333333333333703, 0.3299404806269776169, 0.3333333333333333703, 0.3299404806269776169, 0.3333333333333333703, 0.3299404806269776169, 0.3333333333333333703, 0.3299404806269776169, 0.3333333333333333703, 0.3299404806269776169, 0.3333333333333333703, 0.3299404806269776169, 0.3333333333333333703, 0.3299404806269776169, 0.3333333333333333703, 0.3299404806269776169, 0.3333333333333333703, 0.3299404806269776169, 0.3333333333333333703, 0.3299404806269776169, 0.3333333333333333703, 0.3299404806269776169, 0.3333333333333333703, 0.3299404806269776169, 0.3333333333333333703, 0.3299404806269776169, 0.3333333333333333703, 0.3299404806269776169, 0.3333333333333333703, 0.3299404806269776169, 0.3333333333333333703, 0.3299404806269776169, 0.3333333333333333703, 0.3299404806269776169, 0.3333333333333333703, 0.3299404806269776169, 0.3333333333333333703, 0.3299404806269776169, 0.3333333333333333703, 0.3299404806269776169, 0.3333333333333333703, 0.3299404806269776169, 0.3333333333333333703, 0.3299404806269776169, 0.3333333333333333703, 0.3299404806269776169, 0.3333333333333333703, 0.3299404806269776169, 0.3333333333333333703, 0.3299404806269776169, 0.3333333333333333703, 0.3299404806269776169, 0.3333333333333333703, 0.3299404806269776169, 0.3333333333333333703, 0.3299404806269776169, 0.3333333333333333703, 0.3299404806269776169, 0.3333333333333333703, 0.3299404806269776169, 0.3333333333333333703, 0.3299404806269776169, 0.3333333333333333703, 0.3299404806269776169, 0.3333333333333333703, 0.3299404806269776169, 0.3333333333333333703, 0.3299404806269776169, 0.3333333333333333703, 0.3299404806269776169, 0.3333333333333333703, 0.3299404806269776169, 0.3333333333333333703, 0.3299404806269776169, 0.3333333333333333703, 0.3299404806269776169, 0.3333333333333333703, 0.3299404806269776169, 0.3333333333333333703, 0.3299404806269776169, 0.3333333333333333703, 0.3299404806269776169, 0.3333333333333333703, 0.3299404806269776169, 0.3333333333333333703, 0.3299404806269776169, 0.3333333333333333703, 0.3299404806269776169, 0.3333333333333333703, 0.3299404806269776169, 0.3333333333333333703, 0.3299404806269776169, 0.3333333333333333703, 0.3299404806269776169, 0.3333333333333333703, 0.3299404806269776169, 0.3333333333333333703, 0.3299404806269776169, 0.3333333333333333703, 0.3299404806269776169, 0.3333333333333333703, 0.3299404806269776169, 0.3333333333333333703, 0.3299404806269776169, 0.3333333333333333703, 0.3299404806269776169, 0.3333333333333333703, 0.3299404806269776169, 0.3333333333333333703, 0.3299404806269776169, 0.3333333333333333703, 0.3299404806269776169, 0.3333333333333333703, 0.3299404806269776169, 0.3333333333333333703, 0.3299404806269776169, 0.3333333333333333703, 0.3299404806269776169, 0.3333333333333333703, 0.3299404806269776169, 0.3333333333333333703, 0.3299404806269776169, 0.3333333333333333703, 0.3299404806269776169, 0.3333333333333333703, 0.3299404806269776169, 0.3333333333333333703, 0.3299404806269776169, 0.3333333333333333703, 0.3299404806269776169, 0.3333333333333333703, 0.3299404806269776169, 0.3333333333333333703, 0.3299404806269776169, 0.3333333333333333703, 0.3299404806269776169, 0.3333333333333333703, 0.3299404806269776169, 0.3333333333333333703, 0.3299404806269776169, 0.3333333333333333703, 0.3299404806269776169, 0.3333333333333333703, 0.3299404806269776169, 0.3333333333333333703, 0.3299404806269776169, 0.3333333333333333703, 0.3299404806269776169, 0.3333333333333333703, 0.3299404806269776169, 0.3333333333333333703, 0.3299404806269776169, 0.3333333333333333703, 0.3299404806269776169, 0.3333333333333333703, 0.3299404806269776169, 0.3333333333333333703, 0.3299404806269776169, 0.3333333333333333703, 0.3299404806269776169, 0.3333333333333333703, 0.3299404806269776169, 0.3333333333333333703, 0.3299404806269776169, 0.3333333333333333703, 0.3299404806269776169, 0.3333333333333333703, 0.3299404806269776169, 0.3333333333333333703, 0.3299404806269776169, 0.3333333333333333703, 0.3299404806269776169, 0.3333333333333333703, 0.3299404806269776169, 0.3333333333333333703, 0.3299404806269776169, 0.3333333333333333703, 0.3299404806269776169, 0.3333333333333333703, 0.3299404806269776169, 0.3333333333333333703, 0.3299404806269776169, 0.3333333333333333703, 0.3299404806269776169, 0.3333333333333333703, 0.3299404806269776169, 0.3333333333333333703, 0.3299404806269776169, 0.3333333333333333703, 0.3299404806269776169, 0.3333333333333333703, 0.3299404806269776169, 0.3333333333333333703, 0.3299404806269776169, 0.3333333333333333703, 0.3299404806269776169, 0.3333333333333333703, 0.3299404806269776169, 0.3333333333333333703, 0.3299404806269776169, 0.3333333333333333703, 0.3299404806269776169, 0.3333333333333333703, 0.3299404806269776169, 0.3333333333333333703, 0.3299404806269776169, 0.3333333333333333703, 0.3299404806269776169, 0.3333333333333333703, 0.3299404806269776169, 0.3333333333333333703, 0.3299404806269776169, 0.3333333333333333703, 0.3299404806269776169, 0.3333333333333333703, 0.3299404806269776169, 0.3333333333333333703, 0.3299404806269776169, 0.3333333333333333703, 0.3299404806269776169, 0.3333333333333333703, 0.3299404806269776169, 0.3333333333333333703, 0.3299404806269776169, 0.3333333333333333703, 0.3299404806269776169, 0.3333333333333333703, 0.3299404806269776169, 0.3333333333333333703, 0.3299404806269776169, 0.3333333333333333703, 0.3299404806269776169, 0.3333333333333333703, 0.3299404806269776169, 0.3333333333333333703, 0.3299404806269776169, 0.3333333333333333703, 0.3299404806269776169, 0.3333333333333333703, 0.3299404806269776169, 0.3333333333333333703, 0.3299404806269776169, 0.3333333333333333703, 0.3299404806269776169, 0.3333333333333333703, 0.3299404806269776169, 0.3333333333333333703, 0.3299404806269776169, 0.3333333333333333703, 0.3299404806269776169, 0.3333333333333333703, 0.3299404806269776169, 0.3333333333333333703, 0.3299404806269776169, 0.3333333333333333703, 0.3299404806269776169, 0.3333333333333333703, 0.3299404806269776169, 0.3333333333333333703, 0.3299404806269776169, 0.3333333333333333703, 0.3299404806269776169, 0.3333333333333333703, 0.3299404806269776169, 0.3333333333333333703, 0.3299404806269776169, 0.3333333333333333703, 0.3299404806269776169, 0.3333333333333333703, 0.3299404806269776169, 0.3333333333333333703, 0.3299404806269776169, 0.3333333333333333703, 0.3299404806269776169, 0.3333333333333333703, 0.3299404806269776169, 0.3333333333333333703, 0.3299404806269776169, 0.3333333333333333703, 0.3299404806269776169, 0.3333333333333333703, 0.3299404806269776169, 0.3333333333333333703, 0.3299404806269776169, 0.3333333333333333703, 0.3299404806269776169, 0.3333333333333333703, 0.3299404806269776169, 0.3333333333333333703, 0.3299404806269776169, 0.3333333333333333703, 0.3299404806269776169, 0.3333333333333333703, 0.3299404806269776169, 0.3333333333333333703, 0.3299404806269776169, 0.3333333333333333703, 0.3299404806269776169, 0.3333333333333333703, 0.3299404806269776169, 0.3333333333333333703, 0.3299404806269776169, 0.3333333333333333703, 0.3299404806269776169, 0.3333333333333333703, 0.3299404806269776169, 0.3333333333333333703, 0.3299404806269776169, 0.3333333333333333703, 0.3299404806269776169, 0.3333333333333333703, 0.3299404806269776169, 0.3333333333333333703, 0.3299404806269776169, 0.3333333333333333703, 0.3299404806269776169, 0.3333333333333333703, 0.3299404806269776169, 0.3333333333333333703, 0.3299404806269776169, 0.3333333333333333703, 0.3299404806269776169, 0.3333333333333333703, 0.3299404806269776169, 0.3333333333333333703, 0.3299404806269776169, 0.3333333333333333703, 0.3299404806269776169, 0.3333333333333333703, 0.3299404806269776169, 0.3333333333333333703, 0.3299404806269776169, 0.3333333333333333703, 0.3299404806269776169, 0.3333333333333333703, 0.3299404806269776169, 0.3333333333333333703, 0.3299404806269776169, 0.3333333333333333703, 0.3299404806269776169, 0.3333333333333333703, 0.3299404806269776169, 0.3333333333333333703, 0.3299404806269776169, 0.3333333333333333703, 0.3299404806269776169, 0.3333333333333333703, 0.3299404806269776169, 0.3333333333333333703, 0.3299404806269776169, 0.3333333333333333703, 0.3299404806269776169, 0.3333333333333333703, 0.3299404806269776169, 0.3333333333333333703, 0.3299404806269776169, 0.3333333333333333703, 0.3299404806269776169, 0.3333333333333333703, 0.3299404806269776169, 0.3333333333333333703, 0.3299404806269776169, 0.3333333333333333703, 0.3299404806269776169, 0.3333333333333333703, 0.3299404806269776169, 0.3333333333333333703, 0.3299404806269776169, 0.3333333333333333703, 0.3299404806269776169, 0.3333333333333333703, 0.3299404806269776169, 0.3333333333333333703, 0.3299404806269776169, 0.3333333333333333703, 0.3299404806269776169, 0.3333333333333333703, 0.3299404806269776169, 0.3333333333333333703, 0.3299404806269776169, 0.3333333333333333703, 0.3299404806269776169, 0.3333333333333333703, 0.3299404806269776169, 0.3333333333333333703, 0.3299404806269776169, 0.3333333333333333703, 0.3299404806269776169, 0.3333333333333333703, 0.3299404806269776169, 0.3333333333333333703, 0.3299404806269776169, 0.3333333333333333703, 0.3299404806269776169, 0.3333333333333333703, 0.3299404806269776169, 0.3333333333333333703, 0.3299404806269776169, 0.3333333333333333703, 0.3299404806269776169, 0.3333333333333333703, 0.3299404806269776169, 0.3333333333333333703, 0.3299404806269776169, 0.3333333333333333703, 0.3299404806269776169, 0.3333333333333333703, 0.3299404806269776169, 0.3333333333333333703, 0.3299404806269776169, 0.3333333333333333703, 0.3299404806269776169, 0.3333333333333333703, 0.3299404806269776169, 0.3333333333333333703, 0.3299404806269776169, 0.3333333333333333703, 0.3299404806269776169, 0.3333333333333333703, 0.3299404806269776169, 0.3333333333333333703, 0.3299404806269776169, 0.3333333333333333703, 0.3299404806269776169, 0.3333333333333333703, 0.3299404806269776169, 0.3333333333333333703, 0.3299404806269776169, 0.3333333333333333703, 0.3299404806269776169, 0.3333333333333333703, 0.3299404806269776169, 0.3333333333333333703, 0.3299404806269776169, 0.3333333333333333703, 0.3299404806269776169, 0.3333333333333333703, 0.3299404806269776169, 0.3333333333333333703, 0.3299404806269776169, 0.3333333333333333703, 0.3299404806269776169, 0.3333333333333333703, 0.3299404806269776169, 0.3333333333333333703, 0.3299404806269776169, 0.3333333333333333703, 0.3299404806269776169, 0.3333333333333333703, 0.3299404806269776169, 0.3333333333333333703, 0.3299404806269776169, 0.3333333333333333703, 0.3299404806269776169, 0.3333333333333333703, 0.3299404806269776169, 0.3333333333333333703, 0.3299404806269776169, 0.3333333333333333703, 0.3299404806269776169, 0.3333333333333333703, 0.3299404806269776169, 0.3333333333333333703, 0.3299404806269776169, 0.3333333333333333703, 0.3299404806269776169, 0.3333333333333333703, 0.3299404806269776169, 0.3333333333333333703, 0.3299404806269776169, 0.3333333333333333703, 0.3299404806269776169, 0.3333333333333333703, 0.3299404806269776169, 0.3333333333333333703, 0.3299404806269776169, 0.3333333333333333703, 0.3299404806269776169, 0.3333333333333333703, 0.3299404806269776169, 0.3333333333333333703, 0.3299404806269776169, 0.3333333333333333703, 0.3299404806269776169, 0.3333333333333333703, 0.3299404806269776169, 0.3333333333333333703, 0.3299404806269776169, 0.3333333333333333703, 0.3299404806269776169, 0.3333333333333333703, 0.3299404806269776169, 0.3333333333333333703, 0.3299404806269776169, 0.3333333333333333703, 0.3299404806269776169, 0.3333333333333333703, 0.3299404806269776169, 0.3333333333333333703, 0.3299404806269776169, 0.3333333333333333703, 0.3299404806269776169, 0.3333333333333333703, 0.3299404806269776169, 0.3333333333333333703, 0.3299404806269776169, 0.3333333333333333703, 0.3299404806269776169, 0.3333333333333333703, 0.3299404806269776169, 0.3333333333333333703, 0.3299404806269776169, 0.3333333333333333703, 0.3299404806269776169, 0.3333333333333333703, 0.3299404806269776169, 0.3333333333333333703, 0.3299404806269776169, 0.3333333333333333703, 0.3299404806269776169, 0.3333333333333333703, 0.3299404806269776169, 0.3333333333333333703, 0.3299404806269776169, 0.3333333333333333703, 0.3299404806269776169, 0.3333333333333333703, 0.3299404806269776169, 0.3333333333333333703, 0.3299404806269776169, 0.3333333333333333703, 0.3299404806269776169, 0.3333333333333333703, 0.3299404806269776169, 0.3333333333333333703, 0.3299404806269776169, 0.3333333333333333703, 0.3299404806269776169, 0.3333333333333333703, 0.3299404806269776169, 0.3333333333333333703, 0.3299404806269776169, 0.3333333333333333703, 0.3299404806269776169, 0.3333333333333333703, 0.3299404806269776169, 0.3333333333333333703, 0.3299404806269776169, 0.3333333333333333703, 0.3299404806269776169, 0.3333333333333333703, 0.3299404806269776169, 0.3333333333333333703, 0.3299404806269776169, 0.3333333333333333703, 0.3299404806269776169, 0.3333333333333333703, 0.3299404806269776169, 0.3333333333333333703, 0.3299404806269776169, 0.3333333333333333703, 0.3299404806269776169, 0.3333333333333333703, 0.3299404806269776169, 0.3333333333333333703, 0.3299404806269776169, 0.3333333333333333703, 0.3299404806269776169, 0.3333333333333333703, 0.3299404806269776169, 0.3333333333333333703, 0.3299404806269776169, 0.3333333333333333703, 0.3299404806269776169, 0.3333333333333333703, 0.3299404806269776169, 0.3333333333333333703, 0.3299404806269776169, 0.3333333333333333703, 0.3299404806269776169, 0.3333333333333333703, 0.3299404806269776169, 0.3333333333333333703, 0.3299404806269776169, 0.3333333333333333703, 0.3299404806269776169, 0.3333333333333333703, 0.3299404806269776169, 0.3333333333333333703, 0.3299404806269776169, 0.3333333333333333703, 0.3299404806269776169, 0.3333333333333333703, 0.3299404806269776169, 0.3333333333333333703, 0.3299404806269776169, 0.3333333333333333703, 0.3299404806269776169, 0.3333333333333333703, 0.3299404806269776169, 0.3333333333333333703, 0.3299404806269776169, 0.3333333333333333703, 0.3299404806269776169, 0.3333333333333333703, 0.3299404806269776169, 0.3333333333333333703, 0.3299404806269776169, 0.3333333333333333703, 0.3299404806269776169, 0.3333333333333333703, 0.3299404806269776169, 0.3333333333333333703, 0.3299404806269776169, 0.3333333333333333703, 0.3299404806269776169, 0.3333333333333333703, 0.3299404806269776169, 0.3333333333333333703, 0.3299404806269776169, 0.3333333333333333703, 0.3299404806269776169, 0.3333333333333333703, 0.3299404806269776169, 0.3333333333333333703, 0.3320603117974822438, 0.3317425830320511193),
 ( 0.3333333333333333703, 0.3299404806269776169, 0.3333333333333333703, 0.3299404806269776169, 0.3333333333333333703, 0.3299404806269776169, 0.3333333333333333703, 0.3299404806269776169, 0.3333333333333333703, 0.3299404806269776169, 0.3333333333333333703, 0.3299404806269776169, 0.3333333333333333703, 0.3299404806269776169, 0.3333333333333333703, 0.3299404806269776169, 0.3333333333333333703, 0.3299404806269776169, 0.3333333333333333703, 0.3299404806269776169, 0.3333333333333333703, 0.3299404806269776169, 0.3333333333333333703, 0.3299404806269776169, 0.3333333333333333703, 0.3299404806269776169, 0.3333333333333333703, 0.3299404806269776169, 0.3333333333333333703, 0.3299404806269776169, 0.3333333333333333703, 0.3299404806269776169, 0.3333333333333333703, 0.3299404806269776169, 0.3333333333333333703, 0.3299404806269776169, 0.3333333333333333703, 0.3299404806269776169, 0.3333333333333333703, 0.3299404806269776169, 0.3333333333333333703, 0.3299404806269776169, 0.3333333333333333703, 0.3299404806269776169, 0.3333333333333333703, 0.3299404806269776169, 0.3333333333333333703, 0.3299404806269776169, 0.3333333333333333703, 0.3299404806269776169, 0.3333333333333333703, 0.3299404806269776169, 0.3333333333333333703, 0.3299404806269776169, 0.3333333333333333703, 0.3299404806269776169, 0.3333333333333333703, 0.3299404806269776169, 0.3333333333333333703, 0.3299404806269776169, 0.3333333333333333703, 0.3299404806269776169, 0.3333333333333333703, 0.3299404806269776169, 0.3333333333333333703, 0.3299404806269776169, 0.3333333333333333703, 0.3299404806269776169, 0.3333333333333333703, 0.3299404806269776169, 0.3333333333333333703, 0.3299404806269776169, 0.3333333333333333703, 0.3299404806269776169, 0.3333333333333333703, 0.3299404806269776169, 0.3333333333333333703, 0.3299404806269776169, 0.3333333333333333703, 0.3299404806269776169, 0.3333333333333333703, 0.3299404806269776169, 0.3333333333333333703, 0.3299404806269776169, 0.3333333333333333703, 0.3299404806269776169, 0.3333333333333333703, 0.3299404806269776169, 0.3333333333333333703, 0.3299404806269776169, 0.3333333333333333703, 0.3299404806269776169, 0.3333333333333333703, 0.3299404806269776169, 0.3333333333333333703, 0.3299404806269776169, 0.3333333333333333703, 0.3299404806269776169, 0.3333333333333333703, 0.3299404806269776169, 0.3333333333333333703, 0.3299404806269776169, 0.3333333333333333703, 0.3299404806269776169, 0.3333333333333333703, 0.3299404806269776169, 0.3333333333333333703, 0.3299404806269776169, 0.3333333333333333703, 0.3299404806269776169, 0.3333333333333333703, 0.3299404806269776169, 0.3333333333333333703, 0.3299404806269776169, 0.3333333333333333703, 0.3299404806269776169, 0.3333333333333333703, 0.3299404806269776169, 0.3333333333333333703, 0.3299404806269776169, 0.3333333333333333703, 0.3299404806269776169, 0.3333333333333333703, 0.3299404806269776169, 0.3333333333333333703, 0.3299404806269776169, 0.3333333333333333703, 0.3299404806269776169, 0.3333333333333333703, 0.3299404806269776169, 0.3333333333333333703, 0.3299404806269776169, 0.3333333333333333703, 0.3299404806269776169, 0.3333333333333333703, 0.3299404806269776169, 0.3333333333333333703, 0.3299404806269776169, 0.3333333333333333703, 0.3299404806269776169, 0.3333333333333333703, 0.3299404806269776169, 0.3333333333333333703, 0.3299404806269776169, 0.3333333333333333703, 0.3299404806269776169, 0.3333333333333333703, 0.3299404806269776169, 0.3333333333333333703, 0.3299404806269776169, 0.3333333333333333703, 0.3299404806269776169, 0.3333333333333333703, 0.3299404806269776169, 0.3333333333333333703, 0.3299404806269776169, 0.3333333333333333703, 0.3299404806269776169, 0.3333333333333333703, 0.3299404806269776169, 0.3333333333333333703, 0.3299404806269776169, 0.3333333333333333703, 0.3299404806269776169, 0.3333333333333333703, 0.3299404806269776169, 0.3333333333333333703, 0.3299404806269776169, 0.3333333333333333703, 0.3299404806269776169, 0.3333333333333333703, 0.3299404806269776169, 0.3333333333333333703, 0.3299404806269776169, 0.3333333333333333703, 0.3299404806269776169, 0.3333333333333333703, 0.3299404806269776169, 0.3333333333333333703, 0.3299404806269776169, 0.3333333333333333703, 0.3299404806269776169, 0.3333333333333333703, 0.3299404806269776169, 0.3333333333333333703, 0.3299404806269776169, 0.3333333333333333703, 0.3299404806269776169, 0.3333333333333333703, 0.3299404806269776169, 0.3333333333333333703, 0.3299404806269776169, 0.3333333333333333703, 0.3299404806269776169, 0.3333333333333333703, 0.3299404806269776169, 0.3333333333333333703, 0.3299404806269776169, 0.3333333333333333703, 0.3299404806269776169, 0.3333333333333333703, 0.3299404806269776169, 0.3333333333333333703, 0.3299404806269776169, 0.3333333333333333703, 0.3299404806269776169, 0.3333333333333333703, 0.3299404806269776169, 0.3333333333333333703, 0.3299404806269776169, 0.3333333333333333703, 0.3299404806269776169, 0.3333333333333333703, 0.3299404806269776169, 0.3333333333333333703, 0.3299404806269776169, 0.3333333333333333703, 0.3299404806269776169, 0.3333333333333333703, 0.3299404806269776169, 0.3333333333333333703, 0.3299404806269776169, 0.3333333333333333703, 0.3299404806269776169, 0.3333333333333333703, 0.3299404806269776169, 0.3333333333333333703, 0.3299404806269776169, 0.3333333333333333703, 0.3299404806269776169, 0.3333333333333333703, 0.3299404806269776169, 0.3333333333333333703, 0.3299404806269776169, 0.3333333333333333703, 0.3299404806269776169, 0.3333333333333333703, 0.3299404806269776169, 0.3333333333333333703, 0.3299404806269776169, 0.3333333333333333703, 0.3299404806269776169, 0.3333333333333333703, 0.3299404806269776169, 0.3333333333333333703, 0.3299404806269776169, 0.3333333333333333703, 0.3299404806269776169, 0.3333333333333333703, 0.3299404806269776169, 0.3333333333333333703, 0.3299404806269776169, 0.3333333333333333703, 0.3299404806269776169, 0.3333333333333333703, 0.3299404806269776169, 0.3333333333333333703, 0.3299404806269776169, 0.3333333333333333703, 0.3299404806269776169, 0.3333333333333333703, 0.3299404806269776169, 0.3333333333333333703, 0.3299404806269776169, 0.3333333333333333703, 0.3299404806269776169, 0.3333333333333333703, 0.3299404806269776169, 0.3333333333333333703, 0.3299404806269776169, 0.3333333333333333703, 0.3299404806269776169, 0.3333333333333333703, 0.3299404806269776169, 0.3333333333333333703, 0.3299404806269776169, 0.3333333333333333703, 0.3299404806269776169, 0.3333333333333333703, 0.3299404806269776169, 0.3333333333333333703, 0.3299404806269776169, 0.3333333333333333703, 0.3299404806269776169, 0.3333333333333333703, 0.3299404806269776169, 0.3333333333333333703, 0.3299404806269776169, 0.3333333333333333703, 0.3299404806269776169, 0.3333333333333333703, 0.3299404806269776169, 0.3333333333333333703, 0.3299404806269776169, 0.3333333333333333703, 0.3299404806269776169, 0.3333333333333333703, 0.3299404806269776169, 0.3333333333333333703, 0.3299404806269776169, 0.3333333333333333703, 0.3299404806269776169, 0.3333333333333333703, 0.3299404806269776169, 0.3333333333333333703, 0.3299404806269776169, 0.3333333333333333703, 0.3299404806269776169, 0.3333333333333333703, 0.3299404806269776169, 0.3333333333333333703, 0.3299404806269776169, 0.3333333333333333703, 0.3299404806269776169, 0.3333333333333333703, 0.3299404806269776169, 0.3333333333333333703, 0.3299404806269776169, 0.3333333333333333703, 0.3299404806269776169, 0.3333333333333333703, 0.3299404806269776169, 0.3333333333333333703, 0.3299404806269776169, 0.3333333333333333703, 0.3299404806269776169, 0.3333333333333333703, 0.3299404806269776169, 0.3333333333333333703, 0.3299404806269776169, 0.3333333333333333703, 0.3299404806269776169, 0.3333333333333333703, 0.3299404806269776169, 0.3333333333333333703, 0.3299404806269776169, 0.3333333333333333703, 0.3299404806269776169, 0.3333333333333333703, 0.3299404806269776169, 0.3333333333333333703, 0.3299404806269776169, 0.3333333333333333703, 0.3299404806269776169, 0.3333333333333333703, 0.3299404806269776169, 0.3333333333333333703, 0.3299404806269776169, 0.3333333333333333703, 0.3299404806269776169, 0.3333333333333333703, 0.3299404806269776169, 0.3333333333333333703, 0.3299404806269776169, 0.3333333333333333703, 0.3299404806269776169, 0.3333333333333333703, 0.3299404806269776169, 0.3333333333333333703, 0.3299404806269776169, 0.3333333333333333703, 0.3299404806269776169, 0.3333333333333333703, 0.3299404806269776169, 0.3333333333333333703, 0.3299404806269776169, 0.3333333333333333703, 0.3299404806269776169, 0.3333333333333333703, 0.3299404806269776169, 0.3333333333333333703, 0.3299404806269776169, 0.3333333333333333703, 0.3299404806269776169, 0.3333333333333333703, 0.3299404806269776169, 0.3333333333333333703, 0.3299404806269776169, 0.3333333333333333703, 0.3299404806269776169, 0.3333333333333333703, 0.3299404806269776169, 0.3333333333333333703, 0.3299404806269776169, 0.3333333333333333703, 0.3299404806269776169, 0.3333333333333333703, 0.3299404806269776169, 0.3333333333333333703, 0.3299404806269776169, 0.3333333333333333703, 0.3299404806269776169, 0.3333333333333333703, 0.3299404806269776169, 0.3333333333333333703, 0.3299404806269776169, 0.3333333333333333703, 0.3299404806269776169, 0.3333333333333333703, 0.3299404806269776169, 0.3333333333333333703, 0.3299404806269776169, 0.3333333333333333703, 0.3299404806269776169, 0.3333333333333333703, 0.3299404806269776169, 0.3333333333333333703, 0.3299404806269776169, 0.3333333333333333703, 0.3299404806269776169, 0.3333333333333333703, 0.3299404806269776169, 0.3333333333333333703, 0.3299404806269776169, 0.3333333333333333703, 0.3299404806269776169, 0.3333333333333333703, 0.3299404806269776169, 0.3333333333333333703, 0.3299404806269776169, 0.3333333333333333703, 0.3299404806269776169, 0.3333333333333333703, 0.3299404806269776169, 0.3333333333333333703, 0.3299404806269776169, 0.3333333333333333703, 0.3299404806269776169, 0.3333333333333333703, 0.3299404806269776169, 0.3333333333333333703, 0.3299404806269776169, 0.3333333333333333703, 0.3299404806269776169, 0.3333333333333333703, 0.3299404806269776169, 0.3333333333333333703, 0.3299404806269776169, 0.3333333333333333703, 0.3299404806269776169, 0.3333333333333333703, 0.3299404806269776169, 0.3333333333333333703, 0.3299404806269776169, 0.3333333333333333703, 0.3299404806269776169, 0.3333333333333333703, 0.3299404806269776169, 0.3333333333333333703, 0.3299404806269776169, 0.3333333333333333703, 0.3299404806269776169, 0.3333333333333333703, 0.3299404806269776169, 0.3333333333333333703, 0.3299404806269776169, 0.3333333333333333703, 0.3299404806269776169, 0.3333333333333333703, 0.3299404806269776169, 0.3333333333333333703, 0.3299404806269776169, 0.3333333333333333703, 0.3299404806269776169, 0.3333333333333333703, 0.3299404806269776169, 0.3333333333333333703, 0.3299404806269776169, 0.3333333333333333703, 0.3299404806269776169, 0.3333333333333333703, 0.3299404806269776169, 0.3333333333333333703, 0.3299404806269776169, 0.3333333333333333703, 0.3299404806269776169, 0.3333333333333333703, 0.3299404806269776169, 0.3333333333333333703, 0.3299404806269776169, 0.3333333333333333703, 0.3299404806269776169, 0.3333333333333333703, 0.3299404806269776169, 0.3333333333333333703, 0.3299404806269776169, 0.3333333333333333703, 0.3299404806269776169, 0.3333333333333333703, 0.3299404806269776169, 0.3333333333333333703, 0.3299404806269776169, 0.3333333333333333703, 0.3299404806269776169, 0.3333333333333333703, 0.3299404806269776169, 0.3333333333333333703, 0.3299404806269776169, 0.3333333333333333703, 0.3299404806269776169, 0.3333333333333333703, 0.3299404806269776169, 0.3333333333333333703, 0.3299404806269776169, 0.3333333333333333703, 0.3299404806269776169, 0.3333333333333333703, 0.3299404806269776169, 0.3333333333333333703, 0.3299404806269776169, 0.3333333333333333703, 0.3299404806269776169, 0.3333333333333333703, 0.3299404806269776169, 0.3333333333333333703, 0.3299404806269776169, 0.3333333333333333703, 0.3299404806269776169, 0.3333333333333333703, 0.3299404806269776169, 0.3333333333333333703, 0.3299404806269776169, 0.3333333333333333703, 0.3299404806269776169, 0.3333333333333333703, 0.3299404806269776169, 0.3333333333333333703, 0.3299404806269776169, 0.3333333333333333703, 0.3299404806269776169, 0.3333333333333333703, 0.3299404806269776169, 0.3333333333333333703, 0.3299404806269776169, 0.3333333333333333703, 0.3299404806269776169, 0.3333333333333333703, 0.3299404806269776169, 0.3333333333333333703, 0.3299404806269776169, 0.3333333333333333703, 0.3299404806269776169, 0.3333333333333333703, 0.3299404806269776169, 0.3333333333333333703, 0.3299404806269776169, 0.3333333333333333703, 0.3299404806269776169, 0.3333333333333333703, 0.3299404806269776169, 0.3333333333333333703, 0.3299404806269776169, 0.3333333333333333703, 0.3299404806269776169, 0.3333333333333333703, 0.3299404806269776169, 0.3333333333333333703, 0.3299404806269776169, 0.3333333333333333703, 0.3299404806269776169, 0.3333333333333333703, 0.3299404806269776169, 0.3333333333333333703, 0.3299404806269776169, 0.3333333333333333703, 0.3299404806269776169, 0.3333333333333333703, 0.3299404806269776169, 0.3333333333333333703, 0.3299404806269776169, 0.3333333333333333703, 0.3299404806269776169, 0.3333333333333333703, 0.3299404806269776169, 0.3333333333333333703, 0.3299404806269776169, 0.3333333333333333703, 0.3299404806269776169, 0.3333333333333333703, 0.3299404806269776169, 0.3333333333333333703, 0.3299404806269776169, 0.3333333333333333703, 0.3299404806269776169, 0.3333333333333333703, 0.3299404806269776169, 0.3333333333333333703, 0.3299404806269776169, 0.3333333333333333703, 0.3299404806269776169, 0.3333333333333333703, 0.3299404806269776169, 0.3333333333333333703, 0.3299404806269776169, 0.3333333333333333703, 0.3299404806269776169, 0.3333333333333333703, 0.3299404806269776169, 0.3333333333333333703, 0.3299404806269776169, 0.3333333333333333703, 0.3299404806269776169, 0.3333333333333333703, 0.3299404806269776169, 0.3333333333333333703, 0.3299404806269776169, 0.3333333333333333703, 0.3299404806269776169, 0.3333333333333333703, 0.3299404806269776169, 0.3333333333333333703, 0.3299404806269776169, 0.3333333333333333703, 0.3299404806269776169, 0.3333333333333333703, 0.3299404806269776169, 0.3333333333333333703, 0.3299404806269776169, 0.3333333333333333703, 0.3299404806269776169, 0.3333333333333333703, 0.3299404806269776169, 0.3333333333333333703, 0.3299404806269776169, 0.3333333333333333703, 0.3299404806269776169, 0.3333333333333333703, 0.3299404806269776169, 0.3333333333333333703, 0.3299404806269776169, 0.3333333333333333703, 0.3299404806269776169, 0.3333333333333333703, 0.3299404806269776169, 0.3333333333333333703, 0.3299404806269776169, 0.3333333333333333703, 0.3299404806269776169, 0.3333333333333333703, 0.3299404806269776169, 0.3333333333333333703, 0.3299404806269776169, 0.3333333333333333703, 0.3299404806269776169, 0.3333333333333333703, 0.3299404806269776169, 0.3333333333333333703, 0.3299404806269776169, 0.3333333333333333703, 0.3299404806269776169, 0.3333333333333333703, 0.3299404806269776169, 0.3333333333333333703, 0.3299404806269776169, 0.3333333333333333703, 0.3299404806269776169, 0.3333333333333333703, 0.3299404806269776169, 0.3333333333333333703, 0.3299404806269776169, 0.3333333333333333703, 0.3299404806269776169, 0.3333333333333333703, 0.3299404806269776169, 0.3333333333333333703, 0.3299404806269776169, 0.3333333333333333703, 0.3299404806269776169, 0.3333333333333333703, 0.3299404806269776169, 0.3333333333333333703, 0.3299404806269776169, 0.3333333333333333703, 0.3299404806269776169, 0.3333333333333333703, 0.3299404806269776169, 0.3333333333333333703, 0.3299404806269776169, 0.3333333333333333703, 0.3299404806269776169, 0.3333333333333333703, 0.3299404806269776169, 0.3333333333333333703, 0.3299404806269776169, 0.3333333333333333703, 0.3299404806269776169, 0.3333333333333333703, 0.3299404806269776169, 0.3333333333333333703, 0.3299404806269776169, 0.3333333333333333703, 0.3299404806269776169, 0.3333333333333333703, 0.3299404806269776169, 0.3333333333333333703, 0.3299404806269776169, 0.3333333333333333703, 0.3299404806269776169, 0.3333333333333333703, 0.3299404806269776169, 0.3333333333333333703, 0.3299404806269776169, 0.3333333333333333703, 0.3299404806269776169, 0.3333333333333333703, 0.3299404806269776169, 0.3333333333333333703, 0.3299404806269776169, 0.3333333333333333703, 0.3299404806269776169, 0.3333333333333333703, 0.3299404806269776169, 0.3333333333333333703, 0.3299404806269776169, 0.3333333333333333703, 0.3299404806269776169, 0.3333333333333333703, 0.3299404806269776169, 0.3333333333333333703, 0.3299404806269776169, 0.3333333333333333703, 0.3299404806269776169, 0.3333333333333333703, 0.3299404806269776169, 0.3333333333333333703, 0.3299404806269776169, 0.3333333333333333703, 0.3299404806269776169, 0.3333333333333333703, 0.3299404806269776169, 0.3333333333333333703, 0.3299404806269776169, 0.3333333333333333703, 0.3299404806269776169, 0.3333333333333333703, 0.3299404806269776169, 0.3333333333333333703, 0.3299404806269776169, 0.3333333333333333703, 0.3299404806269776169, 0.3333333333333333703, 0.3299404806269776169, 0.3333333333333333703, 0.3299404806269776169, 0.3333333333333333703, 0.3299404806269776169, 0.3333333333333333703, 0.3299404806269776169, 0.3333333333333333703, 0.3299404806269776169, 0.3333333333333333703, 0.3299404806269776169, 0.3333333333333333703, 0.3299404806269776169, 0.3333333333333333703, 0.3299404806269776169, 0.3333333333333333703, 0.3299404806269776169, 0.3333333333333333703, 0.3299404806269776169, 0.3333333333333333703, 0.3299404806269776169, 0.3333333333333333703, 0.3299404806269776169, 0.3333333333333333703, 0.3299404806269776169, 0.3333333333333333703, 0.3299404806269776169, 0.3333333333333333703, 0.3299404806269776169, 0.3333333333333333703, 0.3299404806269776169, 0.3333333333333333703, 0.3299404806269776169, 0.3333333333333333703, 0.3299404806269776169, 0.3333333333333333703, 0.3299404806269776169, 0.3333333333333333703, 0.3299404806269776169, 0.3333333333333333703, 0.3299404806269776169, 0.3333333333333333703, 0.3299404806269776169, 0.3333333333333333703, 0.3299404806269776169, 0.3333333333333333703, 0.3299404806269776169, 0.3333333333333333703, 0.3299404806269776169, 0.3333333333333333703, 0.3299404806269776169, 0.3333333333333333703, 0.3299404806269776169, 0.3333333333333333703, 0.3299404806269776169, 0.3333333333333333703, 0.3299404806269776169, 0.3333333333333333703, 0.3299404806269776169, 0.3333333333333333703, 0.3299404806269776169, 0.3333333333333333703, 0.3299404806269776169, 0.3333333333333333703, 0.3299404806269776169, 0.3333333333333333703, 0.3299404806269776169, 0.3333333333333333703, 0.3299404806269776169, 0.3333333333333333703, 0.3299404806269776169, 0.3333333333333333703, 0.3299404806269776169, 0.3333333333333333703, 0.3299404806269776169, 0.3333333333333333703, 0.3299404806269776169, 0.3333333333333333703, 0.3299404806269776169, 0.3333333333333333703, 0.3299404806269776169, 0.3333333333333333703, 0.3299404806269776169, 0.3333333333333333703, 0.3299404806269776169, 0.3333333333333333703, 0.3299404806269776169, 0.3333333333333333703, 0.3299404806269776169, 0.3333333333333333703, 0.3299404806269776169, 0.3333333333333333703, 0.3299404806269776169, 0.3333333333333333703, 0.3299404806269776169, 0.3333333333333333703, 0.3299404806269776169, 0.3333333333333333703, 0.3299404806269776169, 0.3333333333333333703, 0.3299404806269776169, 0.3333333333333333703, 0.3299404806269776169, 0.3333333333333333703, 0.3299404806269776169, 0.3333333333333333703, 0.3299404806269776169, 0.3333333333333333703, 0.3299404806269776169, 0.3333333333333333703, 0.3299404806269776169, 0.3333333333333333703, 0.3299404806269776169, 0.3333333333333333703, 0.3299404806269776169, 0.3333333333333333703, 0.3299404806269776169, 0.3333333333333333703, 0.3299404806269776169, 0.3333333333333333703, 0.3320603117974822438, 0.3317425830320511193),
 ( 1.000000000000000000, 0.9898214418809326842, 1.000000000000000000, 0.9898214418809326842, 1.000000000000000000, 0.9898214418809326842, 1.000000000000000000, 0.9898214418809326842, 1.000000000000000000, 0.9898214418809326842, 1.000000000000000000, 0.9898214418809326842, 1.000000000000000000, 0.9898214418809326842, 1.000000000000000000, 0.9898214418809326842, 1.000000000000000000, 0.9898214418809326842, 1.000000000000000000, 0.9898214418809326842, 1.000000000000000000, 0.9898214418809326842, 1.000000000000000000, 0.9898214418809326842, 1.000000000000000000, 0.9898214418809326842, 1.000000000000000000, 0.9898214418809326842, 1.000000000000000000, 0.9898214418809326842, 1.000000000000000000, 0.9898214418809326842, 1.000000000000000000, 0.9898214418809326842, 1.000000000000000000, 0.9898214418809326842, 1.000000000000000000, 0.9898214418809326842, 1.000000000000000000, 0.9898214418809326842, 1.000000000000000000, 0.9898214418809326842, 1.000000000000000000, 0.9898214418809326842, 1.000000000000000000, 0.9898214418809326842, 1.000000000000000000, 0.9898214418809326842, 1.000000000000000000, 0.9898214418809326842, 1.000000000000000000, 0.9898214418809326842, 1.000000000000000000, 0.9898214418809326842, 1.000000000000000000, 0.9898214418809326842, 1.000000000000000000, 0.9898214418809326842, 1.000000000000000000, 0.9898214418809326842, 1.000000000000000000, 0.9898214418809326842, 1.000000000000000000, 0.9898214418809326842, 1.000000000000000000, 0.9898214418809326842, 1.000000000000000000, 0.9898214418809326842, 1.000000000000000000, 0.9898214418809326842, 1.000000000000000000, 0.9898214418809326842, 1.000000000000000000, 0.9898214418809326842, 1.000000000000000000, 0.9898214418809326842, 1.000000000000000000, 0.9898214418809326842, 1.000000000000000000, 0.9898214418809326842, 1.000000000000000000, 0.9898214418809326842, 1.000000000000000000, 0.9898214418809326842, 1.000000000000000000, 0.9898214418809326842, 1.000000000000000000, 0.9898214418809326842, 1.000000000000000000, 0.9898214418809326842, 1.000000000000000000, 0.9898214418809326842, 1.000000000000000000, 0.9898214418809326842, 1.000000000000000000, 0.9898214418809326842, 1.000000000000000000, 0.9898214418809326842, 1.000000000000000000, 0.9898214418809326842, 1.000000000000000000, 0.9898214418809326842, 1.000000000000000000, 0.9898214418809326842, 1.000000000000000000, 0.9898214418809326842, 1.000000000000000000, 0.9898214418809326842, 1.000000000000000000, 0.9898214418809326842, 1.000000000000000000, 0.9898214418809326842, 1.000000000000000000, 0.9898214418809326842, 1.000000000000000000, 0.9898214418809326842, 1.000000000000000000, 0.9898214418809326842, 1.000000000000000000, 0.9898214418809326842, 1.000000000000000000, 0.9898214418809326842, 1.000000000000000000, 0.9898214418809326842, 1.000000000000000000, 0.9898214418809326842, 1.000000000000000000, 0.9898214418809326842, 1.000000000000000000, 0.9898214418809326842, 1.000000000000000000, 0.9898214418809326842, 1.000000000000000000, 0.9898214418809326842, 1.000000000000000000, 0.9898214418809326842, 1.000000000000000000, 0.9898214418809326842, 1.000000000000000000, 0.9898214418809326842, 1.000000000000000000, 0.9898214418809326842, 1.000000000000000000, 0.9898214418809326842, 1.000000000000000000, 0.9898214418809326842, 1.000000000000000000, 0.9898214418809326842, 1.000000000000000000, 0.9898214418809326842, 1.000000000000000000, 0.9898214418809326842, 1.000000000000000000, 0.9898214418809326842, 1.000000000000000000, 0.9898214418809326842, 1.000000000000000000, 0.9898214418809326842, 1.000000000000000000, 0.9898214418809326842, 1.000000000000000000, 0.9898214418809326842, 1.000000000000000000, 0.9898214418809326842, 1.000000000000000000, 0.9898214418809326842, 1.000000000000000000, 0.9898214418809326842, 1.000000000000000000, 0.9898214418809326842, 1.000000000000000000, 0.9898214418809326842, 1.000000000000000000, 0.9898214418809326842, 1.000000000000000000, 0.9898214418809326842, 1.000000000000000000, 0.9898214418809326842, 1.000000000000000000, 0.9898214418809326842, 1.000000000000000000, 0.9898214418809326842, 1.000000000000000000, 0.9898214418809326842, 1.000000000000000000, 0.9898214418809326842, 1.000000000000000000, 0.9898214418809326842, 1.000000000000000000, 0.9898214418809326842, 1.000000000000000000, 0.9898214418809326842, 1.000000000000000000, 0.9898214418809326842, 1.000000000000000000, 0.9898214418809326842, 1.000000000000000000, 0.9898214418809326842, 1.000000000000000000, 0.9898214418809326842, 1.000000000000000000, 0.9898214418809326842, 1.000000000000000000, 0.9898214418809326842, 1.000000000000000000, 0.9898214418809326842, 1.000000000000000000, 0.9898214418809326842, 1.000000000000000000, 0.9898214418809326842, 1.000000000000000000, 0.9898214418809326842, 1.000000000000000000, 0.9898214418809326842, 1.000000000000000000, 0.9898214418809326842, 1.000000000000000000, 0.9898214418809326842, 1.000000000000000000, 0.9898214418809326842, 1.000000000000000000, 0.9898214418809326842, 1.000000000000000000, 0.9898214418809326842, 1.000000000000000000, 0.9898214418809326842, 1.000000000000000000, 0.9898214418809326842, 1.000000000000000000, 0.9898214418809326842, 1.000000000000000000, 0.9898214418809326842, 1.000000000000000000, 0.9898214418809326842, 1.000000000000000000, 0.9898214418809326842, 1.000000000000000000, 0.9898214418809326842, 1.000000000000000000, 0.9898214418809326842, 1.000000000000000000, 0.9898214418809326842, 1.000000000000000000, 0.9898214418809326842, 1.000000000000000000, 0.9898214418809326842, 1.000000000000000000, 0.9898214418809326842, 1.000000000000000000, 0.9898214418809326842, 1.000000000000000000, 0.9898214418809326842, 1.000000000000000000, 0.9898214418809326842, 1.000000000000000000, 0.9898214418809326842, 1.000000000000000000, 0.9898214418809326842, 1.000000000000000000, 0.9898214418809326842, 1.000000000000000000, 0.9898214418809326842, 1.000000000000000000, 0.9898214418809326842, 1.000000000000000000, 0.9898214418809326842, 1.000000000000000000, 0.9898214418809326842, 1.000000000000000000, 0.9898214418809326842, 1.000000000000000000, 0.9898214418809326842, 1.000000000000000000, 0.9898214418809326842, 1.000000000000000000, 0.9898214418809326842, 1.000000000000000000, 0.9898214418809326842, 1.000000000000000000, 0.9898214418809326842, 1.000000000000000000, 0.9898214418809326842, 1.000000000000000000, 0.9898214418809326842, 1.000000000000000000, 0.9898214418809326842, 1.000000000000000000, 0.9898214418809326842, 1.000000000000000000, 0.9898214418809326842, 1.000000000000000000, 0.9898214418809326842, 1.000000000000000000, 0.9898214418809326842, 1.000000000000000000, 0.9898214418809326842, 1.000000000000000000, 0.9898214418809326842, 1.000000000000000000, 0.9898214418809326842, 1.000000000000000000, 0.9898214418809326842, 1.000000000000000000, 0.9898214418809326842, 1.000000000000000000, 0.9898214418809326842, 1.000000000000000000, 0.9898214418809326842, 1.000000000000000000, 0.9898214418809326842, 1.000000000000000000, 0.9898214418809326842, 1.000000000000000000, 0.9898214418809326842, 1.000000000000000000, 0.9898214418809326842, 1.000000000000000000, 0.9898214418809326842, 1.000000000000000000, 0.9898214418809326842, 1.000000000000000000, 0.9898214418809326842, 1.000000000000000000, 0.9898214418809326842, 1.000000000000000000, 0.9898214418809326842, 1.000000000000000000, 0.9898214418809326842, 1.000000000000000000, 0.9898214418809326842, 1.000000000000000000, 0.9898214418809326842, 1.000000000000000000, 0.9898214418809326842, 1.000000000000000000, 0.9898214418809326842, 1.000000000000000000, 0.9898214418809326842, 1.000000000000000000, 0.9898214418809326842, 1.000000000000000000, 0.9898214418809326842, 1.000000000000000000, 0.9898214418809326842, 1.000000000000000000, 0.9898214418809326842, 1.000000000000000000, 0.9898214418809326842, 1.000000000000000000, 0.9898214418809326842, 1.000000000000000000, 0.9898214418809326842, 1.000000000000000000, 0.9898214418809326842, 1.000000000000000000, 0.9898214418809326842, 1.000000000000000000, 0.9898214418809326842, 1.000000000000000000, 0.9898214418809326842, 1.000000000000000000, 0.9898214418809326842, 1.000000000000000000, 0.9898214418809326842, 1.000000000000000000, 0.9898214418809326842, 1.000000000000000000, 0.9898214418809326842, 1.000000000000000000, 0.9898214418809326842, 1.000000000000000000, 0.9898214418809326842, 1.000000000000000000, 0.9898214418809326842, 1.000000000000000000, 0.9898214418809326842, 1.000000000000000000, 0.9898214418809326842, 1.000000000000000000, 0.9898214418809326842, 1.000000000000000000, 0.9898214418809326842, 1.000000000000000000, 0.9898214418809326842, 1.000000000000000000, 0.9898214418809326842, 1.000000000000000000, 0.9898214418809326842, 1.000000000000000000, 0.9898214418809326842, 1.000000000000000000, 0.9898214418809326842, 1.000000000000000000, 0.9898214418809326842, 1.000000000000000000, 0.9898214418809326842, 1.000000000000000000, 0.9898214418809326842, 1.000000000000000000, 0.9898214418809326842, 1.000000000000000000, 0.9898214418809326842, 1.000000000000000000, 0.9898214418809326842, 1.000000000000000000, 0.9898214418809326842, 1.000000000000000000, 0.9898214418809326842, 1.000000000000000000, 0.9898214418809326842, 1.000000000000000000, 0.9898214418809326842, 1.000000000000000000, 0.9898214418809326842, 1.000000000000000000, 0.9898214418809326842, 1.000000000000000000, 0.9898214418809326842, 1.000000000000000000, 0.9898214418809326842, 1.000000000000000000, 0.9898214418809326842, 1.000000000000000000, 0.9898214418809326842, 1.000000000000000000, 0.9898214418809326842, 1.000000000000000000, 0.9898214418809326842, 1.000000000000000000, 0.9898214418809326842, 1.000000000000000000, 0.9898214418809326842, 1.000000000000000000, 0.9898214418809326842, 1.000000000000000000, 0.9898214418809326842, 1.000000000000000000, 0.9898214418809326842, 1.000000000000000000, 0.9898214418809326842, 1.000000000000000000, 0.9898214418809326842, 1.000000000000000000, 0.9898214418809326842, 1.000000000000000000, 0.9898214418809326842, 1.000000000000000000, 0.9898214418809326842, 1.000000000000000000, 0.9898214418809326842, 1.000000000000000000, 0.9898214418809326842, 1.000000000000000000, 0.9898214418809326842, 1.000000000000000000, 0.9898214418809326842, 1.000000000000000000, 0.9898214418809326842, 1.000000000000000000, 0.9898214418809326842, 1.000000000000000000, 0.9898214418809326842, 1.000000000000000000, 0.9898214418809326842, 1.000000000000000000, 0.9898214418809326842, 1.000000000000000000, 0.9898214418809326842, 1.000000000000000000, 0.9898214418809326842, 1.000000000000000000, 0.9898214418809326842, 1.000000000000000000, 0.9898214418809326842, 1.000000000000000000, 0.9898214418809326842, 1.000000000000000000, 0.9898214418809326842, 1.000000000000000000, 0.9898214418809326842, 1.000000000000000000, 0.9898214418809326842, 1.000000000000000000, 0.9898214418809326842, 1.000000000000000000, 0.9898214418809326842, 1.000000000000000000, 0.9898214418809326842, 1.000000000000000000, 0.9898214418809326842, 1.000000000000000000, 0.9898214418809326842, 1.000000000000000000, 0.9898214418809326842, 1.000000000000000000, 0.9898214418809326842, 1.000000000000000000, 0.9898214418809326842, 1.000000000000000000, 0.9898214418809326842, 1.000000000000000000, 0.9898214418809326842, 1.000000000000000000, 0.9898214418809326842, 1.000000000000000000, 0.9898214418809326842, 1.000000000000000000, 0.9898214418809326842, 1.000000000000000000, 0.9898214418809326842, 1.000000000000000000, 0.9898214418809326842, 1.000000000000000000, 0.9898214418809326842, 1.000000000000000000, 0.9898214418809326842, 1.000000000000000000, 0.9898214418809326842, 1.000000000000000000, 0.9898214418809326842, 1.000000000000000000, 0.9898214418809326842, 1.000000000000000000, 0.9898214418809326842, 1.000000000000000000, 0.9898214418809326842, 1.000000000000000000, 0.9898214418809326842, 1.000000000000000000, 0.9898214418809326842, 1.000000000000000000, 0.9898214418809326842, 1.000000000000000000, 0.9898214418809326842, 1.000000000000000000, 0.9898214418809326842, 1.000000000000000000, 0.9898214418809326842, 1.000000000000000000, 0.9898214418809326842, 1.000000000000000000, 0.9898214418809326842, 1.000000000000000000, 0.9898214418809326842, 1.000000000000000000, 0.9898214418809326842, 1.000000000000000000, 0.9898214418809326842, 1.000000000000000000, 0.9898214418809326842, 1.000000000000000000, 0.9898214418809326842, 1.000000000000000000, 0.9898214418809326842, 1.000000000000000000, 0.9898214418809326842, 1.000000000000000000, 0.9898214418809326842, 1.000000000000000000, 0.9898214418809326842, 1.000000000000000000, 0.9898214418809326842, 1.000000000000000000, 0.9898214418809326842, 1.000000000000000000, 0.9898214418809326842, 1.000000000000000000, 0.9898214418809326842, 1.000000000000000000, 0.9898214418809326842, 1.000000000000000000, 0.9898214418809326842, 1.000000000000000000, 0.9898214418809326842, 1.000000000000000000, 0.9898214418809326842, 1.000000000000000000, 0.9898214418809326842, 1.000000000000000000, 0.9898214418809326842, 1.000000000000000000, 0.9898214418809326842, 1.000000000000000000, 0.9898214418809326842, 1.000000000000000000, 0.9898214418809326842, 1.000000000000000000, 0.9898214418809326842, 1.000000000000000000, 0.9898214418809326842, 1.000000000000000000, 0.9898214418809326842, 1.000000000000000000, 0.9898214418809326842, 1.000000000000000000, 0.9898214418809326842, 1.000000000000000000, 0.9898214418809326842, 1.000000000000000000, 0.9898214418809326842, 1.000000000000000000, 0.9898214418809326842, 1.000000000000000000, 0.9898214418809326842, 1.000000000000000000, 0.9898214418809326842, 1.000000000000000000, 0.9898214418809326842, 1.000000000000000000, 0.9898214418809326842, 1.000000000000000000, 0.9898214418809326842, 1.000000000000000000, 0.9898214418809326842, 1.000000000000000000, 0.9898214418809326842, 1.000000000000000000, 0.9898214418809326842, 1.000000000000000000, 0.9898214418809326842, 1.000000000000000000, 0.9898214418809326842, 1.000000000000000000, 0.9898214418809326842, 1.000000000000000000, 0.9898214418809326842, 1.000000000000000000, 0.9898214418809326842, 1.000000000000000000, 0.9898214418809326842, 1.000000000000000000, 0.9898214418809326842, 1.000000000000000000, 0.9898214418809326842, 1.000000000000000000, 0.9898214418809326842, 1.000000000000000000, 0.9898214418809326842, 1.000000000000000000, 0.9898214418809326842, 1.000000000000000000, 0.9898214418809326842, 1.000000000000000000, 0.9898214418809326842, 1.000000000000000000, 0.9898214418809326842, 1.000000000000000000, 0.9898214418809326842, 1.000000000000000000, 0.9898214418809326842, 1.000000000000000000, 0.9898214418809326842, 1.000000000000000000, 0.9898214418809326842, 1.000000000000000000, 0.9898214418809326842, 1.000000000000000000, 0.9898214418809326842, 1.000000000000000000, 0.9898214418809326842, 1.000000000000000000, 0.9898214418809326842, 1.000000000000000000, 0.9898214418809326842, 1.000000000000000000, 0.9898214418809326842, 1.000000000000000000, 0.9898214418809326842, 1.000000000000000000, 0.9898214418809326842, 1.000000000000000000, 0.9898214418809326842, 1.000000000000000000, 0.9898214418809326842, 1.000000000000000000, 0.9898214418809326842, 1.000000000000000000, 0.9898214418809326842, 1.000000000000000000, 0.9898214418809326842, 1.000000000000000000, 0.9898214418809326842, 1.000000000000000000, 0.9898214418809326842, 1.000000000000000000, 0.9898214418809326842, 1.000000000000000000, 0.9898214418809326842, 1.000000000000000000, 0.9898214418809326842, 1.000000000000000000, 0.9898214418809326842, 1.000000000000000000, 0.9898214418809326842, 1.000000000000000000, 0.9898214418809326842, 1.000000000000000000, 0.9898214418809326842, 1.000000000000000000, 0.9898214418809326842, 1.000000000000000000, 0.9898214418809326842, 1.000000000000000000, 0.9898214418809326842, 1.000000000000000000, 0.9898214418809326842, 1.000000000000000000, 0.9898214418809326842, 1.000000000000000000, 0.9898214418809326842, 1.000000000000000000, 0.9898214418809326842, 1.000000000000000000, 0.9898214418809326842, 1.000000000000000000, 0.9898214418809326842, 1.000000000000000000, 0.9898214418809326842, 1.000000000000000000, 0.9898214418809326842, 1.000000000000000000, 0.9898214418809326842, 1.000000000000000000, 0.9898214418809326842, 1.000000000000000000, 0.9898214418809326842, 1.000000000000000000, 0.9898214418809326842, 1.000000000000000000, 0.9898214418809326842, 1.000000000000000000, 0.9898214418809326842, 1.000000000000000000, 0.9898214418809326842, 1.000000000000000000, 0.9898214418809326842, 1.000000000000000000, 0.9898214418809326842, 1.000000000000000000, 0.9898214418809326842, 1.000000000000000000, 0.9898214418809326842, 1.000000000000000000, 0.9898214418809326842, 1.000000000000000000, 0.9898214418809326842, 1.000000000000000000, 0.9898214418809326842, 1.000000000000000000, 0.9898214418809326842, 1.000000000000000000, 0.9898214418809326842, 1.000000000000000000, 0.9898214418809326842, 1.000000000000000000, 0.9898214418809326842, 1.000000000000000000, 0.9898214418809326842, 1.000000000000000000, 0.9898214418809326842, 1.000000000000000000, 0.9898214418809326842, 1.000000000000000000, 0.9898214418809326842, 1.000000000000000000, 0.9898214418809326842, 1.000000000000000000, 0.9898214418809326842, 1.000000000000000000, 0.9898214418809326842, 1.000000000000000000, 0.9898214418809326842, 1.000000000000000000, 0.9898214418809326842, 1.000000000000000000, 0.9898214418809326842, 1.000000000000000000, 0.9898214418809326842, 1.000000000000000000, 0.9898214418809326842, 1.000000000000000000, 0.9898214418809326842, 1.000000000000000000, 0.9898214418809326842, 1.000000000000000000, 0.9898214418809326842, 1.000000000000000000, 0.9898214418809326842, 1.000000000000000000, 0.9898214418809326842, 1.000000000000000000, 0.9898214418809326842, 1.000000000000000000, 0.9898214418809326842, 1.000000000000000000, 0.9898214418809326842, 1.000000000000000000, 0.9898214418809326842, 1.000000000000000000, 0.9898214418809326842, 1.000000000000000000, 0.9898214418809326842, 1.000000000000000000, 0.9898214418809326842, 1.000000000000000000, 0.9898214418809326842, 1.000000000000000000, 0.9898214418809326842, 1.000000000000000000, 0.9898214418809326842, 1.000000000000000000, 0.9898214418809326842, 1.000000000000000000, 0.9898214418809326842, 1.000000000000000000, 0.9898214418809326842, 1.000000000000000000, 0.9898214418809326842, 1.000000000000000000, 0.9898214418809326842, 1.000000000000000000, 0.9898214418809326842, 1.000000000000000000, 0.9898214418809326842, 1.000000000000000000, 0.9898214418809326842, 1.000000000000000000, 0.9898214418809326842, 1.000000000000000000, 0.9898214418809326842, 1.000000000000000000, 0.9898214418809326842, 1.000000000000000000, 0.9898214418809326842, 1.000000000000000000, 0.9898214418809326842, 1.000000000000000000, 0.9898214418809326842, 1.000000000000000000, 0.9898214418809326842, 1.000000000000000000, 0.9898214418809326842, 1.000000000000000000, 0.9898214418809326842, 1.000000000000000000, 0.9898214418809326842, 1.000000000000000000, 0.9898214418809326842, 1.000000000000000000, 0.9898214418809326842, 1.000000000000000000, 0.9898214418809326842, 1.000000000000000000, 0.9898214418809326842, 1.000000000000000000, 0.9898214418809326842, 1.000000000000000000, 0.9898214418809326842, 1.000000000000000000, 0.9898214418809326842, 1.000000000000000000, 0.9961809353924466759, 0.9952277490961531914),
 ( 0.3333333333333333703, 0.3299404806269776169, 0.3333333333333333703, 0.3299404806269776169, 0.3333333333333333703, 0.3299404806269776169, 0.3333333333333333703, 0.3299404806269776169, 0.3333333333333333703, 0.3299404806269776169, 0.3333333333333333703, 0.3299404806269776169, 0.3333333333333333703, 0.3299404806269776169, 0.3333333333333333703, 0.3299404806269776169, 0.3333333333333333703, 0.3299404806269776169, 0.3333333333333333703, 0.3299404806269776169, 0.3333333333333333703, 0.3299404806269776169, 0.3333333333333333703, 0.3299404806269776169, 0.3333333333333333703, 0.3299404806269776169, 0.3333333333333333703, 0.3299404806269776169, 0.3333333333333333703, 0.3299404806269776169, 0.3333333333333333703, 0.3299404806269776169, 0.3333333333333333703, 0.3299404806269776169, 0.3333333333333333703, 0.3299404806269776169, 0.3333333333333333703, 0.3299404806269776169, 0.3333333333333333703, 0.3299404806269776169, 0.3333333333333333703, 0.3299404806269776169, 0.3333333333333333703, 0.3299404806269776169, 0.3333333333333333703, 0.3299404806269776169, 0.3333333333333333703, 0.3299404806269776169, 0.3333333333333333703, 0.3299404806269776169, 0.3333333333333333703, 0.3299404806269776169, 0.3333333333333333703, 0.3299404806269776169, 0.3333333333333333703, 0.3299404806269776169, 0.3333333333333333703, 0.3299404806269776169, 0.3333333333333333703, 0.3299404806269776169, 0.3333333333333333703, 0.3299404806269776169, 0.3333333333333333703, 0.3299404806269776169, 0.3333333333333333703, 0.3299404806269776169, 0.3333333333333333703, 0.3299404806269776169, 0.3333333333333333703, 0.3299404806269776169, 0.3333333333333333703, 0.3299404806269776169, 0.3333333333333333703, 0.3299404806269776169, 0.3333333333333333703, 0.3299404806269776169, 0.3333333333333333703, 0.3299404806269776169, 0.3333333333333333703, 0.3299404806269776169, 0.3333333333333333703, 0.3299404806269776169, 0.3333333333333333703, 0.3299404806269776169, 0.3333333333333333703, 0.3299404806269776169, 0.3333333333333333703, 0.3299404806269776169, 0.3333333333333333703, 0.3299404806269776169, 0.3333333333333333703, 0.3299404806269776169, 0.3333333333333333703, 0.3299404806269776169, 0.3333333333333333703, 0.3299404806269776169, 0.3333333333333333703, 0.3299404806269776169, 0.3333333333333333703, 0.3299404806269776169, 0.3333333333333333703, 0.3299404806269776169, 0.3333333333333333703, 0.3299404806269776169, 0.3333333333333333703, 0.3299404806269776169, 0.3333333333333333703, 0.3299404806269776169, 0.3333333333333333703, 0.3299404806269776169, 0.3333333333333333703, 0.3299404806269776169, 0.3333333333333333703, 0.3299404806269776169, 0.3333333333333333703, 0.3299404806269776169, 0.3333333333333333703, 0.3299404806269776169, 0.3333333333333333703, 0.3299404806269776169, 0.3333333333333333703, 0.3299404806269776169, 0.3333333333333333703, 0.3299404806269776169, 0.3333333333333333703, 0.3299404806269776169, 0.3333333333333333703, 0.3299404806269776169, 0.3333333333333333703, 0.3299404806269776169, 0.3333333333333333703, 0.3299404806269776169, 0.3333333333333333703, 0.3299404806269776169, 0.3333333333333333703, 0.3299404806269776169, 0.3333333333333333703, 0.3299404806269776169, 0.3333333333333333703, 0.3299404806269776169, 0.3333333333333333703, 0.3299404806269776169, 0.3333333333333333703, 0.3299404806269776169, 0.3333333333333333703, 0.3299404806269776169, 0.3333333333333333703, 0.3299404806269776169, 0.3333333333333333703, 0.3299404806269776169, 0.3333333333333333703, 0.3299404806269776169, 0.3333333333333333703, 0.3299404806269776169, 0.3333333333333333703, 0.3299404806269776169, 0.3333333333333333703, 0.3299404806269776169, 0.3333333333333333703, 0.3299404806269776169, 0.3333333333333333703, 0.3299404806269776169, 0.3333333333333333703, 0.3299404806269776169, 0.3333333333333333703, 0.3299404806269776169, 0.3333333333333333703, 0.3299404806269776169, 0.3333333333333333703, 0.3299404806269776169, 0.3333333333333333703, 0.3299404806269776169, 0.3333333333333333703, 0.3299404806269776169, 0.3333333333333333703, 0.3299404806269776169, 0.3333333333333333703, 0.3299404806269776169, 0.3333333333333333703, 0.3299404806269776169, 0.3333333333333333703, 0.3299404806269776169, 0.3333333333333333703, 0.3299404806269776169, 0.3333333333333333703, 0.3299404806269776169, 0.3333333333333333703, 0.3299404806269776169, 0.3333333333333333703, 0.3299404806269776169, 0.3333333333333333703, 0.3299404806269776169, 0.3333333333333333703, 0.3299404806269776169, 0.3333333333333333703, 0.3299404806269776169, 0.3333333333333333703, 0.3299404806269776169, 0.3333333333333333703, 0.3299404806269776169, 0.3333333333333333703, 0.3299404806269776169, 0.3333333333333333703, 0.3299404806269776169, 0.3333333333333333703, 0.3299404806269776169, 0.3333333333333333703, 0.3299404806269776169, 0.3333333333333333703, 0.3299404806269776169, 0.3333333333333333703, 0.3299404806269776169, 0.3333333333333333703, 0.3299404806269776169, 0.3333333333333333703, 0.3299404806269776169, 0.3333333333333333703, 0.3299404806269776169, 0.3333333333333333703, 0.3299404806269776169, 0.3333333333333333703, 0.3299404806269776169, 0.3333333333333333703, 0.3299404806269776169, 0.3333333333333333703, 0.3299404806269776169, 0.3333333333333333703, 0.3299404806269776169, 0.3333333333333333703, 0.3299404806269776169, 0.3333333333333333703, 0.3299404806269776169, 0.3333333333333333703, 0.3299404806269776169, 0.3333333333333333703, 0.3299404806269776169, 0.3333333333333333703, 0.3299404806269776169, 0.3333333333333333703, 0.3299404806269776169, 0.3333333333333333703, 0.3299404806269776169, 0.3333333333333333703, 0.3299404806269776169, 0.3333333333333333703, 0.3299404806269776169, 0.3333333333333333703, 0.3299404806269776169, 0.3333333333333333703, 0.3299404806269776169, 0.3333333333333333703, 0.3299404806269776169, 0.3333333333333333703, 0.3299404806269776169, 0.3333333333333333703, 0.3299404806269776169, 0.3333333333333333703, 0.3299404806269776169, 0.3333333333333333703, 0.3299404806269776169, 0.3333333333333333703, 0.3299404806269776169, 0.3333333333333333703, 0.3299404806269776169, 0.3333333333333333703, 0.3299404806269776169, 0.3333333333333333703, 0.3299404806269776169, 0.3333333333333333703, 0.3299404806269776169, 0.3333333333333333703, 0.3299404806269776169, 0.3333333333333333703, 0.3299404806269776169, 0.3333333333333333703, 0.3299404806269776169, 0.3333333333333333703, 0.3299404806269776169, 0.3333333333333333703, 0.3299404806269776169, 0.3333333333333333703, 0.3299404806269776169, 0.3333333333333333703, 0.3299404806269776169, 0.3333333333333333703, 0.3299404806269776169, 0.3333333333333333703, 0.3299404806269776169, 0.3333333333333333703, 0.3299404806269776169, 0.3333333333333333703, 0.3299404806269776169, 0.3333333333333333703, 0.3299404806269776169, 0.3333333333333333703, 0.3299404806269776169, 0.3333333333333333703, 0.3299404806269776169, 0.3333333333333333703, 0.3299404806269776169, 0.3333333333333333703, 0.3299404806269776169, 0.3333333333333333703, 0.3299404806269776169, 0.3333333333333333703, 0.3299404806269776169, 0.3333333333333333703, 0.3299404806269776169, 0.3333333333333333703, 0.3299404806269776169, 0.3333333333333333703, 0.3299404806269776169, 0.3333333333333333703, 0.3299404806269776169, 0.3333333333333333703, 0.3299404806269776169, 0.3333333333333333703, 0.3299404806269776169, 0.3333333333333333703, 0.3299404806269776169, 0.3333333333333333703, 0.3299404806269776169, 0.3333333333333333703, 0.3299404806269776169, 0.3333333333333333703, 0.3299404806269776169, 0.3333333333333333703, 0.3299404806269776169, 0.3333333333333333703, 0.3299404806269776169, 0.3333333333333333703, 0.3299404806269776169, 0.3333333333333333703, 0.3299404806269776169, 0.3333333333333333703, 0.3299404806269776169, 0.3333333333333333703, 0.3299404806269776169, 0.3333333333333333703, 0.3299404806269776169, 0.3333333333333333703, 0.3299404806269776169, 0.3333333333333333703, 0.3299404806269776169, 0.3333333333333333703, 0.3299404806269776169, 0.3333333333333333703, 0.3299404806269776169, 0.3333333333333333703, 0.3299404806269776169, 0.3333333333333333703, 0.3299404806269776169, 0.3333333333333333703, 0.3299404806269776169, 0.3333333333333333703, 0.3299404806269776169, 0.3333333333333333703, 0.3299404806269776169, 0.3333333333333333703, 0.3299404806269776169, 0.3333333333333333703, 0.3299404806269776169, 0.3333333333333333703, 0.3299404806269776169, 0.3333333333333333703, 0.3299404806269776169, 0.3333333333333333703, 0.3299404806269776169, 0.3333333333333333703, 0.3299404806269776169, 0.3333333333333333703, 0.3299404806269776169, 0.3333333333333333703, 0.3299404806269776169, 0.3333333333333333703, 0.3299404806269776169, 0.3333333333333333703, 0.3299404806269776169, 0.3333333333333333703, 0.3299404806269776169, 0.3333333333333333703, 0.3299404806269776169, 0.3333333333333333703, 0.3299404806269776169, 0.3333333333333333703, 0.3299404806269776169, 0.3333333333333333703, 0.3299404806269776169, 0.3333333333333333703, 0.3299404806269776169, 0.3333333333333333703, 0.3299404806269776169, 0.3333333333333333703, 0.3299404806269776169, 0.3333333333333333703, 0.3299404806269776169, 0.3333333333333333703, 0.3299404806269776169, 0.3333333333333333703, 0.3299404806269776169, 0.3333333333333333703, 0.3299404806269776169, 0.3333333333333333703, 0.3299404806269776169, 0.3333333333333333703, 0.3299404806269776169, 0.3333333333333333703, 0.3299404806269776169, 0.3333333333333333703, 0.3299404806269776169, 0.3333333333333333703, 0.3299404806269776169, 0.3333333333333333703, 0.3299404806269776169, 0.3333333333333333703, 0.3299404806269776169, 0.3333333333333333703, 0.3299404806269776169, 0.3333333333333333703, 0.3299404806269776169, 0.3333333333333333703, 0.3299404806269776169, 0.3333333333333333703, 0.3299404806269776169, 0.3333333333333333703, 0.3299404806269776169, 0.3333333333333333703, 0.3299404806269776169, 0.3333333333333333703, 0.3299404806269776169, 0.3333333333333333703, 0.3299404806269776169, 0.3333333333333333703, 0.3299404806269776169, 0.3333333333333333703, 0.3299404806269776169, 0.3333333333333333703, 0.3299404806269776169, 0.3333333333333333703, 0.3299404806269776169, 0.3333333333333333703, 0.3299404806269776169, 0.3333333333333333703, 0.3299404806269776169, 0.3333333333333333703, 0.3299404806269776169, 0.3333333333333333703, 0.3299404806269776169, 0.3333333333333333703, 0.3299404806269776169, 0.3333333333333333703, 0.3299404806269776169, 0.3333333333333333703, 0.3299404806269776169, 0.3333333333333333703, 0.3299404806269776169, 0.3333333333333333703, 0.3299404806269776169, 0.3333333333333333703, 0.3299404806269776169, 0.3333333333333333703, 0.3299404806269776169, 0.3333333333333333703, 0.3299404806269776169, 0.3333333333333333703, 0.3299404806269776169, 0.3333333333333333703, 0.3299404806269776169, 0.3333333333333333703, 0.3299404806269776169, 0.3333333333333333703, 0.3299404806269776169, 0.3333333333333333703, 0.3299404806269776169, 0.3333333333333333703, 0.3299404806269776169, 0.3333333333333333703, 0.3299404806269776169, 0.3333333333333333703, 0.3299404806269776169, 0.3333333333333333703, 0.3299404806269776169, 0.3333333333333333703, 0.3299404806269776169, 0.3333333333333333703, 0.3299404806269776169, 0.3333333333333333703, 0.3299404806269776169, 0.3333333333333333703, 0.3299404806269776169, 0.3333333333333333703, 0.3299404806269776169, 0.3333333333333333703, 0.3299404806269776169, 0.3333333333333333703, 0.3299404806269776169, 0.3333333333333333703, 0.3299404806269776169, 0.3333333333333333703, 0.3299404806269776169, 0.3333333333333333703, 0.3299404806269776169, 0.3333333333333333703, 0.3299404806269776169, 0.3333333333333333703, 0.3299404806269776169, 0.3333333333333333703, 0.3299404806269776169, 0.3333333333333333703, 0.3299404806269776169, 0.3333333333333333703, 0.3299404806269776169, 0.3333333333333333703, 0.3299404806269776169, 0.3333333333333333703, 0.3299404806269776169, 0.3333333333333333703, 0.3299404806269776169, 0.3333333333333333703, 0.3299404806269776169, 0.3333333333333333703, 0.3299404806269776169, 0.3333333333333333703, 0.3299404806269776169, 0.3333333333333333703, 0.3299404806269776169, 0.3333333333333333703, 0.3299404806269776169, 0.3333333333333333703, 0.3299404806269776169, 0.3333333333333333703, 0.3299404806269776169, 0.3333333333333333703, 0.3299404806269776169, 0.3333333333333333703, 0.3299404806269776169, 0.3333333333333333703, 0.3299404806269776169, 0.3333333333333333703, 0.3299404806269776169, 0.3333333333333333703, 0.3299404806269776169, 0.3333333333333333703, 0.3299404806269776169, 0.3333333333333333703, 0.3299404806269776169, 0.3333333333333333703, 0.3299404806269776169, 0.3333333333333333703, 0.3299404806269776169, 0.3333333333333333703, 0.3299404806269776169, 0.3333333333333333703, 0.3299404806269776169, 0.3333333333333333703, 0.3299404806269776169, 0.3333333333333333703, 0.3299404806269776169, 0.3333333333333333703, 0.3299404806269776169, 0.3333333333333333703, 0.3299404806269776169, 0.3333333333333333703, 0.3299404806269776169, 0.3333333333333333703, 0.3299404806269776169, 0.3333333333333333703, 0.3299404806269776169, 0.3333333333333333703, 0.3299404806269776169, 0.3333333333333333703, 0.3299404806269776169, 0.3333333333333333703, 0.3299404806269776169, 0.3333333333333333703, 0.3299404806269776169, 0.3333333333333333703, 0.3299404806269776169, 0.3333333333333333703, 0.3299404806269776169, 0.3333333333333333703, 0.3299404806269776169, 0.3333333333333333703, 0.3299404806269776169, 0.3333333333333333703, 0.3299404806269776169, 0.3333333333333333703, 0.3299404806269776169, 0.3333333333333333703, 0.3299404806269776169, 0.3333333333333333703, 0.3299404806269776169, 0.3333333333333333703, 0.3299404806269776169, 0.3333333333333333703, 0.3299404806269776169, 0.3333333333333333703, 0.3299404806269776169, 0.3333333333333333703, 0.3299404806269776169, 0.3333333333333333703, 0.3299404806269776169, 0.3333333333333333703, 0.3299404806269776169, 0.3333333333333333703, 0.3299404806269776169, 0.3333333333333333703, 0.3299404806269776169, 0.3333333333333333703, 0.3299404806269776169, 0.3333333333333333703, 0.3299404806269776169, 0.3333333333333333703, 0.3299404806269776169, 0.3333333333333333703, 0.3299404806269776169, 0.3333333333333333703, 0.3299404806269776169, 0.3333333333333333703, 0.3299404806269776169, 0.3333333333333333703, 0.3299404806269776169, 0.3333333333333333703, 0.3299404806269776169, 0.3333333333333333703, 0.3299404806269776169, 0.3333333333333333703, 0.3299404806269776169, 0.3333333333333333703, 0.3299404806269776169, 0.3333333333333333703, 0.3299404806269776169, 0.3333333333333333703, 0.3299404806269776169, 0.3333333333333333703, 0.3299404806269776169, 0.3333333333333333703, 0.3299404806269776169, 0.3333333333333333703, 0.3299404806269776169, 0.3333333333333333703, 0.3299404806269776169, 0.3333333333333333703, 0.3299404806269776169, 0.3333333333333333703, 0.3299404806269776169, 0.3333333333333333703, 0.3299404806269776169, 0.3333333333333333703, 0.3299404806269776169, 0.3333333333333333703, 0.3299404806269776169, 0.3333333333333333703, 0.3299404806269776169, 0.3333333333333333703, 0.3299404806269776169, 0.3333333333333333703, 0.3299404806269776169, 0.3333333333333333703, 0.3299404806269776169, 0.3333333333333333703, 0.3299404806269776169, 0.3333333333333333703, 0.3299404806269776169, 0.3333333333333333703, 0.3299404806269776169, 0.3333333333333333703, 0.3299404806269776169, 0.3333333333333333703, 0.3299404806269776169, 0.3333333333333333703, 0.3299404806269776169, 0.3333333333333333703, 0.3299404806269776169, 0.3333333333333333703, 0.3299404806269776169, 0.3333333333333333703, 0.3299404806269776169, 0.3333333333333333703, 0.3299404806269776169, 0.3333333333333333703, 0.3299404806269776169, 0.3333333333333333703, 0.3299404806269776169, 0.3333333333333333703, 0.3299404806269776169, 0.3333333333333333703, 0.3299404806269776169, 0.3333333333333333703, 0.3299404806269776169, 0.3333333333333333703, 0.3299404806269776169, 0.3333333333333333703, 0.3299404806269776169, 0.3333333333333333703, 0.3299404806269776169, 0.3333333333333333703, 0.3299404806269776169, 0.3333333333333333703, 0.3299404806269776169, 0.3333333333333333703, 0.3299404806269776169, 0.3333333333333333703, 0.3299404806269776169, 0.3333333333333333703, 0.3299404806269776169, 0.3333333333333333703, 0.3299404806269776169, 0.3333333333333333703, 0.3299404806269776169, 0.3333333333333333703, 0.3299404806269776169, 0.3333333333333333703, 0.3299404806269776169, 0.3333333333333333703, 0.3299404806269776169, 0.3333333333333333703, 0.3299404806269776169, 0.3333333333333333703, 0.3299404806269776169, 0.3333333333333333703, 0.3299404806269776169, 0.3333333333333333703, 0.3299404806269776169, 0.3333333333333333703, 0.3299404806269776169, 0.3333333333333333703, 0.3299404806269776169, 0.3333333333333333703, 0.3299404806269776169, 0.3333333333333333703, 0.3299404806269776169, 0.3333333333333333703, 0.3299404806269776169, 0.3333333333333333703, 0.3299404806269776169, 0.3333333333333333703, 0.3299404806269776169, 0.3333333333333333703, 0.3299404806269776169, 0.3333333333333333703, 0.3299404806269776169, 0.3333333333333333703, 0.3299404806269776169, 0.3333333333333333703, 0.3299404806269776169, 0.3333333333333333703, 0.3299404806269776169, 0.3333333333333333703, 0.3299404806269776169, 0.3333333333333333703, 0.3299404806269776169, 0.3333333333333333703, 0.3299404806269776169, 0.3333333333333333703, 0.3299404806269776169, 0.3333333333333333703, 0.3299404806269776169, 0.3333333333333333703, 0.3299404806269776169, 0.3333333333333333703, 0.3299404806269776169, 0.3333333333333333703, 0.3299404806269776169, 0.3333333333333333703, 0.3299404806269776169, 0.3333333333333333703, 0.3299404806269776169, 0.3333333333333333703, 0.3299404806269776169, 0.3333333333333333703, 0.3299404806269776169, 0.3333333333333333703, 0.3299404806269776169, 0.3333333333333333703, 0.3299404806269776169, 0.3333333333333333703, 0.3299404806269776169, 0.3333333333333333703, 0.3299404806269776169, 0.3333333333333333703, 0.3299404806269776169, 0.3333333333333333703, 0.3299404806269776169, 0.3333333333333333703, 0.3299404806269776169, 0.3333333333333333703, 0.3299404806269776169, 0.3333333333333333703, 0.3299404806269776169, 0.3333333333333333703, 0.3299404806269776169, 0.3333333333333333703, 0.3299404806269776169, 0.3333333333333333703, 0.3299404806269776169, 0.3333333333333333703, 0.3299404806269776169, 0.3333333333333333703, 0.3299404806269776169, 0.3333333333333333703, 0.3299404806269776169, 0.3333333333333333703, 0.3299404806269776169, 0.3333333333333333703, 0.3299404806269776169, 0.3333333333333333703, 0.3299404806269776169, 0.3333333333333333703, 0.3299404806269776169, 0.3333333333333333703, 0.3299404806269776169, 0.3333333333333333703, 0.3299404806269776169, 0.3333333333333333703, 0.3299404806269776169, 0.3333333333333333703, 0.3299404806269776169, 0.3333333333333333703, 0.3299404806269776169, 0.3333333333333333703, 0.3299404806269776169, 0.3333333333333333703, 0.3299404806269776169, 0.3333333333333333703, 0.3299404806269776169, 0.3333333333333333703, 0.3299404806269776169, 0.3333333333333333703, 0.3299404806269776169, 0.3333333333333333703, 0.3299404806269776169, 0.3333333333333333703, 0.3299404806269776169, 0.3333333333333333703, 0.3299404806269776169, 0.3333333333333333703, 0.3299404806269776169, 0.3333333333333333703, 0.3299404806269776169, 0.3333333333333333703, 0.3299404806269776169, 0.3333333333333333703, 0.3299404806269776169, 0.3333333333333333703, 0.3299404806269776169, 0.3333333333333333703, 0.3299404806269776169, 0.3333333333333333703, 0.3299404806269776169, 0.3333333333333333703, 0.3299404806269776169, 0.3333333333333333703, 0.3299404806269776169, 0.3333333333333333703, 0.3299404806269776169, 0.3333333333333333703, 0.3299404806269776169, 0.3333333333333333703, 0.3299404806269776169, 0.3333333333333333703, 0.3320603117974822438, 0.3317425830320511193),
 ( 0.3333333333333333703, 0.3299404806269776169, 0.3333333333333333703, 0.3299404806269776169, 0.3333333333333333703, 0.3299404806269776169, 0.3333333333333333703, 0.3299404806269776169, 0.3333333333333333703, 0.3299404806269776169, 0.3333333333333333703, 0.3299404806269776169, 0.3333333333333333703, 0.3299404806269776169, 0.3333333333333333703, 0.3299404806269776169, 0.3333333333333333703, 0.3299404806269776169, 0.3333333333333333703, 0.3299404806269776169, 0.3333333333333333703, 0.3299404806269776169, 0.3333333333333333703, 0.3299404806269776169, 0.3333333333333333703, 0.3299404806269776169, 0.3333333333333333703, 0.3299404806269776169, 0.3333333333333333703, 0.3299404806269776169, 0.3333333333333333703, 0.3299404806269776169, 0.3333333333333333703, 0.3299404806269776169, 0.3333333333333333703, 0.3299404806269776169, 0.3333333333333333703, 0.3299404806269776169, 0.3333333333333333703, 0.3299404806269776169, 0.3333333333333333703, 0.3299404806269776169, 0.3333333333333333703, 0.3299404806269776169, 0.3333333333333333703, 0.3299404806269776169, 0.3333333333333333703, 0.3299404806269776169, 0.3333333333333333703, 0.3299404806269776169, 0.3333333333333333703, 0.3299404806269776169, 0.3333333333333333703, 0.3299404806269776169, 0.3333333333333333703, 0.3299404806269776169, 0.3333333333333333703, 0.3299404806269776169, 0.3333333333333333703, 0.3299404806269776169, 0.3333333333333333703, 0.3299404806269776169, 0.3333333333333333703, 0.3299404806269776169, 0.3333333333333333703, 0.3299404806269776169, 0.3333333333333333703, 0.3299404806269776169, 0.3333333333333333703, 0.3299404806269776169, 0.3333333333333333703, 0.3299404806269776169, 0.3333333333333333703, 0.3299404806269776169, 0.3333333333333333703, 0.3299404806269776169, 0.3333333333333333703, 0.3299404806269776169, 0.3333333333333333703, 0.3299404806269776169, 0.3333333333333333703, 0.3299404806269776169, 0.3333333333333333703, 0.3299404806269776169, 0.3333333333333333703, 0.3299404806269776169, 0.3333333333333333703, 0.3299404806269776169, 0.3333333333333333703, 0.3299404806269776169, 0.3333333333333333703, 0.3299404806269776169, 0.3333333333333333703, 0.3299404806269776169, 0.3333333333333333703, 0.3299404806269776169, 0.3333333333333333703, 0.3299404806269776169, 0.3333333333333333703, 0.3299404806269776169, 0.3333333333333333703, 0.3299404806269776169, 0.3333333333333333703, 0.3299404806269776169, 0.3333333333333333703, 0.3299404806269776169, 0.3333333333333333703, 0.3299404806269776169, 0.3333333333333333703, 0.3299404806269776169, 0.3333333333333333703, 0.3299404806269776169, 0.3333333333333333703, 0.3299404806269776169, 0.3333333333333333703, 0.3299404806269776169, 0.3333333333333333703, 0.3299404806269776169, 0.3333333333333333703, 0.3299404806269776169, 0.3333333333333333703, 0.3299404806269776169, 0.3333333333333333703, 0.3299404806269776169, 0.3333333333333333703, 0.3299404806269776169, 0.3333333333333333703, 0.3299404806269776169, 0.3333333333333333703, 0.3299404806269776169, 0.3333333333333333703, 0.3299404806269776169, 0.3333333333333333703, 0.3299404806269776169, 0.3333333333333333703, 0.3299404806269776169, 0.3333333333333333703, 0.3299404806269776169, 0.3333333333333333703, 0.3299404806269776169, 0.3333333333333333703, 0.3299404806269776169, 0.3333333333333333703, 0.3299404806269776169, 0.3333333333333333703, 0.3299404806269776169, 0.3333333333333333703, 0.3299404806269776169, 0.3333333333333333703, 0.3299404806269776169, 0.3333333333333333703, 0.3299404806269776169, 0.3333333333333333703, 0.3299404806269776169, 0.3333333333333333703, 0.3299404806269776169, 0.3333333333333333703, 0.3299404806269776169, 0.3333333333333333703, 0.3299404806269776169, 0.3333333333333333703, 0.3299404806269776169, 0.3333333333333333703, 0.3299404806269776169, 0.3333333333333333703, 0.3299404806269776169, 0.3333333333333333703, 0.3299404806269776169, 0.3333333333333333703, 0.3299404806269776169, 0.3333333333333333703, 0.3299404806269776169, 0.3333333333333333703, 0.3299404806269776169, 0.3333333333333333703, 0.3299404806269776169, 0.3333333333333333703, 0.3299404806269776169, 0.3333333333333333703, 0.3299404806269776169, 0.3333333333333333703, 0.3299404806269776169, 0.3333333333333333703, 0.3299404806269776169, 0.3333333333333333703, 0.3299404806269776169, 0.3333333333333333703, 0.3299404806269776169, 0.3333333333333333703, 0.3299404806269776169, 0.3333333333333333703, 0.3299404806269776169, 0.3333333333333333703, 0.3299404806269776169, 0.3333333333333333703, 0.3299404806269776169, 0.3333333333333333703, 0.3299404806269776169, 0.3333333333333333703, 0.3299404806269776169, 0.3333333333333333703, 0.3299404806269776169, 0.3333333333333333703, 0.3299404806269776169, 0.3333333333333333703, 0.3299404806269776169, 0.3333333333333333703, 0.3299404806269776169, 0.3333333333333333703, 0.3299404806269776169, 0.3333333333333333703, 0.3299404806269776169, 0.3333333333333333703, 0.3299404806269776169, 0.3333333333333333703, 0.3299404806269776169, 0.3333333333333333703, 0.3299404806269776169, 0.3333333333333333703, 0.3299404806269776169, 0.3333333333333333703, 0.3299404806269776169, 0.3333333333333333703, 0.3299404806269776169, 0.3333333333333333703, 0.3299404806269776169, 0.3333333333333333703, 0.3299404806269776169, 0.3333333333333333703, 0.3299404806269776169, 0.3333333333333333703, 0.3299404806269776169, 0.3333333333333333703, 0.3299404806269776169, 0.3333333333333333703, 0.3299404806269776169, 0.3333333333333333703, 0.3299404806269776169, 0.3333333333333333703, 0.3299404806269776169, 0.3333333333333333703, 0.3299404806269776169, 0.3333333333333333703, 0.3299404806269776169, 0.3333333333333333703, 0.3299404806269776169, 0.3333333333333333703, 0.3299404806269776169, 0.3333333333333333703, 0.3299404806269776169, 0.3333333333333333703, 0.3299404806269776169, 0.3333333333333333703, 0.3299404806269776169, 0.3333333333333333703, 0.3299404806269776169, 0.3333333333333333703, 0.3299404806269776169, 0.3333333333333333703, 0.3299404806269776169, 0.3333333333333333703, 0.3299404806269776169, 0.3333333333333333703, 0.3299404806269776169, 0.3333333333333333703, 0.3299404806269776169, 0.3333333333333333703, 0.3299404806269776169, 0.3333333333333333703, 0.3299404806269776169, 0.3333333333333333703, 0.3299404806269776169, 0.3333333333333333703, 0.3299404806269776169, 0.3333333333333333703, 0.3299404806269776169, 0.3333333333333333703, 0.3299404806269776169, 0.3333333333333333703, 0.3299404806269776169, 0.3333333333333333703, 0.3299404806269776169, 0.3333333333333333703, 0.3299404806269776169, 0.3333333333333333703, 0.3299404806269776169, 0.3333333333333333703, 0.3299404806269776169, 0.3333333333333333703, 0.3299404806269776169, 0.3333333333333333703, 0.3299404806269776169, 0.3333333333333333703, 0.3299404806269776169, 0.3333333333333333703, 0.3299404806269776169, 0.3333333333333333703, 0.3299404806269776169, 0.3333333333333333703, 0.3299404806269776169, 0.3333333333333333703, 0.3299404806269776169, 0.3333333333333333703, 0.3299404806269776169, 0.3333333333333333703, 0.3299404806269776169, 0.3333333333333333703, 0.3299404806269776169, 0.3333333333333333703, 0.3299404806269776169, 0.3333333333333333703, 0.3299404806269776169, 0.3333333333333333703, 0.3299404806269776169, 0.3333333333333333703, 0.3299404806269776169, 0.3333333333333333703, 0.3299404806269776169, 0.3333333333333333703, 0.3299404806269776169, 0.3333333333333333703, 0.3299404806269776169, 0.3333333333333333703, 0.3299404806269776169, 0.3333333333333333703, 0.3299404806269776169, 0.3333333333333333703, 0.3299404806269776169, 0.3333333333333333703, 0.3299404806269776169, 0.3333333333333333703, 0.3299404806269776169, 0.3333333333333333703, 0.3299404806269776169, 0.3333333333333333703, 0.3299404806269776169, 0.3333333333333333703, 0.3299404806269776169, 0.3333333333333333703, 0.3299404806269776169, 0.3333333333333333703, 0.3299404806269776169, 0.3333333333333333703, 0.3299404806269776169, 0.3333333333333333703, 0.3299404806269776169, 0.3333333333333333703, 0.3299404806269776169, 0.3333333333333333703, 0.3299404806269776169, 0.3333333333333333703, 0.3299404806269776169, 0.3333333333333333703, 0.3299404806269776169, 0.3333333333333333703, 0.3299404806269776169, 0.3333333333333333703, 0.3299404806269776169, 0.3333333333333333703, 0.3299404806269776169, 0.3333333333333333703, 0.3299404806269776169, 0.3333333333333333703, 0.3299404806269776169, 0.3333333333333333703, 0.3299404806269776169, 0.3333333333333333703, 0.3299404806269776169, 0.3333333333333333703, 0.3299404806269776169, 0.3333333333333333703, 0.3299404806269776169, 0.3333333333333333703, 0.3299404806269776169, 0.3333333333333333703, 0.3299404806269776169, 0.3333333333333333703, 0.3299404806269776169, 0.3333333333333333703, 0.3299404806269776169, 0.3333333333333333703, 0.3299404806269776169, 0.3333333333333333703, 0.3299404806269776169, 0.3333333333333333703, 0.3299404806269776169, 0.3333333333333333703, 0.3299404806269776169, 0.3333333333333333703, 0.3299404806269776169, 0.3333333333333333703, 0.3299404806269776169, 0.3333333333333333703, 0.3299404806269776169, 0.3333333333333333703, 0.3299404806269776169, 0.3333333333333333703, 0.3299404806269776169, 0.3333333333333333703, 0.3299404806269776169, 0.3333333333333333703, 0.3299404806269776169, 0.3333333333333333703, 0.3299404806269776169, 0.3333333333333333703, 0.3299404806269776169, 0.3333333333333333703, 0.3299404806269776169, 0.3333333333333333703, 0.3299404806269776169, 0.3333333333333333703, 0.3299404806269776169, 0.3333333333333333703, 0.3299404806269776169, 0.3333333333333333703, 0.3299404806269776169, 0.3333333333333333703, 0.3299404806269776169, 0.3333333333333333703, 0.3299404806269776169, 0.3333333333333333703, 0.3299404806269776169, 0.3333333333333333703, 0.3299404806269776169, 0.3333333333333333703, 0.3299404806269776169, 0.3333333333333333703, 0.3299404806269776169, 0.3333333333333333703, 0.3299404806269776169, 0.3333333333333333703, 0.3299404806269776169, 0.3333333333333333703, 0.3299404806269776169, 0.3333333333333333703, 0.3299404806269776169, 0.3333333333333333703, 0.3299404806269776169, 0.3333333333333333703, 0.3299404806269776169, 0.3333333333333333703, 0.3299404806269776169, 0.3333333333333333703, 0.3299404806269776169, 0.3333333333333333703, 0.3299404806269776169, 0.3333333333333333703, 0.3299404806269776169, 0.3333333333333333703, 0.3299404806269776169, 0.3333333333333333703, 0.3299404806269776169, 0.3333333333333333703, 0.3299404806269776169, 0.3333333333333333703, 0.3299404806269776169, 0.3333333333333333703, 0.3299404806269776169, 0.3333333333333333703, 0.3299404806269776169, 0.3333333333333333703, 0.3299404806269776169, 0.3333333333333333703, 0.3299404806269776169, 0.3333333333333333703, 0.3299404806269776169, 0.3333333333333333703, 0.3299404806269776169, 0.3333333333333333703, 0.3299404806269776169, 0.3333333333333333703, 0.3299404806269776169, 0.3333333333333333703, 0.3299404806269776169, 0.3333333333333333703, 0.3299404806269776169, 0.3333333333333333703, 0.3299404806269776169, 0.3333333333333333703, 0.3299404806269776169, 0.3333333333333333703, 0.3299404806269776169, 0.3333333333333333703, 0.3299404806269776169, 0.3333333333333333703, 0.3299404806269776169, 0.3333333333333333703, 0.3299404806269776169, 0.3333333333333333703, 0.3299404806269776169, 0.3333333333333333703, 0.3299404806269776169, 0.3333333333333333703, 0.3299404806269776169, 0.3333333333333333703, 0.3299404806269776169, 0.3333333333333333703, 0.3299404806269776169, 0.3333333333333333703, 0.3299404806269776169, 0.3333333333333333703, 0.3299404806269776169, 0.3333333333333333703, 0.3299404806269776169, 0.3333333333333333703, 0.3299404806269776169, 0.3333333333333333703, 0.3299404806269776169, 0.3333333333333333703, 0.3299404806269776169, 0.3333333333333333703, 0.3299404806269776169, 0.3333333333333333703, 0.3299404806269776169, 0.3333333333333333703, 0.3299404806269776169, 0.3333333333333333703, 0.3299404806269776169, 0.3333333333333333703, 0.3299404806269776169, 0.3333333333333333703, 0.3299404806269776169, 0.3333333333333333703, 0.3299404806269776169, 0.3333333333333333703, 0.3299404806269776169, 0.3333333333333333703, 0.3299404806269776169, 0.3333333333333333703, 0.3299404806269776169, 0.3333333333333333703, 0.3299404806269776169, 0.3333333333333333703, 0.3299404806269776169, 0.3333333333333333703, 0.3299404806269776169, 0.3333333333333333703, 0.3299404806269776169, 0.3333333333333333703, 0.3299404806269776169, 0.3333333333333333703, 0.3299404806269776169, 0.3333333333333333703, 0.3299404806269776169, 0.3333333333333333703, 0.3299404806269776169, 0.3333333333333333703, 0.3299404806269776169, 0.3333333333333333703, 0.3299404806269776169, 0.3333333333333333703, 0.3299404806269776169, 0.3333333333333333703, 0.3299404806269776169, 0.3333333333333333703, 0.3299404806269776169, 0.3333333333333333703, 0.3299404806269776169, 0.3333333333333333703, 0.3299404806269776169, 0.3333333333333333703, 0.3299404806269776169, 0.3333333333333333703, 0.3299404806269776169, 0.3333333333333333703, 0.3299404806269776169, 0.3333333333333333703, 0.3299404806269776169, 0.3333333333333333703, 0.3299404806269776169, 0.3333333333333333703, 0.3299404806269776169, 0.3333333333333333703, 0.3299404806269776169, 0.3333333333333333703, 0.3299404806269776169, 0.3333333333333333703, 0.3299404806269776169, 0.3333333333333333703, 0.3299404806269776169, 0.3333333333333333703, 0.3299404806269776169, 0.3333333333333333703, 0.3299404806269776169, 0.3333333333333333703, 0.3299404806269776169, 0.3333333333333333703, 0.3299404806269776169, 0.3333333333333333703, 0.3299404806269776169, 0.3333333333333333703, 0.3299404806269776169, 0.3333333333333333703, 0.3299404806269776169, 0.3333333333333333703, 0.3299404806269776169, 0.3333333333333333703, 0.3299404806269776169, 0.3333333333333333703, 0.3299404806269776169, 0.3333333333333333703, 0.3299404806269776169, 0.3333333333333333703, 0.3299404806269776169, 0.3333333333333333703, 0.3299404806269776169, 0.3333333333333333703, 0.3299404806269776169, 0.3333333333333333703, 0.3299404806269776169, 0.3333333333333333703, 0.3299404806269776169, 0.3333333333333333703, 0.3299404806269776169, 0.3333333333333333703, 0.3299404806269776169, 0.3333333333333333703, 0.3299404806269776169, 0.3333333333333333703, 0.3299404806269776169, 0.3333333333333333703, 0.3299404806269776169, 0.3333333333333333703, 0.3299404806269776169, 0.3333333333333333703, 0.3299404806269776169, 0.3333333333333333703, 0.3299404806269776169, 0.3333333333333333703, 0.3299404806269776169, 0.3333333333333333703, 0.3299404806269776169, 0.3333333333333333703, 0.3299404806269776169, 0.3333333333333333703, 0.3299404806269776169, 0.3333333333333333703, 0.3299404806269776169, 0.3333333333333333703, 0.3299404806269776169, 0.3333333333333333703, 0.3299404806269776169, 0.3333333333333333703, 0.3299404806269776169, 0.3333333333333333703, 0.3299404806269776169, 0.3333333333333333703, 0.3299404806269776169, 0.3333333333333333703, 0.3299404806269776169, 0.3333333333333333703, 0.3299404806269776169, 0.3333333333333333703, 0.3299404806269776169, 0.3333333333333333703, 0.3299404806269776169, 0.3333333333333333703, 0.3299404806269776169, 0.3333333333333333703, 0.3299404806269776169, 0.3333333333333333703, 0.3299404806269776169, 0.3333333333333333703, 0.3299404806269776169, 0.3333333333333333703, 0.3299404806269776169, 0.3333333333333333703, 0.3299404806269776169, 0.3333333333333333703, 0.3299404806269776169, 0.3333333333333333703, 0.3299404806269776169, 0.3333333333333333703, 0.3299404806269776169, 0.3333333333333333703, 0.3299404806269776169, 0.3333333333333333703, 0.3299404806269776169, 0.3333333333333333703, 0.3299404806269776169, 0.3333333333333333703, 0.3299404806269776169, 0.3333333333333333703, 0.3299404806269776169, 0.3333333333333333703, 0.3299404806269776169, 0.3333333333333333703, 0.3299404806269776169, 0.3333333333333333703, 0.3299404806269776169, 0.3333333333333333703, 0.3299404806269776169, 0.3333333333333333703, 0.3299404806269776169, 0.3333333333333333703, 0.3299404806269776169, 0.3333333333333333703, 0.3299404806269776169, 0.3333333333333333703, 0.3299404806269776169, 0.3333333333333333703, 0.3299404806269776169, 0.3333333333333333703, 0.3299404806269776169, 0.3333333333333333703, 0.3299404806269776169, 0.3333333333333333703, 0.3299404806269776169, 0.3333333333333333703, 0.3299404806269776169, 0.3333333333333333703, 0.3299404806269776169, 0.3333333333333333703, 0.3299404806269776169, 0.3333333333333333703, 0.3299404806269776169, 0.3333333333333333703, 0.3299404806269776169, 0.3333333333333333703, 0.3299404806269776169, 0.3333333333333333703, 0.3299404806269776169, 0.3333333333333333703, 0.3299404806269776169, 0.3333333333333333703, 0.3299404806269776169, 0.3333333333333333703, 0.3299404806269776169, 0.3333333333333333703, 0.3299404806269776169, 0.3333333333333333703, 0.3299404806269776169, 0.3333333333333333703, 0.3299404806269776169, 0.3333333333333333703, 0.3299404806269776169, 0.3333333333333333703, 0.3299404806269776169, 0.3333333333333333703, 0.3299404806269776169, 0.3333333333333333703, 0.3299404806269776169, 0.3333333333333333703, 0.3299404806269776169, 0.3333333333333333703, 0.3299404806269776169, 0.3333333333333333703, 0.3299404806269776169, 0.3333333333333333703, 0.3299404806269776169, 0.3333333333333333703, 0.3299404806269776169, 0.3333333333333333703, 0.3299404806269776169, 0.3333333333333333703, 0.3299404806269776169, 0.3333333333333333703, 0.3299404806269776169, 0.3333333333333333703, 0.3299404806269776169, 0.3333333333333333703, 0.3299404806269776169, 0.3333333333333333703, 0.3299404806269776169, 0.3333333333333333703, 0.3299404806269776169, 0.3333333333333333703, 0.3299404806269776169, 0.3333333333333333703, 0.3299404806269776169, 0.3333333333333333703, 0.3299404806269776169, 0.3333333333333333703, 0.3299404806269776169, 0.3333333333333333703, 0.3299404806269776169, 0.3333333333333333703, 0.3299404806269776169, 0.3333333333333333703, 0.3299404806269776169, 0.3333333333333333703, 0.3299404806269776169, 0.3333333333333333703, 0.3299404806269776169, 0.3333333333333333703, 0.3299404806269776169, 0.3333333333333333703, 0.3299404806269776169, 0.3333333333333333703, 0.3299404806269776169, 0.3333333333333333703, 0.3299404806269776169, 0.3333333333333333703, 0.3299404806269776169, 0.3333333333333333703, 0.3299404806269776169, 0.3333333333333333703, 0.3299404806269776169, 0.3333333333333333703, 0.3299404806269776169, 0.3333333333333333703, 0.3299404806269776169, 0.3333333333333333703, 0.3299404806269776169, 0.3333333333333333703, 0.3299404806269776169, 0.3333333333333333703, 0.3299404806269776169, 0.3333333333333333703, 0.3299404806269776169, 0.3333333333333333703, 0.3299404806269776169, 0.3333333333333333703, 0.3299404806269776169, 0.3333333333333333703, 0.3299404806269776169, 0.3333333333333333703, 0.3299404806269776169, 0.3333333333333333703, 0.3299404806269776169, 0.3333333333333333703, 0.3299404806269776169, 0.3333333333333333703, 0.3299404806269776169, 0.3333333333333333703, 0.3299404806269776169, 0.3333333333333333703, 0.3299404806269776169, 0.3333333333333333703, 0.3299404806269776169, 0.3333333333333333703, 0.3299404806269776169, 0.3333333333333333703, 0.3299404806269776169, 0.3333333333333333703, 0.3299404806269776169, 0.3333333333333333703, 0.3299404806269776169, 0.3333333333333333703, 0.3299404806269776169, 0.3333333333333333703, 0.3299404806269776169, 0.3333333333333333703, 0.3299404806269776169, 0.3333333333333333703, 0.3299404806269776169, 0.3333333333333333703, 0.3299404806269776169, 0.3333333333333333703, 0.3299404806269776169, 0.3333333333333333703, 0.3299404806269776169, 0.3333333333333333703, 0.3299404806269776169, 0.3333333333333333703, 0.3299404806269776169, 0.3333333333333333703, 0.3299404806269776169, 0.3333333333333333703, 0.3299404806269776169, 0.3333333333333333703, 0.3320603117974822438, 0.3317425830320511193),
 ( 1.000000000000000000, 0.9898214418809326842, 1.000000000000000000, 0.9898214418809326842, 1.000000000000000000, 0.9898214418809326842, 1.000000000000000000, 0.9898214418809326842, 1.000000000000000000, 0.9898214418809326842, 1.000000000000000000, 0.9898214418809326842, 1.000000000000000000, 0.9898214418809326842, 1.000000000000000000, 0.9898214418809326842, 1.000000000000000000, 0.9898214418809326842, 1.000000000000000000, 0.9898214418809326842, 1.000000000000000000, 0.9898214418809326842, 1.000000000000000000, 0.9898214418809326842, 1.000000000000000000, 0.9898214418809326842, 1.000000000000000000, 0.9898214418809326842, 1.000000000000000000, 0.9898214418809326842, 1.000000000000000000, 0.9898214418809326842, 1.000000000000000000, 0.9898214418809326842, 1.000000000000000000, 0.9898214418809326842, 1.000000000000000000, 0.9898214418809326842, 1.000000000000000000, 0.9898214418809326842, 1.000000000000000000, 0.9898214418809326842, 1.000000000000000000, 0.9898214418809326842, 1.000000000000000000, 0.9898214418809326842, 1.000000000000000000, 0.9898214418809326842, 1.000000000000000000, 0.9898214418809326842, 1.000000000000000000, 0.9898214418809326842, 1.000000000000000000, 0.9898214418809326842, 1.000000000000000000, 0.9898214418809326842, 1.000000000000000000, 0.9898214418809326842, 1.000000000000000000, 0.9898214418809326842, 1.000000000000000000, 0.9898214418809326842, 1.000000000000000000, 0.9898214418809326842, 1.000000000000000000, 0.9898214418809326842, 1.000000000000000000, 0.9898214418809326842, 1.000000000000000000, 0.9898214418809326842, 1.000000000000000000, 0.9898214418809326842, 1.000000000000000000, 0.9898214418809326842, 1.000000000000000000, 0.9898214418809326842, 1.000000000000000000, 0.9898214418809326842, 1.000000000000000000, 0.9898214418809326842, 1.000000000000000000, 0.9898214418809326842, 1.000000000000000000, 0.9898214418809326842, 1.000000000000000000, 0.9898214418809326842, 1.000000000000000000, 0.9898214418809326842, 1.000000000000000000, 0.9898214418809326842, 1.000000000000000000, 0.9898214418809326842, 1.000000000000000000, 0.9898214418809326842, 1.000000000000000000, 0.9898214418809326842, 1.000000000000000000, 0.9898214418809326842, 1.000000000000000000, 0.9898214418809326842, 1.000000000000000000, 0.9898214418809326842, 1.000000000000000000, 0.9898214418809326842, 1.000000000000000000, 0.9898214418809326842, 1.000000000000000000, 0.9898214418809326842, 1.000000000000000000, 0.9898214418809326842, 1.000000000000000000, 0.9898214418809326842, 1.000000000000000000, 0.9898214418809326842, 1.000000000000000000, 0.9898214418809326842, 1.000000000000000000, 0.9898214418809326842, 1.000000000000000000, 0.9898214418809326842, 1.000000000000000000, 0.9898214418809326842, 1.000000000000000000, 0.9898214418809326842, 1.000000000000000000, 0.9898214418809326842, 1.000000000000000000, 0.9898214418809326842, 1.000000000000000000, 0.9898214418809326842, 1.000000000000000000, 0.9898214418809326842, 1.000000000000000000, 0.9898214418809326842, 1.000000000000000000, 0.9898214418809326842, 1.000000000000000000, 0.9898214418809326842, 1.000000000000000000, 0.9898214418809326842, 1.000000000000000000, 0.9898214418809326842, 1.000000000000000000, 0.9898214418809326842, 1.000000000000000000, 0.9898214418809326842, 1.000000000000000000, 0.9898214418809326842, 1.000000000000000000, 0.9898214418809326842, 1.000000000000000000, 0.9898214418809326842, 1.000000000000000000, 0.9898214418809326842, 1.000000000000000000, 0.9898214418809326842, 1.000000000000000000, 0.9898214418809326842, 1.000000000000000000, 0.9898214418809326842, 1.000000000000000000, 0.9898214418809326842, 1.000000000000000000, 0.9898214418809326842, 1.000000000000000000, 0.9898214418809326842, 1.000000000000000000, 0.9898214418809326842, 1.000000000000000000, 0.9898214418809326842, 1.000000000000000000, 0.9898214418809326842, 1.000000000000000000, 0.9898214418809326842, 1.000000000000000000, 0.9898214418809326842, 1.000000000000000000, 0.9898214418809326842, 1.000000000000000000, 0.9898214418809326842, 1.000000000000000000, 0.9898214418809326842, 1.000000000000000000, 0.9898214418809326842, 1.000000000000000000, 0.9898214418809326842, 1.000000000000000000, 0.9898214418809326842, 1.000000000000000000, 0.9898214418809326842, 1.000000000000000000, 0.9898214418809326842, 1.000000000000000000, 0.9898214418809326842, 1.000000000000000000, 0.9898214418809326842, 1.000000000000000000, 0.9898214418809326842, 1.000000000000000000, 0.9898214418809326842, 1.000000000000000000, 0.9898214418809326842, 1.000000000000000000, 0.9898214418809326842, 1.000000000000000000, 0.9898214418809326842, 1.000000000000000000, 0.9898214418809326842, 1.000000000000000000, 0.9898214418809326842, 1.000000000000000000, 0.9898214418809326842, 1.000000000000000000, 0.9898214418809326842, 1.000000000000000000, 0.9898214418809326842, 1.000000000000000000, 0.9898214418809326842, 1.000000000000000000, 0.9898214418809326842, 1.000000000000000000, 0.9898214418809326842, 1.000000000000000000, 0.9898214418809326842, 1.000000000000000000, 0.9898214418809326842, 1.000000000000000000, 0.9898214418809326842, 1.000000000000000000, 0.9898214418809326842, 1.000000000000000000, 0.9898214418809326842, 1.000000000000000000, 0.9898214418809326842, 1.000000000000000000, 0.9898214418809326842, 1.000000000000000000, 0.9898214418809326842, 1.000000000000000000, 0.9898214418809326842, 1.000000000000000000, 0.9898214418809326842, 1.000000000000000000, 0.9898214418809326842, 1.000000000000000000, 0.9898214418809326842, 1.000000000000000000, 0.9898214418809326842, 1.000000000000000000, 0.9898214418809326842, 1.000000000000000000, 0.9898214418809326842, 1.000000000000000000, 0.9898214418809326842, 1.000000000000000000, 0.9898214418809326842, 1.000000000000000000, 0.9898214418809326842, 1.000000000000000000, 0.9898214418809326842, 1.000000000000000000, 0.9898214418809326842, 1.000000000000000000, 0.9898214418809326842, 1.000000000000000000, 0.9898214418809326842, 1.000000000000000000, 0.9898214418809326842, 1.000000000000000000, 0.9898214418809326842, 1.000000000000000000, 0.9898214418809326842, 1.000000000000000000, 0.9898214418809326842, 1.000000000000000000, 0.9898214418809326842, 1.000000000000000000, 0.9898214418809326842, 1.000000000000000000, 0.9898214418809326842, 1.000000000000000000, 0.9898214418809326842, 1.000000000000000000, 0.9898214418809326842, 1.000000000000000000, 0.9898214418809326842, 1.000000000000000000, 0.9898214418809326842, 1.000000000000000000, 0.9898214418809326842, 1.000000000000000000, 0.9898214418809326842, 1.000000000000000000, 0.9898214418809326842, 1.000000000000000000, 0.9898214418809326842, 1.000000000000000000, 0.9898214418809326842, 1.000000000000000000, 0.9898214418809326842, 1.000000000000000000, 0.9898214418809326842, 1.000000000000000000, 0.9898214418809326842, 1.000000000000000000, 0.9898214418809326842, 1.000000000000000000, 0.9898214418809326842, 1.000000000000000000, 0.9898214418809326842, 1.000000000000000000, 0.9898214418809326842, 1.000000000000000000, 0.9898214418809326842, 1.000000000000000000, 0.9898214418809326842, 1.000000000000000000, 0.9898214418809326842, 1.000000000000000000, 0.9898214418809326842, 1.000000000000000000, 0.9898214418809326842, 1.000000000000000000, 0.9898214418809326842, 1.000000000000000000, 0.9898214418809326842, 1.000000000000000000, 0.9898214418809326842, 1.000000000000000000, 0.9898214418809326842, 1.000000000000000000, 0.9898214418809326842, 1.000000000000000000, 0.9898214418809326842, 1.000000000000000000, 0.9898214418809326842, 1.000000000000000000, 0.9898214418809326842, 1.000000000000000000, 0.9898214418809326842, 1.000000000000000000, 0.9898214418809326842, 1.000000000000000000, 0.9898214418809326842, 1.000000000000000000, 0.9898214418809326842, 1.000000000000000000, 0.9898214418809326842, 1.000000000000000000, 0.9898214418809326842, 1.000000000000000000, 0.9898214418809326842, 1.000000000000000000, 0.9898214418809326842, 1.000000000000000000, 0.9898214418809326842, 1.000000000000000000, 0.9898214418809326842, 1.000000000000000000, 0.9898214418809326842, 1.000000000000000000, 0.9898214418809326842, 1.000000000000000000, 0.9898214418809326842, 1.000000000000000000, 0.9898214418809326842, 1.000000000000000000, 0.9898214418809326842, 1.000000000000000000, 0.9898214418809326842, 1.000000000000000000, 0.9898214418809326842, 1.000000000000000000, 0.9898214418809326842, 1.000000000000000000, 0.9898214418809326842, 1.000000000000000000, 0.9898214418809326842, 1.000000000000000000, 0.9898214418809326842, 1.000000000000000000, 0.9898214418809326842, 1.000000000000000000, 0.9898214418809326842, 1.000000000000000000, 0.9898214418809326842, 1.000000000000000000, 0.9898214418809326842, 1.000000000000000000, 0.9898214418809326842, 1.000000000000000000, 0.9898214418809326842, 1.000000000000000000, 0.9898214418809326842, 1.000000000000000000, 0.9898214418809326842, 1.000000000000000000, 0.9898214418809326842, 1.000000000000000000, 0.9898214418809326842, 1.000000000000000000, 0.9898214418809326842, 1.000000000000000000, 0.9898214418809326842, 1.000000000000000000, 0.9898214418809326842, 1.000000000000000000, 0.9898214418809326842, 1.000000000000000000, 0.9898214418809326842, 1.000000000000000000, 0.9898214418809326842, 1.000000000000000000, 0.9898214418809326842, 1.000000000000000000, 0.9898214418809326842, 1.000000000000000000, 0.9898214418809326842, 1.000000000000000000, 0.9898214418809326842, 1.000000000000000000, 0.9898214418809326842, 1.000000000000000000, 0.9898214418809326842, 1.000000000000000000, 0.9898214418809326842, 1.000000000000000000, 0.9898214418809326842, 1.000000000000000000, 0.9898214418809326842, 1.000000000000000000, 0.9898214418809326842, 1.000000000000000000, 0.9898214418809326842, 1.000000000000000000, 0.9898214418809326842, 1.000000000000000000, 0.9898214418809326842, 1.000000000000000000, 0.9898214418809326842, 1.000000000000000000, 0.9898214418809326842, 1.000000000000000000, 0.9898214418809326842, 1.000000000000000000, 0.9898214418809326842, 1.000000000000000000, 0.9898214418809326842, 1.000000000000000000, 0.9898214418809326842, 1.000000000000000000, 0.9898214418809326842, 1.000000000000000000, 0.9898214418809326842, 1.000000000000000000, 0.9898214418809326842, 1.000000000000000000, 0.9898214418809326842, 1.000000000000000000, 0.9898214418809326842, 1.000000000000000000, 0.9898214418809326842, 1.000000000000000000, 0.9898214418809326842, 1.000000000000000000, 0.9898214418809326842, 1.000000000000000000, 0.9898214418809326842, 1.000000000000000000, 0.9898214418809326842, 1.000000000000000000, 0.9898214418809326842, 1.000000000000000000, 0.9898214418809326842, 1.000000000000000000, 0.9898214418809326842, 1.000000000000000000, 0.9898214418809326842, 1.000000000000000000, 0.9898214418809326842, 1.000000000000000000, 0.9898214418809326842, 1.000000000000000000, 0.9898214418809326842, 1.000000000000000000, 0.9898214418809326842, 1.000000000000000000, 0.9898214418809326842, 1.000000000000000000, 0.9898214418809326842, 1.000000000000000000, 0.9898214418809326842, 1.000000000000000000, 0.9898214418809326842, 1.000000000000000000, 0.9898214418809326842, 1.000000000000000000, 0.9898214418809326842, 1.000000000000000000, 0.9898214418809326842, 1.000000000000000000, 0.9898214418809326842, 1.000000000000000000, 0.9898214418809326842, 1.000000000000000000, 0.9898214418809326842, 1.000000000000000000, 0.9898214418809326842, 1.000000000000000000, 0.9898214418809326842, 1.000000000000000000, 0.9898214418809326842, 1.000000000000000000, 0.9898214418809326842, 1.000000000000000000, 0.9898214418809326842, 1.000000000000000000, 0.9898214418809326842, 1.000000000000000000, 0.9898214418809326842, 1.000000000000000000, 0.9898214418809326842, 1.000000000000000000, 0.9898214418809326842, 1.000000000000000000, 0.9898214418809326842, 1.000000000000000000, 0.9898214418809326842, 1.000000000000000000, 0.9898214418809326842, 1.000000000000000000, 0.9898214418809326842, 1.000000000000000000, 0.9898214418809326842, 1.000000000000000000, 0.9898214418809326842, 1.000000000000000000, 0.9898214418809326842, 1.000000000000000000, 0.9898214418809326842, 1.000000000000000000, 0.9898214418809326842, 1.000000000000000000, 0.9898214418809326842, 1.000000000000000000, 0.9898214418809326842, 1.000000000000000000, 0.9898214418809326842, 1.000000000000000000, 0.9898214418809326842, 1.000000000000000000, 0.9898214418809326842, 1.000000000000000000, 0.9898214418809326842, 1.000000000000000000, 0.9898214418809326842, 1.000000000000000000, 0.9898214418809326842, 1.000000000000000000, 0.9898214418809326842, 1.000000000000000000, 0.9898214418809326842, 1.000000000000000000, 0.9898214418809326842, 1.000000000000000000, 0.9898214418809326842, 1.000000000000000000, 0.9898214418809326842, 1.000000000000000000, 0.9898214418809326842, 1.000000000000000000, 0.9898214418809326842, 1.000000000000000000, 0.9898214418809326842, 1.000000000000000000, 0.9898214418809326842, 1.000000000000000000, 0.9898214418809326842, 1.000000000000000000, 0.9898214418809326842, 1.000000000000000000, 0.9898214418809326842, 1.000000000000000000, 0.9898214418809326842, 1.000000000000000000, 0.9898214418809326842, 1.000000000000000000, 0.9898214418809326842, 1.000000000000000000, 0.9898214418809326842, 1.000000000000000000, 0.9898214418809326842, 1.000000000000000000, 0.9898214418809326842, 1.000000000000000000, 0.9898214418809326842, 1.000000000000000000, 0.9898214418809326842, 1.000000000000000000, 0.9898214418809326842, 1.000000000000000000, 0.9898214418809326842, 1.000000000000000000, 0.9898214418809326842, 1.000000000000000000, 0.9898214418809326842, 1.000000000000000000, 0.9898214418809326842, 1.000000000000000000, 0.9898214418809326842, 1.000000000000000000, 0.9898214418809326842, 1.000000000000000000, 0.9898214418809326842, 1.000000000000000000, 0.9898214418809326842, 1.000000000000000000, 0.9898214418809326842, 1.000000000000000000, 0.9898214418809326842, 1.000000000000000000, 0.9898214418809326842, 1.000000000000000000, 0.9898214418809326842, 1.000000000000000000, 0.9898214418809326842, 1.000000000000000000, 0.9898214418809326842, 1.000000000000000000, 0.9898214418809326842, 1.000000000000000000, 0.9898214418809326842, 1.000000000000000000, 0.9898214418809326842, 1.000000000000000000, 0.9898214418809326842, 1.000000000000000000, 0.9898214418809326842, 1.000000000000000000, 0.9898214418809326842, 1.000000000000000000, 0.9898214418809326842, 1.000000000000000000, 0.9898214418809326842, 1.000000000000000000, 0.9898214418809326842, 1.000000000000000000, 0.9898214418809326842, 1.000000000000000000, 0.9898214418809326842, 1.000000000000000000, 0.9898214418809326842, 1.000000000000000000, 0.9898214418809326842, 1.000000000000000000, 0.9898214418809326842, 1.000000000000000000, 0.9898214418809326842, 1.000000000000000000, 0.9898214418809326842, 1.000000000000000000, 0.9898214418809326842, 1.000000000000000000, 0.9898214418809326842, 1.000000000000000000, 0.9898214418809326842, 1.000000000000000000, 0.9898214418809326842, 1.000000000000000000, 0.9898214418809326842, 1.000000000000000000, 0.9898214418809326842, 1.000000000000000000, 0.9898214418809326842, 1.000000000000000000, 0.9898214418809326842, 1.000000000000000000, 0.9898214418809326842, 1.000000000000000000, 0.9898214418809326842, 1.000000000000000000, 0.9898214418809326842, 1.000000000000000000, 0.9898214418809326842, 1.000000000000000000, 0.9898214418809326842, 1.000000000000000000, 0.9898214418809326842, 1.000000000000000000, 0.9898214418809326842, 1.000000000000000000, 0.9898214418809326842, 1.000000000000000000, 0.9898214418809326842, 1.000000000000000000, 0.9898214418809326842, 1.000000000000000000, 0.9898214418809326842, 1.000000000000000000, 0.9898214418809326842, 1.000000000000000000, 0.9898214418809326842, 1.000000000000000000, 0.9898214418809326842, 1.000000000000000000, 0.9898214418809326842, 1.000000000000000000, 0.9898214418809326842, 1.000000000000000000, 0.9898214418809326842, 1.000000000000000000, 0.9898214418809326842, 1.000000000000000000, 0.9898214418809326842, 1.000000000000000000, 0.9898214418809326842, 1.000000000000000000, 0.9898214418809326842, 1.000000000000000000, 0.9898214418809326842, 1.000000000000000000, 0.9898214418809326842, 1.000000000000000000, 0.9898214418809326842, 1.000000000000000000, 0.9898214418809326842, 1.000000000000000000, 0.9898214418809326842, 1.000000000000000000, 0.9898214418809326842, 1.000000000000000000, 0.9898214418809326842, 1.000000000000000000, 0.9898214418809326842, 1.000000000000000000, 0.9898214418809326842, 1.000000000000000000, 0.9898214418809326842, 1.000000000000000000, 0.9898214418809326842, 1.000000000000000000, 0.9898214418809326842, 1.000000000000000000, 0.9898214418809326842, 1.000000000000000000, 0.9898214418809326842, 1.000000000000000000, 0.9898214418809326842, 1.000000000000000000, 0.9898214418809326842, 1.000000000000000000, 0.9898214418809326842, 1.000000000000000000, 0.9898214418809326842, 1.000000000000000000, 0.9898214418809326842, 1.000000000000000000, 0.9898214418809326842, 1.000000000000000000, 0.9898214418809326842, 1.000000000000000000, 0.9898214418809326842, 1.000000000000000000, 0.9898214418809326842, 1.000000000000000000, 0.9898214418809326842, 1.000000000000000000, 0.9898214418809326842, 1.000000000000000000, 0.9898214418809326842, 1.000000000000000000, 0.9898214418809326842, 1.000000000000000000, 0.9898214418809326842, 1.000000000000000000, 0.9898214418809326842, 1.000000000000000000, 0.9898214418809326842, 1.000000000000000000, 0.9898214418809326842, 1.000000000000000000, 0.9898214418809326842, 1.000000000000000000, 0.9898214418809326842, 1.000000000000000000, 0.9898214418809326842, 1.000000000000000000, 0.9898214418809326842, 1.000000000000000000, 0.9898214418809326842, 1.000000000000000000, 0.9898214418809326842, 1.000000000000000000, 0.9898214418809326842, 1.000000000000000000, 0.9898214418809326842, 1.000000000000000000, 0.9898214418809326842, 1.000000000000000000, 0.9898214418809326842, 1.000000000000000000, 0.9898214418809326842, 1.000000000000000000, 0.9898214418809326842, 1.000000000000000000, 0.9898214418809326842, 1.000000000000000000, 0.9898214418809326842, 1.000000000000000000, 0.9898214418809326842, 1.000000000000000000, 0.9898214418809326842, 1.000000000000000000, 0.9898214418809326842, 1.000000000000000000, 0.9898214418809326842, 1.000000000000000000, 0.9898214418809326842, 1.000000000000000000, 0.9898214418809326842, 1.000000000000000000, 0.9898214418809326842, 1.000000000000000000, 0.9898214418809326842, 1.000000000000000000, 0.9898214418809326842, 1.000000000000000000, 0.9898214418809326842, 1.000000000000000000, 0.9898214418809326842, 1.000000000000000000, 0.9898214418809326842, 1.000000000000000000, 0.9898214418809326842, 1.000000000000000000, 0.9898214418809326842, 1.000000000000000000, 0.9898214418809326842, 1.000000000000000000, 0.9898214418809326842, 1.000000000000000000, 0.9898214418809326842, 1.000000000000000000, 0.9898214418809326842, 1.000000000000000000, 0.9898214418809326842, 1.000000000000000000, 0.9898214418809326842, 1.000000000000000000, 0.9898214418809326842, 1.000000000000000000, 0.9898214418809326842, 1.000000000000000000, 0.9898214418809326842, 1.000000000000000000, 0.9898214418809326842, 1.000000000000000000, 0.9898214418809326842, 1.000000000000000000, 0.9898214418809326842, 1.000000000000000000, 0.9961809353924466759, 0.9952277490961531914) ) ) 
 REPRESENTATION_ITEM ( '' )  SURFACE ( )  );
#14453 = CARTESIAN_POINT ( 'NONE',  ( 795.9930595647434757, -75.07832356259649487, -320.7433823573372820 ) ) ;
#14454 = CARTESIAN_POINT ( 'NONE',  ( 754.8072714833581358, -172.8164208402381234, -338.1981804954720587 ) ) ;
#14455 = CARTESIAN_POINT ( 'NONE',  ( 765.0180583372156207, -192.9982390220562820, -360.0135310231089534 ) ) ;
#14456 = CARTESIAN_POINT ( 'NONE',  ( 757.8323909638827445, -410.6346026584191122, 352.1044303154654358 ) ) ;
#14457 = AXIS2_PLACEMENT_3D ( 'NONE', #12121, #9095, #26203 ) ;
#14458 = CARTESIAN_POINT ( 'NONE',  ( 805.0032342141412300, -157.5436935675108998, -314.9967657858571783 ) ) ;
#14459 = VERTEX_POINT ( 'NONE', #45716 ) ;
#14460 = CARTESIAN_POINT ( 'NONE',  ( 764.8639956371174549, -128.0891481129655745, -319.7806653035542581 ) ) ;
#14461 = VERTEX_POINT ( 'NONE', #42236 ) ;
#14462 = CARTESIAN_POINT ( 'NONE',  ( 804.8461984189677878, -386.1908817542432075, -336.9566956441385628 ) ) ;
#14463 = CARTESIAN_POINT ( 'NONE',  ( 759.0159684113467620, -448.9181544815156144, 325.8855110935213020 ) ) ;
#14464 = CARTESIAN_POINT ( 'NONE',  ( 757.2208543904082489, -136.7146871989600072, 350.9844846989624330 ) ) ;
#14467 = CARTESIAN_POINT ( 'NONE',  ( 748.3538107759620743, -376.7146871989592682, 355.8262568251490165 ) ) ;
#14466 = DIRECTION ( 'NONE',  ( 0.000000000000000000, 0.000000000000000000, 1.000000000000000000 ) ) ;
#14465 = CARTESIAN_POINT ( 'NONE',  ( 779.9999999999992042, 126.4563064324884465, -339.9999999999999432 ) ) ;
#14468 = VERTEX_POINT ( 'NONE', #3443 ) ;
#14469 = CARTESIAN_POINT ( 'NONE',  ( 796.1575198192839480, -390.0090635724249069, -359.4546378042384163 ) ) ;
#14470 = CARTESIAN_POINT ( 'NONE',  ( 989.9999999999992042, 240.0000000000000568, -210.0000000000000000 ) ) ;
#14471 = CARTESIAN_POINT ( 'NONE',  ( 752.7379699480933368, -180.0090635724255890, -361.9858362298580232 ) ) ;
#14472 = CARTESIAN_POINT ( 'NONE',  ( 755.8990559732751535, -35.46360902697151829, 365.9055244015606831 ) ) ;
#14473 = AXIS2_PLACEMENT_3D ( 'NONE', #1486, #22736, #19728 ) ;
#14475 = CARTESIAN_POINT ( 'NONE',  ( 879.9999999999992042, 239.9999999999998863, -244.9999999999999716 ) ) ;
#14474 = CARTESIAN_POINT ( 'NONE',  ( 571.1634899080285095, 239.9999999999999432, -199.9999999999981526 ) ) ;
#14476 = CARTESIAN_POINT ( 'NONE',  ( 759.2295555964440155, -304.1692326535048210, -353.9708237608231229 ) ) ;
#14477 = DIRECTION ( 'NONE',  ( 0.000000000000000000, 0.000000000000000000, 1.000000000000000000 ) ) ;
#14479 = VECTOR ( 'NONE', #13740, 1000.000000000000114 ) ;
#14478 = CARTESIAN_POINT ( 'NONE',  ( 814.4686193811664907, -195.2817908451528410, -346.2056067578752732 ) ) ;
#14480 = PLANE ( 'NONE',  #34468 ) ;
#14481 = LINE ( 'NONE', #6843, #36346 ) ;
#14482 = VECTOR ( 'NONE', #32473, 999.9999999999998863 ) ;
#14483 = CARTESIAN_POINT ( 'NONE',  ( 755.8894580844503253, -351.8272453906068336, 332.3691319403863531 ) ) ;
#14484 = CARTESIAN_POINT ( 'NONE',  ( 804.1009440267234822, -335.4636090269705733, 314.0944755984392600 ) ) ;
#14485 = CARTESIAN_POINT ( 'NONE',  ( 767.7687537140311633, -191.9073299311471885, -372.7932403749916830 ) ) ;
#14486 = LINE ( 'NONE', #28566, #18745 ) ;
#14487 = CARTESIAN_POINT ( 'NONE',  ( 762.3223304703356007, 16.45630643248849267, -322.3223304703362828 ) ) ;
#14488 = VECTOR ( 'NONE', #2733, 1000.000000000000000 ) ;
#14489 = CARTESIAN_POINT ( 'NONE',  ( 749.5768839229115201, -156.5545181178802636, 358.0661480581553064 ) ) ;
#14490 = CARTESIAN_POINT ( 'NONE',  ( 781.2497674668890113, -84.35105083532374692, -375.3608509340180603 ) ) ;
#14491 = CARTESIAN_POINT ( 'NONE',  ( 808.0189434323515343, -134.0891481129655745, 319.0252816721025511 ) ) ;
#14492 = CARTESIAN_POINT ( 'NONE',  ( 796.7737145352015204, -332.6346026584195101, -370.7187646348536987 ) ) ;
#14493 = VECTOR ( 'NONE', #21717, 1000.000000000000000 ) ;
#14494 = EDGE_CURVE ( 'NONE', #20178, #8526, #43311, .T. ) ;
#14495 = CARTESIAN_POINT ( 'NONE',  ( 571.1634899080285095, 229.9999999999999432, -202.7499999999980105 ) ) ;
#14496 = PRODUCT_DEFINITION_SHAPE ( 'NONE', 'NONE',  #13196 ) ;
#14497 = DIRECTION ( 'NONE',  ( -1.000000000000000000, -0.000000000000000000, -0.000000000000000000 ) ) ;
#14498 = CARTESIAN_POINT ( 'NONE',  ( 788.8264449731200330, -237.1800572038742985, 363.6646147819171233 ) ) ;
#14499 = CARTESIAN_POINT ( 'NONE',  ( 762.1177392798416577, -450.5545181178793541, 309.8865473780659272 ) ) ;
#14500 = CARTESIAN_POINT ( 'NONE',  ( 744.9990715423526808, -402.3510508353228374, -341.2370466360926002 ) ) ;
#14501 = CARTESIAN_POINT ( 'NONE',  ( 751.9810565676468741, -434.0891481129646081, -360.9747183278973921 ) ) ;
#14502 = DIRECTION ( 'NONE',  ( -1.000000000000000000, 0.000000000000000000, 0.000000000000000000 ) ) ;
#14503 = CARTESIAN_POINT ( 'NONE',  ( 745.1769319972822814, 6.194403710130517382, 346.2694204179732083 ) ) ;
#14504 = VERTEX_POINT ( 'NONE', #24668 ) ;
#14505 = EDGE_CURVE ( 'NONE', #29708, #39647, #10832, .T. ) ;
#14506 = CARTESIAN_POINT ( 'NONE',  ( 805.9055244015594326, -195.6237781080506863, -315.8990559732753240 ) ) ;
#14507 = PLANE ( 'NONE',  #17974 ) ;
#14508 = CARTESIAN_POINT ( 'NONE',  ( 781.2497674668890113, -300.3510508353230080, 375.3608509340180603 ) ) ;
#14509 = CARTESIAN_POINT ( 'NONE',  ( 755.0636971347428243, -124.2709662947837899, 341.7834795799807353 ) ) ;
#14510 = EDGE_LOOP ( 'NONE', ( #15423, #40472, #28932, #35008 ) ) ;
#14511 = VECTOR ( 'NONE', #32420, 1000.000000000000000 ) ;
#14512 = CARTESIAN_POINT ( 'NONE',  ( 765.0180583372156207, -288.9982390220559978, 360.0135310231089534 ) ) ;
#14513 = AXIS2_PLACEMENT_3D ( 'NONE', #41900, #2635, #27565 ) ;
#14514 = CARTESIAN_POINT ( 'NONE',  ( 745.0891759886404770, -28.27096629478409540, -342.4968714119734159 ) ) ;
#14515 = CARTESIAN_POINT ( 'NONE',  ( 745.4481719005789273, -75.72551174932938522, 347.5162901302853697 ) ) ;
#14516 = ORIENTED_EDGE ( 'NONE', *, *, #37393, .T. ) ;
#14517 = CARTESIAN_POINT ( 'NONE',  ( 814.2805881961230625, -433.6454272087884760, -331.2368401574024119 ) ) ;
#14518 = ORIENTED_EDGE ( 'NONE', *, *, #28880, .F. ) ;
#14520 = EDGE_CURVE ( 'NONE', #17994, #29032, #6426, .T. ) ;
#14519 = EDGE_CURVE ( 'NONE', #9857, #31480, #45486, .T. ) ;
#14521 = CARTESIAN_POINT ( 'NONE',  ( 759.7806653035534055, -30.99823902205680071, 324.8639956371180801 ) ) ;
#14522 = CARTESIAN_POINT ( 'NONE',  ( 778.2165204200184689, -286.8164208402378677, -364.9363028652563230 ) ) ;
#14523 = VECTOR ( 'NONE', #11517, 1000.000000000000000 ) ;
#14525 = CARTESIAN_POINT ( 'NONE',  ( 803.8556311672234642, -297.6237781080502600, 365.6418435158340117 ) ) ;
#14524 = CARTESIAN_POINT ( 'NONE',  ( 782.4968714119720516, -394.8164208402374697, 305.0891759886411023 ) ) ;
#14526 = CARTESIAN_POINT ( 'NONE',  ( 751.2241431872005251, -88.16923265350555994, 359.9636004259367610 ) ) ;
#14527 = CARTESIAN_POINT ( 'NONE',  ( 754.7162404726377645, -278.7363362996980527, -339.4709603349214717 ) ) ;
#14528 = CARTESIAN_POINT ( 'NONE',  ( 762.3223304703356007, -295.5436935675105588, -322.3223304703362828 ) ) ;
#14529 = CARTESIAN_POINT ( 'NONE',  ( 756.3353852180820240, -437.9073299311464211, -331.1735550268787733 ) ) ;
#14530 = CARTESIAN_POINT ( 'NONE',  ( 762.3223304703356007, -103.5436935675111272, -322.3223304703362828 ) ) ;
#14531 = PLANE ( 'NONE',  #44652 ) ;
#14532 = CARTESIAN_POINT ( 'NONE',  ( 808.3070685750230950, -402.9982390220555430, 361.1904061080339261 ) ) ;
#14534 = CARTESIAN_POINT ( 'NONE',  ( 879.9999999999992042, 249.9999999999998295, -360.0000000000000000 ) ) ;
#14533 = CARTESIAN_POINT ( 'NONE',  ( 770.0084009877317612, 19.77989614203463375, 311.3857915150574627 ) ) ;
#14535 = CARTESIAN_POINT ( 'NONE',  ( 814.2805881961230625, -97.64542720878949922, -331.2368401574024119 ) ) ;
#14536 = DIRECTION ( 'NONE',  ( 1.892425610156518354E-16, 1.000000000000000000, -0.000000000000000000 ) ) ;
#14537 = DIRECTION ( 'NONE',  ( 0.000000000000000000, 0.000000000000000000, -1.000000000000000000 ) ) ;
#14538 = CARTESIAN_POINT ( 'NONE',  ( 754.7162404726377645, -254.7363362996981095, 339.4709603349214717 ) ) ;
#14539 = CARTESIAN_POINT ( 'NONE',  ( 785.3141322388236176, -141.7255117493291721, 364.4286716492789537 ) ) ;
#14540 = ORIENTED_EDGE ( 'NONE', *, *, #42688, .T. ) ;
#14541 = CARTESIAN_POINT ( 'NONE',  ( 755.8894580844503253, -63.82724539060779279, -332.3691319403863531 ) ) ;
#14542 = CARTESIAN_POINT ( 'NONE',  ( 792.2312462859673587, -107.9073299311474727, -307.2067596250082602 ) ) ;
#14543 = CARTESIAN_POINT ( 'NONE',  ( 780.5290396650775619, -324.3510508353229511, 365.2837595273619513 ) ) ;
#14544 = DIRECTION ( 'NONE',  ( 0.000000000000000000, 0.000000000000000000, 1.000000000000000000 ) ) ;
#14545 = EDGE_CURVE ( 'NONE', #1111, #23251, #7593, .T. ) ;
#14546 = CARTESIAN_POINT ( 'NONE',  ( 760.0363995740630116, -34.91815448151697154, 368.7758568127991907 ) ) ;
#14548 = VECTOR ( 'NONE', #12416, 1000.000000000000000 ) ;
#14547 = CARTESIAN_POINT ( 'NONE',  ( 787.5162901302840055, -227.3618753856925707, -305.4481719005792684 ) ) ;
#14549 = ADVANCED_FACE ( 'NONE', ( #21669 ), #13604, .F. ) ;
#14550 = CARTESIAN_POINT ( 'NONE',  ( 804.9363028652555840, -64.27096629478397460, 338.2165204200192079 ) ) ;
#14551 = CARTESIAN_POINT ( 'NONE',  ( 759.9999999999992042, -462.9681489794448339, 370.0000000000000568 ) ) ;
#14552 = CARTESIAN_POINT ( 'NONE',  ( 747.3154664389472828, -307.9874144716866340, -326.4474001241230781 ) ) ;
#14553 = AXIS2_PLACEMENT_3D ( 'NONE', #26378, #26146, #15755 ) ;
#14554 = CARTESIAN_POINT ( 'NONE',  ( 768.9521613784389729, -441.8272453906066630, 373.2346286133773106 ) ) ;
#14555 = CARTESIAN_POINT ( 'NONE',  ( 745.4481719005789273, -315.7255117493286320, -347.5162901302853129 ) ) ;
#14556 = FACE_OUTER_BOUND ( 'NONE', #24700, .T. ) ;
#14557 = CARTESIAN_POINT ( 'NONE',  ( 759.2295555964440155, -376.1692326535046504, 353.9708237608231229 ) ) ;
#14558 = CARTESIAN_POINT ( 'NONE',  ( 777.4774526936600978, -34.27096629478407408, 304.7301800767028226 ) ) ;
#14559 = ADVANCED_FACE ( 'NONE', ( #17539 ), #24216, .F. ) ;
#14560 = CARTESIAN_POINT ( 'NONE',  ( 804.6798772138708955, -399.7255117493283478, -334.6312213355107019 ) ) ;
#14561 = AXIS2_PLACEMENT_3D ( 'NONE', #22071, #25074, #28554 ) ;
#14562 = EDGE_CURVE ( 'NONE', #34298, #30700, #21220, .T. ) ;
#14563 = CARTESIAN_POINT ( 'NONE',  ( 759.2295555964440155, -40.16923265350570915, 353.9708237608231229 ) ) ;
#14564 = CARTESIAN_POINT ( 'NONE',  ( 746.0683387631852383, -91.44195992623282621, -331.3260364891676204 ) ) ;
#14565 = CARTESIAN_POINT ( 'NONE',  ( 810.1134526219336749, -200.5328690171415644, 357.8822607201570349 ) ) ;
#14566 = CARTESIAN_POINT ( 'NONE',  ( 768.0187753319979720, -8.634602658420517329, 318.0580252608186242 ) ) ;
#14567 = ORIENTED_EDGE ( 'NONE', *, *, #4052, .F. ) ;
#14568 = CARTESIAN_POINT ( 'NONE',  ( 754.8983024940795303, -210.8965053807778816, -336.9254006560228163 ) ) ;
#14569 = CARTESIAN_POINT ( 'NONE',  ( 756.5762568750052424, -195.1800572038744974, 348.7366044899774238 ) ) ;
#14570 = CARTESIAN_POINT ( 'NONE',  ( 815.0009284576459549, -30.35105083532391390, -338.7629533639073429 ) ) ;
#14571 = CARTESIAN_POINT ( 'NONE',  ( 778.1981804954715471, -322.2709662947830793, 314.8072714833591021 ) ) ;
#14572 = CARTESIAN_POINT ( 'NONE',  ( 807.4745771775690173, -452.9681489794449476, -340.5093320845589346 ) ) ;
#14573 = DIRECTION ( 'NONE',  ( -1.000000000000000000, -0.000000000000000000, -0.000000000000000000 ) ) ;
#14574 = EDGE_CURVE ( 'NONE', #11372, #41096, #44024, .T. ) ;
#14575 = EDGE_LOOP ( 'NONE', ( #12774, #23728, #18552 ) ) ;
#14576 = CARTESIAN_POINT ( 'NONE',  ( 800.7704444035546203, -52.16923265350567362, 326.0291762391768771 ) ) ;
#14578 = AXIS2_PLACEMENT_3D ( 'NONE', #34050, #30591, #16509 ) ;
#14577 = CARTESIAN_POINT ( 'NONE',  ( 771.3260364891663130, -355.6454272087887603, -306.0683387631859773 ) ) ;
#14579 = EDGE_CURVE ( 'NONE', #22309, #27668, #4803, .T. ) ;
#14580 = CARTESIAN_POINT ( 'NONE',  ( 814.5518280994195948, -303.7255117493286889, 332.4837098697145166 ) ) ;
#14581 = CARTESIAN_POINT ( 'NONE',  ( 771.2368401574024119, 10.55804007376686826, 374.2805881961240857 ) ) ;
#14582 = CARTESIAN_POINT ( 'NONE',  ( 773.4516893846965786, -187.6454272087892434, -315.8398074228977066 ) ) ;
#14583 = CARTESIAN_POINT ( 'NONE',  ( 797.8594530101008786, -157.5436935675108998, -322.1405469898980982 ) ) ;
#14584 = CARTESIAN_POINT ( 'NONE',  ( 778.1981804954715471, -346.2709662947830225, -314.8072714833591021 ) ) ;
#14585 = ORIENTED_EDGE ( 'NONE', *, *, #27442, .T. ) ;
#14586 = CARTESIAN_POINT ( 'NONE',  ( 764.0069404352550464, 8.921676437403235127, -359.2566176426627180 ) ) ;
#14587 = AXIS2_PLACEMENT_3D ( 'NONE', #25052, #44415, #33800 ) ;
#14588 = CARTESIAN_POINT ( 'NONE',  ( 747.2067596250078623, -291.1800572038741848, 352.2312462859687230 ) ) ;
#14589 = FACE_OUTER_BOUND ( 'NONE', #12288, .T. ) ;
#14590 = CARTESIAN_POINT ( 'NONE',  ( 784.1219089521767955, -213.2817908451527842, 315.0488828828318333 ) ) ;
#14591 = CARTESIAN_POINT ( 'NONE',  ( 776.9566956441375396, -324.8965053807775121, 364.8461984189686405 ) ) ;
#14592 = DIRECTION ( 'NONE',  ( 0.000000000000000000, -1.000000000000000000, 0.000000000000000000 ) ) ;
#14593 = CARTESIAN_POINT ( 'NONE',  ( 755.8894580844503253, -159.8272453906075157, 332.3691319403863531 ) ) ;
#14594 = CARTESIAN_POINT ( 'NONE',  ( 795.1360043628807261, -44.08914811296584446, 360.2193346964456282 ) ) ;
#14595 = ORIENTED_EDGE ( 'NONE', *, *, #44639, .F. ) ;
#14596 = CARTESIAN_POINT ( 'NONE',  ( 783.7953271457878373, -416.1908817542430938, -375.1787889125761239 ) ) ;
#14597 = CARTESIAN_POINT ( 'NONE',  ( 811.0346526505617248, 9.365397341579424051, -323.0537975583478101 ) ) ;
#14598 = CARTESIAN_POINT ( 'NONE',  ( 746.4236121716829757, -255.8272453906072315, 328.8385539511384650 ) ) ;
#14599 = CARTESIAN_POINT ( 'NONE',  ( 754.8983024940795303, -186.8965053807779668, 336.9254006560228163 ) ) ;
#14600 = CARTESIAN_POINT ( 'NONE',  ( 755.0636971347428243, -364.2709662947830793, -341.7834795799807353 ) ) ;
#14601 = ADVANCED_FACE ( 'NONE', ( #8065 ), #29309, .F. ) ;
#14602 = CARTESIAN_POINT ( 'NONE',  ( 797.6776695296629214, 4.456306432488530866, 357.6776695296636603 ) ) ;
#14603 = DIRECTION ( 'NONE',  ( 0.000000000000000000, 0.3826834323650836200, 0.9238795325112892920 ) ) ;
#14604 = CARTESIAN_POINT ( 'NONE',  ( 790.9844846989617508, -238.3726999360617640, -317.2208543904092721 ) ) ;
#14605 = EDGE_CURVE ( 'NONE', #10227, #5810, #1107, .T. ) ;
#14606 = CARTESIAN_POINT ( 'NONE',  ( 754.9967657858570647, -25.54369356751136877, 365.0032342141425374 ) ) ;
#14607 = CARTESIAN_POINT ( 'NONE',  ( 745.4481719005789273, -99.72551174932928575, 347.5162901302853129 ) ) ;
#14608 = CARTESIAN_POINT ( 'NONE',  ( -37.63011601220122770, -512.9681489794448908, -339.9999999999999432 ) ) ;
#14609 = CARTESIAN_POINT ( 'NONE',  ( 814.2001403089898304, -401.3618753856920307, -347.4397851343538264 ) ) ;
#14610 = FACE_OUTER_BOUND ( 'NONE', #6674, .T. ) ;
#14611 = CARTESIAN_POINT ( 'NONE',  ( 778.7629533639073998, -344.7363362996978253, 375.0009284576466371 ) ) ;
#14612 = CARTESIAN_POINT ( 'NONE',  ( 1238.921997096861332, 430.0000000000002842, -320.0000000000000568 ) ) ;
#14613 = CARTESIAN_POINT ( 'NONE',  ( 751.9810565676468741, -314.0891481129650629, 360.9747183278973921 ) ) ;
#14614 = CARTESIAN_POINT ( 'NONE',  ( 763.2262854647970016, -56.63460265842036279, -309.2812353651462445 ) ) ;
#14615 = EDGE_CURVE ( 'NONE', #24672, #40820, #14982, .T. ) ;
#14616 = CARTESIAN_POINT ( 'NONE',  ( 762.3223304703356007, -295.5436935675105588, -322.3223304703362828 ) ) ;
#14617 = DIRECTION ( 'NONE',  ( 0.000000000000000000, 0.000000000000000000, -1.000000000000000000 ) ) ;
#14618 = CARTESIAN_POINT ( 'NONE',  ( 792.1044303154645831, -420.4527844766009252, 317.8323909638837677 ) ) ;
#14619 = CARTESIAN_POINT ( 'NONE',  ( 763.8424801807145741, -186.0090635724255890, 320.5453621957614700 ) ) ;
#14620 = CARTESIAN_POINT ( 'NONE',  ( 804.1009440267234822, -47.46360902697148987, -314.0944755984392600 ) ) ;
#14621 = CARTESIAN_POINT ( 'NONE',  ( 757.2208543904082489, -88.71468719896009247, -350.9844846989624330 ) ) ;
#14622 = CARTESIAN_POINT ( 'NONE',  ( 810.1134526219336749, -104.5328690171418913, 357.8822607201570349 ) ) ;
#14623 = CARTESIAN_POINT ( 'NONE',  ( 762.1405469898973024, -409.5436935675101608, 357.8594530101016176 ) ) ;
#14624 = VECTOR ( 'NONE', #42101, 1000.000000000000000 ) ;
#14626 = VERTEX_POINT ( 'NONE', #22127 ) ;
#14625 = CARTESIAN_POINT ( 'NONE',  ( 799.4546378042377910, -105.0783235625964096, -356.1575198192848006 ) ) ;
#14627 = CARTESIAN_POINT ( 'NONE',  ( 791.9812246680005501, -92.63460265842026331, -361.9419747391813189 ) ) ;
#14628 = CARTESIAN_POINT ( 'NONE',  ( 798.7617431975189675, -411.6237781080499758, -323.0428371773161871 ) ) ;
#14630 = CARTESIAN_POINT ( 'NONE',  ( 771.1735550268780344, -225.1800572038743553, 316.3353852180828198 ) ) ;
#14629 = CARTESIAN_POINT ( 'NONE',  ( 774.6312213355099630, -215.3618753856925423, 364.6798772138717482 ) ) ;
#14631 = CARTESIAN_POINT ( 'NONE',  ( 810.1134526219336749, -416.5328690171409107, -357.8822607201570349 ) ) ;
#14632 = CARTESIAN_POINT ( 'NONE',  ( 939.9999999999993179, -590.0000000000001137, -201.9999999999998579 ) ) ;
#14633 = ORIENTED_EDGE ( 'NONE', *, *, #32926, .T. ) ;
#14634 = CARTESIAN_POINT ( 'NONE',  ( 795.1360043628807261, -428.0891481129644944, 360.2193346964456282 ) ) ;
#14635 = EDGE_LOOP ( 'NONE', ( #25745, #32042, #29120, #37724, #23709, #5933 ) ) ;
#14636 = CARTESIAN_POINT ( 'NONE',  ( 758.8095938919642549, -248.0891481129651481, -311.6929314249763365 ) ) ;
#14637 = CARTESIAN_POINT ( 'NONE',  ( 767.6429770376291799, -201.1800572038744690, 306.8695393053162093 ) ) ;
#14638 = CARTESIAN_POINT ( 'NONE',  ( 787.5531968255692163, -261.8272453906071746, 316.1348686366205811 ) ) ;
#14639 = CARTESIAN_POINT ( 'NONE',  ( 755.0488828828309806, -377.8055962898682765, 344.1219089521771934 ) ) ;
#14640 = EDGE_LOOP ( 'NONE', ( #11264, #14585, #12639, #40415 ) ) ;
#14641 = CARTESIAN_POINT ( 'NONE',  ( 780.5236548040995785, -68.73633629969867798, -314.9735926884559944 ) ) ;
#14642 = CARTESIAN_POINT ( 'NONE',  ( 771.2633955100217236, -239.9073299311470748, -363.4237431249939618 ) ) ;
#14643 = VERTEX_POINT ( 'NONE', #8272 ) ;
#14644 = CARTESIAN_POINT ( 'NONE',  ( 788.8264449731200330, -357.1800572038739006, -363.6646147819171233 ) ) ;
#14645 = CARTESIAN_POINT ( 'NONE',  ( 759.7806653035534055, -54.99823902205672255, -324.8639956371180801 ) ) ;
#14646 = CARTESIAN_POINT ( 'NONE',  ( 793.2243759319678702, -218.5328690171414792, 318.4439275373583200 ) ) ;
#14647 = DIRECTION ( 'NONE',  ( -0.000000000000000000, 1.000000000000000000, -0.000000000000000000 ) ) ;
#14648 = DIRECTION ( 'NONE',  ( 1.000000000000000000, 0.000000000000000000, 0.000000000000000000 ) ) ;
#14649 = EDGE_LOOP ( 'NONE', ( #32184, #23487, #38137, #21874, #43689, #32856, #21893 ) ) ;
#14650 = CARTESIAN_POINT ( 'NONE',  ( 759.9864689768902508, -2.089148112965993231, -354.9819416627836404 ) ) ;
#14651 = LINE ( 'NONE', #26323, #34401 ) ;
#14652 = EDGE_LOOP ( 'NONE', ( #23449, #20893 ) ) ;
#14653 = CARTESIAN_POINT ( 'NONE',  ( 791.0478386215596629, -285.8272453906071178, -306.7653713866226326 ) ) ;
#14654 = CARTESIAN_POINT ( 'NONE',  ( 750.9282345327678740, -184.9181544815165239, 319.8311093483690115 ) ) ;
#14655 = CIRCLE ( 'NONE', #45607, 8.024999999999948841 ) ;
#14657 = CARTESIAN_POINT ( 'NONE',  ( 785.3141322388236176, -261.7255117493288026, -364.4286716492789537 ) ) ;
#14656 = DIRECTION ( 'NONE',  ( -0.000000000000000000, -0.000000000000000000, -1.000000000000000000 ) ) ;
#14658 = CARTESIAN_POINT ( 'NONE',  ( 804.1105419155481968, -99.82724539060768620, -347.6308680596136469 ) ) ;
#14659 = CARTESIAN_POINT ( 'NONE',  ( 791.0478386215596629, -381.8272453906068336, 306.7653713866226326 ) ) ;
#14660 = DIRECTION ( 'NONE',  ( 0.000000000000000000, 0.000000000000000000, 1.000000000000000000 ) ) ;
#14661 = CARTESIAN_POINT ( 'NONE',  ( 786.2056067578752163, -11.80559628986942577, -374.4686193811670023 ) ) ;
#14662 = CARTESIAN_POINT ( 'NONE',  ( 782.5225473063383106, -310.2709662947832499, -375.2698199232970637 ) ) ;
#14663 = DIRECTION ( 'NONE',  ( 1.000000000000000000, 0.000000000000000000, -0.000000000000000000 ) ) ;
#14664 = CARTESIAN_POINT ( 'NONE',  ( 794.9819416627830151, -12.99823902205686821, 319.9864689768909898 ) ) ;
#14665 = CARTESIAN_POINT ( 'NONE',  ( 791.0478386215596629, -261.8272453906071746, 306.7653713866226326 ) ) ;
#14666 = CARTESIAN_POINT ( 'NONE',  ( 744.8212110874229666, -210.8965053807778816, -336.2046728542121627 ) ) ;
#14667 = CARTESIAN_POINT ( 'NONE',  ( 801.1904061080336987, -212.0891481129652902, 368.3070685750235498 ) ) ;
#14668 = CARTESIAN_POINT ( 'NONE',  ( 793.3938497862117174, -453.0432664090020012, -372.3358127763067955 ) ) ;
#14669 = CARTESIAN_POINT ( 'NONE',  ( -728.8365100919714905, 240.0000000000001990, -197.2499999999891998 ) ) ;
#14670 = CARTESIAN_POINT ( 'NONE',  ( 778.1981804954714335, -322.2709662947830225, 314.8072714833589885 ) ) ;
#14671 = CARTESIAN_POINT ( 'NONE',  ( 759.0159684113467620, -88.91815448151682233, 325.8855110935213020 ) ) ;
#14672 = CARTESIAN_POINT ( 'NONE',  ( 755.5913626894240451, -85.64542720878952764, 346.6156483768012890 ) ) ;
#14673 = CARTESIAN_POINT ( 'NONE',  ( 773.3843516231979720, 10.55804007376686826, -364.4086373105754433 ) ) ;
#14674 = CARTESIAN_POINT ( 'NONE',  ( 799.9999999999993179, 166.4563064324884465, -319.9999999999999432 ) ) ;
#14675 = CARTESIAN_POINT ( 'NONE',  ( 919.9999999999993179, 219.9999999999998863, 360.0000000000000000 ) ) ;
#14677 = CARTESIAN_POINT ( 'NONE',  ( 755.3201227861273992, -363.7255117493284047, 345.3687786644892981 ) ) ;
#14676 = CARTESIAN_POINT ( 'NONE',  ( 769.1273215169530886, -166.7146871989598367, 317.4527132478988847 ) ) ;
#14678 = ORIENTED_EDGE ( 'NONE', *, *, #40553, .F. ) ;
#14679 = CARTESIAN_POINT ( 'NONE',  ( 760.5453621957607311, -285.0783235625958127, -323.8424801807151425 ) ) ;
#14680 = CARTESIAN_POINT ( 'NONE',  ( 762.3223304703356007, -127.5436935675110561, 322.3223304703362828 ) ) ;
#14681 = CARTESIAN_POINT ( 'NONE',  ( 813.9316612368132837, -295.4419599262320730, -348.6739635108323228 ) ) ;
#14682 = DIRECTION ( 'NONE',  ( -1.000000000000000000, 0.000000000000000000, 0.000000000000000000 ) ) ;
#14683 = CARTESIAN_POINT ( 'NONE',  ( 754.0944755984390895, -399.6237781080500326, 364.1009440267246760 ) ) ;
#14684 = ORIENTED_EDGE ( 'NONE', *, *, #39673, .T. ) ;
#14685 = CARTESIAN_POINT ( 'NONE',  ( 800.2193346964447755, -330.9982390220558273, 355.1360043628815788 ) ) ;
#14686 = CIRCLE ( 'NONE', #19805, 10.00000000000000888 ) ;
#14687 = CARTESIAN_POINT ( 'NONE',  ( 772.3691319403857278, -71.26014174441469606, -315.8894580844506663 ) ) ;
#14688 = CARTESIAN_POINT ( 'NONE',  ( 785.3141322388236176, -165.7255117493291152, -364.4286716492789537 ) ) ;
#14689 = CARTESIAN_POINT ( 'NONE',  ( 771.1735550268778070, -201.1800572038744690, -316.3353852180827630 ) ) ;
#14690 = CARTESIAN_POINT ( 'NONE',  ( 771.2633955100217236, -431.9073299311464211, 363.4237431249939618 ) ) ;
#14691 = CARTESIAN_POINT ( 'NONE',  ( 751.9810565676468741, -146.0891481129655176, -360.9747183278973921 ) ) ;
#14692 = ORIENTED_EDGE ( 'NONE', *, *, #26628, .T. ) ;
#14693 = CARTESIAN_POINT ( 'NONE',  ( 778.1981804954715471, -154.2709662947836762, -314.8072714833591021 ) ) ;
#14694 = ORIENTED_EDGE ( 'NONE', *, *, #30089, .F. ) ;
#14695 = CARTESIAN_POINT ( 'NONE',  ( 798.5707757039680246, -389.4636090269704027, -356.7845633553585003 ) ) ;
#14696 = CARTESIAN_POINT ( 'NONE',  ( 767.8955696845333705, -0.4527844766023628176, 362.1676090361162323 ) ) ;
#14697 = CARTESIAN_POINT ( 'NONE',  ( 811.0346526505616112, -230.6346026584197659, 323.0537975583477532 ) ) ;
#14698 = CARTESIAN_POINT ( 'NONE',  ( 794.1144889064781864, -130.1692326535054463, 360.9840315886528401 ) ) ;
#14701 = CARTESIAN_POINT ( 'NONE',  ( 813.2346286133761168, -389.2601417444136018, 328.9521613784389160 ) ) ;
#14700 = LINE ( 'NONE', #10764, #25504 ) ;
#14699 = CARTESIAN_POINT ( 'NONE',  ( 441.1634899080286232, 256.4999999999999432, -199.9999999999972431 ) ) ;
#14702 = ORIENTED_EDGE ( 'NONE', *, *, #10732, .F. ) ;
#14703 = CARTESIAN_POINT ( 'NONE',  ( 790.0220218866281812, -391.0999726633340288, -363.2186876482849129 ) ) ;
#14704 = CARTESIAN_POINT ( 'NONE',  ( -786.4999999999993179, -512.9681489794448908, -350.0000000000000000 ) ) ;
#14705 = CARTESIAN_POINT ( 'NONE',  ( 754.3581564841646241, -185.4636090269710280, -316.1443688327762516 ) ) ;
#14706 = CARTESIAN_POINT ( 'NONE',  ( 793.5525998758768083, -31.09997266333516919, 372.6845335610516941 ) ) ;
#14708 = DIRECTION ( 'NONE',  ( 1.000000000000000000, 0.000000000000000000, 0.000000000000000000 ) ) ;
#14707 = DIRECTION ( 'NONE',  ( 1.892425610156518354E-16, 1.000000000000000000, -0.000000000000000000 ) ) ;
#14709 = CARTESIAN_POINT ( 'NONE',  ( 803.8651313633788504, -341.2601417444138292, -332.4468031744301015 ) ) ;
#14710 = CARTESIAN_POINT ( 'NONE',  ( 795.1360043628807261, -452.0891481129646650, -360.2193346964456282 ) ) ;
#14711 = CARTESIAN_POINT ( 'NONE',  ( 799.9636004259356241, -190.9181544815164955, -311.2241431872006956 ) ) ;
#14712 = DIRECTION ( 'NONE',  ( -0.000000000000000000, 1.000000000000000000, -0.000000000000000000 ) ) ;
#14713 = DIRECTION ( 'NONE',  ( -1.000000000000000000, 0.000000000000000000, 0.000000000000000000 ) ) ;
#14714 = CARTESIAN_POINT ( 'NONE',  ( 775.8780910478218402, -369.2817908451523294, 364.9511171171680530 ) ) ;
#14715 = CARTESIAN_POINT ( 'NONE',  ( 745.7194118038753459, -349.6454272087887603, 348.7631598425976449 ) ) ;
#14716 = EDGE_CURVE ( 'NONE', #45077, #33694, #40140, .T. ) ;
#14717 = CARTESIAN_POINT ( 'NONE',  ( 804.7487373415286811, -211.5436935675107861, -364.7487373415288516 ) ) ;
#14718 = DIRECTION ( 'NONE',  ( 0.000000000000000000, 0.000000000000000000, -1.000000000000000000 ) ) ;
#14719 = CARTESIAN_POINT ( 'NONE',  ( 756.3353852180819104, -29.90732993114771787, -331.1735550268788302 ) ) ;
#14720 = AXIS2_PLACEMENT_3D ( 'NONE', #14086, #31403, #7163 ) ;
#14721 = CARTESIAN_POINT ( 'NONE',  ( 771.3260364891663130, -139.6454272087893571, 306.0683387631859773 ) ) ;
#14722 = CARTESIAN_POINT ( 'NONE',  ( 798.0661480581538854, -98.53286901714187707, -309.5768839229118043 ) ) ;
#14723 = CARTESIAN_POINT ( 'NONE',  ( 800.9747183278959710, -108.9982390220565804, 311.9810565676471583 ) ) ;
#14724 = CARTESIAN_POINT ( 'NONE',  ( 745.4481719005789273, -339.7255117493285184, -347.5162901302853129 ) ) ;
#14725 = DIRECTION ( 'NONE',  ( 0.000000000000000000, 0.000000000000000000, 1.000000000000000000 ) ) ;
#14726 = CARTESIAN_POINT ( 'NONE',  ( 773.4999999999993179, -365.3551492539851893, -8.132432514707076621 ) ) ;
#14727 = CARTESIAN_POINT ( 'NONE',  ( 778.1981804954714335, -226.2709662947834204, 314.8072714833589885 ) ) ;
#14728 = CARTESIAN_POINT ( 'NONE',  ( 815.3608509340175488, -458.7363362996973706, 341.2497674668889545 ) ) ;
#14729 = CARTESIAN_POINT ( 'NONE',  ( 756.1443688327750579, -405.6237781080500326, -314.3581564841659315 ) ) ;
#14730 =( BOUNDED_CURVE ( )  B_SPLINE_CURVE ( 2, ( #9790, #9341, #34506, #27564, #13491, #23411, #37513 ),
 .UNSPECIFIED., .F., .T. ) 
 B_SPLINE_CURVE_WITH_KNOTS ( ( 3, 2, 2, 3 ),
 ( 0.000000000000000000, 0.002272727272727272617, 0.004545454545454545234, 0.006081874955971018626 ),
 .UNSPECIFIED. ) 
 CURVE ( )  GEOMETRIC_REPRESENTATION_ITEM ( )  RATIONAL_B_SPLINE_CURVE ( ( 0.5000002209606653203, 0.4949109396520706694, 0.5000002209606653203, 0.4949109396520706694, 0.5000002209606653203, 0.4965597396626160176, 0.4977709609702910543 ) ) 
 REPRESENTATION_ITEM ( '' )  );
#14731 = CARTESIAN_POINT ( 'NONE',  ( 745.4481719005789273, -435.7255117493282341, -347.5162901302853129 ) ) ;
#14732 = CARTESIAN_POINT ( 'NONE',  ( 1007.605605532488426, -112.8054336623104348, 752.6593748957919843 ) ) ;
#14733 = CARTESIAN_POINT ( 'NONE',  ( 758.0141637701419768, -39.07832356259662276, 367.2620300519063790 ) ) ;
#14734 = VERTEX_POINT ( 'NONE', #35761 ) ;
#14735 = CARTESIAN_POINT ( 'NONE',  ( 788.7366044899766848, -11.90732993114778182, 316.5762568750059813 ) ) ;
#14736 = CARTESIAN_POINT ( 'NONE',  ( 791.1614460488616487, -203.2601417444143124, -373.5763878283158874 ) ) ;
#14737 = CARTESIAN_POINT ( 'NONE',  ( 815.1787889125755555, -318.8965053807775121, 343.7953271457877804 ) ) ;
#14738 = CARTESIAN_POINT ( 'NONE',  ( 781.7834795799800531, -154.8164208402382371, 315.0636971347436202 ) ) ;
#14739 = ORIENTED_EDGE ( 'NONE', *, *, #10609, .T. ) ;
#14740 = CARTESIAN_POINT ( 'NONE',  ( 794.9819416627830151, -300.9982390220559409, 319.9864689768909898 ) ) ;
#14741 = CARTESIAN_POINT ( 'NONE',  ( 759.0252816721024374, -48.99823902205675807, -368.0189434323527280 ) ) ;
#14742 = CARTESIAN_POINT ( 'NONE',  ( 812.7932403749906598, -87.18005720387481006, 327.7687537140311633 ) ) ;
#14743 = ORIENTED_EDGE ( 'NONE', *, *, #6040, .T. ) ;
#14744 = CARTESIAN_POINT ( 'NONE',  ( 812.3518521366052028, -457.0999726633339151, -326.5853460496235243 ) ) ;
#14745 = AXIS2_PLACEMENT_3D ( 'NONE', #12786, #39466, #18898 ) ;
#14746 = ORIENTED_EDGE ( 'NONE', *, *, #7185, .T. ) ;
#14747 = CONTEXT_DEPENDENT_SHAPE_REPRESENTATION ( #30525, #37660 ) ;
#14749 = CARTESIAN_POINT ( 'NONE',  ( 766.0291762391763086, -322.9181544815161260, 360.7704444035551319 ) ) ;
#14748 = CARTESIAN_POINT ( 'NONE',  ( 755.3201227861273992, -51.72551174932946338, 345.3687786644892981 ) ) ;
#14750 = CARTESIAN_POINT ( 'NONE',  ( 801.9419747391806368, -282.4527844766014937, -351.9812246680014027 ) ) ;
#14752 = CARTESIAN_POINT ( 'NONE',  ( 808.7758568127978833, -292.1692326535048210, 320.0363995740631822 ) ) ;
#14751 = CARTESIAN_POINT ( 'NONE',  ( 749.2812353651451076, -390.4527844766011526, 323.2262854647983090 ) ) ;
#14753 = CARTESIAN_POINT ( 'NONE',  ( 758.4439275373578084, -300.5545181178797520, -353.2243759319684386 ) ) ;
#14754 = CARTESIAN_POINT ( 'NONE',  ( 804.9363028652555840, -304.2709662947832499, -338.2165204200192079 ) ) ;
#14755 = CARTESIAN_POINT ( 'NONE',  ( 762.3223304703356007, -439.5436935675101040, -322.3223304703362828 ) ) ;
#14756 = CARTESIAN_POINT ( 'NONE',  ( 765.0180583372156207, -120.9982390220565378, -360.0135310231089534 ) ) ;
#14757 = EDGE_CURVE ( 'NONE', #43956, #15632, #29067, .T. ) ;
#14758 = CARTESIAN_POINT ( 'NONE',  ( 786.4999999999993179, -544.8427095258973623, -350.0000000000000000 ) ) ;
#14759 = ORIENTED_EDGE ( 'NONE', *, *, #17608, .F. ) ;
#14760 = CARTESIAN_POINT ( 'NONE',  ( 804.7487373415286811, -403.5436935675101608, 364.7487373415288516 ) ) ;
#14762 = CARTESIAN_POINT ( 'NONE',  ( -829.9999999999992042, 290.0000000000001137, -244.9999999999999716 ) ) ;
#14761 = DIRECTION ( 'NONE',  ( 0.000000000000000000, -0.6594541114781790059, 0.7517448203044204691 ) ) ;
#14763 = CARTESIAN_POINT ( 'NONE',  ( 799.9636004259356241, -94.91815448151677970, -311.2241431872006956 ) ) ;
#14764 = CARTESIAN_POINT ( 'NONE',  ( 769.9999999999992042, 178.9475563372491251, 320.0000000000000000 ) ) ;
#14765 = FACE_OUTER_BOUND ( 'NONE', #36865, .T. ) ;
#14766 = EDGE_CURVE ( 'NONE', #12788, #15138, #13047, .T. ) ;
#14767 = CARTESIAN_POINT ( 'NONE',  ( 790.0220218866281812, -271.0999726633344267, 363.2186876482849129 ) ) ;
#14768 = CARTESIAN_POINT ( 'NONE',  ( 795.1360043628807261, -164.0891481129655176, 360.2193346964456282 ) ) ;
#14769 = ORIENTED_EDGE ( 'NONE', *, *, #8604, .T. ) ;
#14770 = CARTESIAN_POINT ( 'NONE',  ( 757.4527132478984868, -40.37269993606240348, -329.1273215169538844 ) ) ;
#14771 = EDGE_CURVE ( 'NONE', #5387, #18328, #8637, .T. ) ;
#14772 = CARTESIAN_POINT ( 'NONE',  ( 787.5162901302840055, -107.3618753856928976, -305.4481719005793252 ) ) ;
#14773 = CARTESIAN_POINT ( 'NONE',  ( 801.3366627262608972, -344.5328690171410813, 353.0897708529566899 ) ) ;
#14774 = CYLINDRICAL_SURFACE ( 'NONE', #35922, 10.00000000000000888 ) ;
#14775 = CARTESIAN_POINT ( 'NONE',  ( 805.6418435158337843, -53.46360902697146855, 363.8556311672236916 ) ) ;
#14776 = CARTESIAN_POINT ( 'NONE',  ( 811.0346526505616112, -230.6346026584197659, -323.0537975583477532 ) ) ;
#14777 = CARTESIAN_POINT ( 'NONE',  ( 812.7932403749906598, -207.1800572038744406, 327.7687537140311633 ) ) ;
#14778 = CARTESIAN_POINT ( 'NONE',  ( 774.6312213355099630, -119.3618753856928691, 364.6798772138717482 ) ) ;
#14779 = CARTESIAN_POINT ( 'NONE',  ( 800.1688906516307043, -322.1692326535048210, -369.0717654672308186 ) ) ;
#14780 = CARTESIAN_POINT ( 'NONE',  ( 805.6418435158337843, -461.4636090269701754, 363.8556311672236916 ) ) ;
#14781 = CARTESIAN_POINT ( 'NONE',  ( 796.9462024416508257, -324.4527844766013231, -308.9653473494370246 ) ) ;
#14782 = LINE ( 'NONE', #42935, #38677 ) ;
#14783 = CARTESIAN_POINT ( 'NONE',  ( 793.2243759319678702, -362.5328690171410813, 318.4439275373583200 ) ) ;
#14784 = CARTESIAN_POINT ( 'NONE',  ( 744.7301800767020268, -52.81642084023856398, 337.4774526936615189 ) ) ;
#14785 = CARTESIAN_POINT ( 'NONE',  ( 768.0187753319979720, -416.6346026584192259, -318.0580252608186242 ) ) ;
#14786 = CARTESIAN_POINT ( 'NONE',  ( 786.6156483768007774, -49.44195992623295410, 315.5913626894246136 ) ) ;
#14787 = CARTESIAN_POINT ( 'NONE',  ( 761.9338519418445230, -86.53286901714194812, -370.4231160770881957 ) ) ;
#14788 = CARTESIAN_POINT ( 'NONE',  ( 781.2497674668890113, -204.3510508353233774, 375.3608509340180603 ) ) ;
#14789 = CARTESIAN_POINT ( 'NONE',  ( 795.1360043628808398, -68.08914811296577341, 360.2193346964456282 ) ) ;
#14790 = ORIENTED_EDGE ( 'NONE', *, *, #39431, .F. ) ;
#14791 = CARTESIAN_POINT ( 'NONE',  ( 765.8855110935204493, -238.1692326535050768, -319.0159684113471599 ) ) ;
#14792 = CARTESIAN_POINT ( 'NONE',  ( 804.6798772138708955, -183.7255117493290015, 334.6312213355107019 ) ) ;
#14793 = CARTESIAN_POINT ( 'NONE',  ( 803.8556311672234642, -33.62377810805116951, -365.6418435158340117 ) ) ;
#14794 = CARTESIAN_POINT ( 'NONE',  ( 794.9819416627830151, -324.9982390220559409, 319.9864689768909898 ) ) ;
#14795 = LINE ( 'NONE', #3929, #7717 ) ;
#14796 = FACE_OUTER_BOUND ( 'NONE', #9210, .T. ) ;
#14797 = ORIENTED_EDGE ( 'NONE', *, *, #12262, .T. ) ;
#14798 = CARTESIAN_POINT ( 'NONE',  ( 754.9735926884551418, -66.35105083532378956, 340.5236548041000333 ) ) ;
#14799 = CARTESIAN_POINT ( 'NONE',  ( 746.4236121716829757, -327.8272453906069472, -328.8385539511384650 ) ) ;
#14800 = CARTESIAN_POINT ( 'NONE',  ( 808.3070685750232087, -282.9982390220559409, 361.1904061080339829 ) ) ;
#14801 = EDGE_CURVE ( 'NONE', #30680, #29342, #21912, .T. ) ;
#14802 = CARTESIAN_POINT ( 'NONE',  ( 814.8230680027162407, 18.19440371013048008, 333.7305795820267917 ) ) ;
#14803 = CARTESIAN_POINT ( 'NONE',  ( 802.5472867521000353, -196.3726999360619061, -350.8726784830461156 ) ) ;
#14804 = CARTESIAN_POINT ( 'NONE',  ( 755.5713283507202505, -173.3618753856927128, -334.6858677611754729 ) ) ;
#14805 = CARTESIAN_POINT ( 'NONE',  ( 797.8594530101009923, -349.5436935675103314, -322.1405469898982119 ) ) ;
#14806 = ORIENTED_EDGE ( 'NONE', *, *, #37084, .F. ) ;
#14807 = CARTESIAN_POINT ( 'NONE',  ( 779.4709603349208464, 23.64894916467591912, -314.7162404726379918 ) ) ;
#14808 = CARTESIAN_POINT ( 'NONE',  ( 792.3570229623688874, -285.1800572038740711, 373.1304606946836202 ) ) ;
#14809 = CARTESIAN_POINT ( 'NONE',  ( 1238.921997096861332, 240.0000000000000568, -244.9999999999999716 ) ) ;
#14810 = CARTESIAN_POINT ( 'NONE',  ( 793.2243759319678702, -362.5328690171410813, 318.4439275373583200 ) ) ;
#14811 = ADVANCED_FACE ( 'NONE', ( #18671 ), #1340, .T. ) ;
#14812 = DIRECTION ( 'NONE',  ( 0.000000000000000000, 0.000000000000000000, 1.000000000000000000 ) ) ;
#14813 = EDGE_CURVE ( 'NONE', #29231, #29607, #34434, .T. ) ;
#14814 = CARTESIAN_POINT ( 'NONE',  ( 793.0897708529556667, -174.5545181178801784, 361.3366627262616362 ) ) ;
#14815 = CARTESIAN_POINT ( 'NONE',  ( 756.3353852180819104, -53.90732993114765037, 331.1735550268788302 ) ) ;
#14816 = ORIENTED_EDGE ( 'NONE', *, *, #22713, .F. ) ;
#14817 = CARTESIAN_POINT ( 'NONE',  ( 802.2119215644370342, -414.0090635724249637, -367.5423716828165084 ) ) ;
#14818 = CARTESIAN_POINT ( 'NONE',  ( 744.7301800767020268, -4.816420840238714085, -337.4774526936615189 ) ) ;
#14819 = CARTESIAN_POINT ( 'NONE',  ( 744.6391490659812007, -278.7363362996980527, 338.7502325331110455 ) ) ;
#14820 = CARTESIAN_POINT ( 'NONE',  ( 796.7845633553578182, -225.6237781080506011, 358.5707757039688204 ) ) ;
#14821 = CARTESIAN_POINT ( 'NONE',  ( 767.8955696845333705, -360.4527844766010958, -362.1676090361162323 ) ) ;
#14822 = DIRECTION ( 'NONE',  ( -0.000000000000000000, 1.000000000000000000, -0.000000000000000000 ) ) ;
#14823 = CARTESIAN_POINT ( 'NONE',  ( 804.6798772138708955, 8.274488250670337663, 334.6312213355107019 ) ) ;
#14824 = DIRECTION ( 'NONE',  ( 4.625929269271485914E-16, -1.000000000000000000, 0.000000000000000000 ) ) ;
#14825 = CARTESIAN_POINT ( 'NONE',  ( 779.4763451958990572, -272.7363362996981095, -365.0264073115438919 ) ) ;
#14826 = CARTESIAN_POINT ( 'NONE',  ( 777.5031285880264704, 1.183579159761269040, 374.9108240113588408 ) ) ;
#14827 = CARTESIAN_POINT ( 'NONE',  ( 745.0891759886404770, -100.2709662947838609, 342.4968714119734159 ) ) ;
#14828 = CARTESIAN_POINT ( 'NONE',  ( 799.9999999999993179, -365.3551492539851893, 18.13243251470705886 ) ) ;
#14829 = CARTESIAN_POINT ( 'NONE',  ( 813.1304606946831655, -449.9073299311464211, -352.3570229623691716 ) ) ;
#14830 = DIRECTION ( 'NONE',  ( 1.000000000000000000, -0.000000000000000000, -0.000000000000000000 ) ) ;
#14831 = EDGE_CURVE ( 'NONE', #22309, #35390, #15221, .T. ) ;
#14832 = CARTESIAN_POINT ( 'NONE',  ( 745.7194118038753459, -397.6454272087885329, 348.7631598425976449 ) ) ;
#14833 = EDGE_CURVE ( 'NONE', #19176, #4054, #43382, .T. ) ;
#14834 = LINE ( 'NONE', #26105, #5100 ) ;
#14835 = CARTESIAN_POINT ( 'NONE',  ( 755.2512626584698410, -343.5436935675103314, 315.2512626584710915 ) ) ;
#14836 = CARTESIAN_POINT ( 'NONE',  ( 755.2512626584698410, -103.5436935675111272, -315.2512626584710915 ) ) ;
#14837 = CARTESIAN_POINT ( 'NONE',  ( 795.1360043628807261, -332.0891481129649492, -360.2193346964456282 ) ) ;
#14838 = PLANE ( 'NONE',  #13659 ) ;
#14839 = CARTESIAN_POINT ( 'NONE',  ( 762.1405469898971887, -433.5436935675099903, 357.8594530101015607 ) ) ;
#14840 = CARTESIAN_POINT ( 'NONE',  ( 793.9708237608222134, -190.9181544815164955, 319.2295555964448681 ) ) ;
#14841 = CARTESIAN_POINT ( 'NONE',  ( 783.7953271457878373, -80.19088175424411702, -375.1787889125761239 ) ) ;
#14842 = CARTESIAN_POINT ( 'NONE',  ( 786.6156483768007774, -73.44195992623286884, -315.5913626894246136 ) ) ;
#14843 = CARTESIAN_POINT ( 'NONE',  ( 788.7631598425961101, -97.44195992623281199, 305.7194118038759143 ) ) ;
#14844 = CARTESIAN_POINT ( 'NONE',  ( 757.8323909638828582, -410.6346026584191691, 352.1044303154654358 ) ) ;
#14845 = CARTESIAN_POINT ( 'NONE',  ( 766.5853460496234675, -157.9874144716871456, 372.3518521366060554 ) ) ;
#14846 = CARTESIAN_POINT ( 'NONE',  ( 791.9812246680005501, -452.6346026584191691, 361.9419747391813189 ) ) ;
#14847 = ORIENTED_EDGE ( 'NONE', *, *, #17991, .T. ) ;
#14848 = CARTESIAN_POINT ( 'NONE',  ( 764.8639956371174549, -104.0891481129656881, -319.7806653035542013 ) ) ;
#14849 = CARTESIAN_POINT ( 'NONE',  ( 765.8855110935204493, -382.1692326535045936, -319.0159684113471599 ) ) ;
#14851 = CARTESIAN_POINT ( 'NONE',  ( 797.6776695296629214, -235.5436935675107293, 357.6776695296636603 ) ) ;
#14850 = CARTESIAN_POINT ( 'NONE',  ( 785.3687786644884454, -275.3618753856923149, 315.3201227861279676 ) ) ;
#14852 = CARTESIAN_POINT ( 'NONE',  ( 701.1634899080286232, 259.9999999999999432, -199.9999999999990337 ) ) ;
#14853 = VERTEX_POINT ( 'NONE', #36439 ) ;
#14854 = CARTESIAN_POINT ( 'NONE',  ( 756.3353852180819104, -437.9073299311463074, 331.1735550268788302 ) ) ;
#14855 = EDGE_CURVE ( 'NONE', #35738, #24791, #35999, .T. ) ;
#14856 = VERTEX_POINT ( 'NONE', #11961 ) ;
#14857 =( NAMED_UNIT ( * ) PLANE_ANGLE_UNIT ( ) SI_UNIT ( $, .RADIAN. ) );
#14858 = CARTESIAN_POINT ( 'NONE',  ( 805.0032342141413437, -181.5436935675108430, 314.9967657858572352 ) ) ;
#14859 = EDGE_CURVE ( 'NONE', #17002, #12726, #25360, .T. ) ;
#14860 = CARTESIAN_POINT ( 'NONE',  ( 793.0897708529556667, -270.5545181178798657, 361.3366627262616362 ) ) ;
#14861 = EDGE_LOOP ( 'NONE', ( #1700, #28992, #22479, #8601 ) ) ;
#14862 = CARTESIAN_POINT ( 'NONE',  ( 773.4516893846965786, -91.64542720878951343, -315.8398074228977066 ) ) ;
#14863 = CARTESIAN_POINT ( 'NONE',  ( 751.2241431872005251, -232.1692326535051620, 359.9636004259367610 ) ) ;
#14864 = CARTESIAN_POINT ( 'NONE',  ( 785.3141322388236176, -237.7255117493289163, -364.4286716492789537 ) ) ;
#14865 = ORIENTED_EDGE ( 'NONE', *, *, #9182, .F. ) ;
#14866 = CARTESIAN_POINT ( 'NONE',  ( 794.9819416627830151, -396.9982390220556567, -319.9864689768909898 ) ) ;
#14867 = CARTESIAN_POINT ( 'NONE',  ( 771.2633955100217236, -47.90732993114767169, -363.4237431249939618 ) ) ;
#14868 = CARTESIAN_POINT ( 'NONE',  ( 755.0488828828309806, -281.8055962898686175, 344.1219089521771934 ) ) ;
#14869 = CARTESIAN_POINT ( 'NONE',  ( 999.9999999999992042, 478.9999999999999432, -199.9999999999999716 ) ) ;
#14870 = DIRECTION ( 'NONE',  ( -0.000000000000000000, -0.000000000000000000, -1.000000000000000000 ) ) ;
#14871 = ADVANCED_FACE ( 'NONE', ( #5036 ), #33215, .T. ) ;
#14872 = CARTESIAN_POINT ( 'NONE',  ( 764.8639956371174549, -8.089148112965974136, -319.7806653035542013 ) ) ;
#14873 = LINE ( 'NONE', #22015, #4223 ) ;
#14874 = ORIENTED_EDGE ( 'NONE', *, *, #44060, .F. ) ;
#14875 = CARTESIAN_POINT ( 'NONE',  ( 810.4231160770870019, -312.5545181178797520, -321.9338519418446936 ) ) ;
#14876 = CARTESIAN_POINT ( 'NONE',  ( 795.8262568251477660, -166.3726999360620198, 308.3538107759623585 ) ) ;
#14878 = CARTESIAN_POINT ( 'NONE',  ( 755.5713283507202505, -269.3618753856924286, -334.6858677611754729 ) ) ;
#14877 = LINE ( 'NONE', #25712, #23876 ) ;
#14879 = CARTESIAN_POINT ( 'NONE',  ( 989.9999999999992042, 249.9999999999998863, 209.9999999999999716 ) ) ;
#14880 = CARTESIAN_POINT ( 'NONE',  ( 790.0220218866281812, -103.0999726633349525, -363.2186876482849129 ) ) ;
#14881 = CARTESIAN_POINT ( 'NONE',  ( 751.9810565676468741, -26.08914811296592262, 360.9747183278973921 ) ) ;
#14882 = DIRECTION ( 'NONE',  ( -0.000000000000000000, -0.000000000000000000, 1.000000000000000000 ) ) ;
#14883 = CARTESIAN_POINT ( 'NONE',  ( 751.6929314249750860, -342.9982390220557704, -318.8095938919659034 ) ) ;
#14884 = LINE ( 'NONE', #43271, #24626 ) ;
#14885 = CARTESIAN_POINT ( 'NONE',  ( 785.3687786644884454, -11.36187538569323863, 315.3201227861279676 ) ) ;
#14886 = CARTESIAN_POINT ( 'NONE',  ( 771.3260364891663130, -283.6454272087889308, 306.0683387631859773 ) ) ;
#14887 = CARTESIAN_POINT ( 'NONE',  ( 744.9990715423526808, -210.3510508353233490, -341.2370466360926002 ) ) ;
#14888 = CARTESIAN_POINT ( 'NONE',  ( 755.2512626584698410, -223.5436935675107577, 315.2512626584710915 ) ) ;
#14889 = CARTESIAN_POINT ( 'NONE',  ( 778.7502325331095108, -432.3510508353226669, -304.6391490659818828 ) ) ;
#14890 = CARTESIAN_POINT ( 'NONE',  ( 799.9999999999993179, -365.3551492539851893, -28.13243251470704109 ) ) ;
#14891 = LINE ( 'NONE', #28969, #1798 ) ;
#14892 = CARTESIAN_POINT ( 'NONE',  ( 774.6858677611749044, -321.7255117493286320, 315.5713283507209894 ) ) ;
#14893 = CARTESIAN_POINT ( 'NONE',  ( 758.4439275373578084, -84.55451811788046257, 353.2243759319684386 ) ) ;
#14894 = CARTESIAN_POINT ( 'NONE',  ( 776.9566956441375396, 11.10349461922141145, -364.8461984189686405 ) ) ;
#14895 = DIRECTION ( 'NONE',  ( 0.000000000000000000, 0.9238795325112891810, -0.3826834323650838421 ) ) ;
#14896 = CARTESIAN_POINT ( 'NONE',  ( -858.8365100919713768, 230.0000000000001990, -199.9999999999881481 ) ) ;
#14898 = CARTESIAN_POINT ( 'NONE',  ( 794.9819416627830151, -372.9982390220557704, 319.9864689768909898 ) ) ;
#14897 = CARTESIAN_POINT ( 'NONE',  ( 773.3843516231979720, -157.4419599262326130, 364.4086373105754433 ) ) ;
#14899 = EDGE_LOOP ( 'NONE', ( #13362, #17972, #1535, #10186 ) ) ;
#14900 = CARTESIAN_POINT ( 'NONE',  ( 805.0264073115434940, -294.3510508353230648, -339.4763451958999099 ) ) ;
#14901 = CARTESIAN_POINT ( 'NONE',  ( 756.1443688327750579, -285.6237781080502600, -314.3581564841659315 ) ) ;
#14902 = FACE_OUTER_BOUND ( 'NONE', #25277, .T. ) ;
#14903 = CARTESIAN_POINT ( 'NONE',  ( 801.1904061080336987, 3.910851887033985896, 368.3070685750235498 ) ) ;
#14904 = VERTEX_POINT ( 'NONE', #663 ) ;
#14905 = CARTESIAN_POINT ( 'NONE',  ( 765.0180583372156207, -312.9982390220559409, 360.0135310231089534 ) ) ;
#14906 = EDGE_CURVE ( 'NONE', #32527, #23783, #8736, .T. ) ;
#14907 = CARTESIAN_POINT ( 'NONE',  ( 783.0433043558608688, -72.89650538077830788, -315.1538015810313027 ) ) ;
#14908 = CARTESIAN_POINT ( 'NONE',  ( 779.9999999999992042, 16.45630643248849267, -339.9999999999999432 ) ) ;
#14909 = CARTESIAN_POINT ( 'NONE',  ( 801.1904061080336987, -164.0891481129655176, -368.3070685750235498 ) ) ;
#14910 = EDGE_LOOP ( 'NONE', ( #41775, #36098, #11312, #42590 ) ) ;
#14911 = CIRCLE ( 'NONE', #8985, 8.024999999999948841 ) ;
#14912 = CARTESIAN_POINT ( 'NONE',  ( 754.8072714833583632, -124.8164208402383366, -338.1981804954721156 ) ) ;
#14913 = EDGE_LOOP ( 'NONE', ( #21303, #33985, #19565, #21370, #43910, #5047, #34769, #31307, #23342, #27099, #4103, #5567, #21607 ) ) ;
#14914 = CARTESIAN_POINT ( 'NONE',  ( 757.0176451133909268, -421.0999726633340288, -349.9200121543848354 ) ) ;
#14915 = CARTESIAN_POINT ( 'NONE',  ( 797.6776695296629214, 4.456306432488530866, 357.6776695296636603 ) ) ;
#14916 = CARTESIAN_POINT ( 'NONE',  ( 756.7813123517142913, -139.9874144716872024, 329.9779781133712504 ) ) ;
#14919 = CARTESIAN_POINT ( 'NONE',  ( 811.6461892240364477, -388.7146871989592114, 324.1737431748509835 ) ) ;
#14918 = DIRECTION ( 'NONE',  ( 1.000000000000000000, 0.000000000000000000, 0.000000000000000000 ) ) ;
#14917 = FACE_OUTER_BOUND ( 'NONE', #20214, .T. ) ;
#14920 = EDGE_LOOP ( 'NONE', ( #43306, #20670, #32029, #19435 ) ) ;
#14921 = CARTESIAN_POINT ( 'NONE',  ( 787.5531968255692163, -381.8272453906068336, -316.1348686366205811 ) ) ;
#14922 = FACE_OUTER_BOUND ( 'NONE', #26806, .T. ) ;
#14923 = CARTESIAN_POINT ( 'NONE',  ( 799.9636004259356241, -214.9181544815164386, -311.2241431872006956 ) ) ;
#14924 = CARTESIAN_POINT ( 'NONE',  ( 814.4686193811664907, -51.28179084515328867, 346.2056067578752732 ) ) ;
#14926 = CARTESIAN_POINT ( 'NONE',  ( -468.8365100919714337, 256.5000000000001705, -199.9999999999908766 ) ) ;
#14925 = PLANE ( 'NONE',  #34448 ) ;
#14927 = CARTESIAN_POINT ( 'NONE',  ( 764.0069404352550464, -327.0783235625956991, -359.2566176426627180 ) ) ;
#14928 = DIRECTION ( 'NONE',  ( -0.000000000000000000, 1.000000000000000000, -0.000000000000000000 ) ) ;
#14929 = CARTESIAN_POINT ( 'NONE',  ( 745.1792804349281596, -182.1908817542437760, -343.7566961878542884 ) ) ;
#14930 = FACE_OUTER_BOUND ( 'NONE', #14389, .T. ) ;
#14931 = FACE_BOUND ( 'NONE', #44148, .T. ) ;
#14932 = CARTESIAN_POINT ( 'NONE',  ( 793.0897708529556667, -390.5545181178794678, 361.3366627262616362 ) ) ;
#14933 = CARTESIAN_POINT ( 'NONE',  ( 754.9967657858570647, -217.5436935675107293, -365.0032342141425943 ) ) ;
#14934 = CYLINDRICAL_SURFACE ( 'NONE', #22378, 7.999999999999896083 ) ;
#14935 = CARTESIAN_POINT ( 'NONE',  ( 764.8639956371174549, -8.089148112965974136, -319.7806653035542013 ) ) ;
#14936 = CARTESIAN_POINT ( 'NONE',  ( 764.1737431748507561, -130.3726999360621619, 371.6461892240376415 ) ) ;
#14937 = CARTESIAN_POINT ( 'NONE',  ( 801.9858362298568863, -99.07832356259642381, -312.7379699480935642 ) ) ;
#14938 = CARTESIAN_POINT ( 'NONE',  ( 759.0252816721024374, -120.9982390220565378, 368.0189434323527280 ) ) ;
#14939 = CARTESIAN_POINT ( 'NONE',  ( 758.8095938919642549, -344.0891481129647786, -311.6929314249763365 ) ) ;
#14940 = LINE ( 'NONE', #8019, #45167 ) ;
#14941 = FACE_OUTER_BOUND ( 'NONE', #10873, .T. ) ;
#14942 = CARTESIAN_POINT ( 'NONE',  ( 802.1676090361156639, -206.6346026584198512, 327.8955696845344505 ) ) ;
#14943 = AXIS2_PLACEMENT_3D ( 'NONE', #18177, #18401, #7543 ) ;
#14944 = CARTESIAN_POINT ( 'NONE',  ( 812.3518521366052028, -457.0999726633339151, 326.5853460496235243 ) ) ;
#14945 = CARTESIAN_POINT ( 'NONE',  ( 749.8865473780648472, -404.5328690171409107, -322.1177392798429082 ) ) ;
#14946 = CARTESIAN_POINT ( 'NONE',  ( 814.5518280994195948, -423.7255117493281205, -332.4837098697145734 ) ) ;
#14947 = DIRECTION ( 'NONE',  ( -0.000000000000000000, 1.000000000000000000, -0.000000000000000000 ) ) ;
#14948 = CARTESIAN_POINT ( 'NONE',  ( 745.1769319972822814, -17.80559628986940979, 346.2694204179732083 ) ) ;
#14949 = ORIENTED_EDGE ( 'NONE', *, *, #13155, .T. ) ;
#14950 = CARTESIAN_POINT ( 'NONE',  ( 756.1348686366196716, -185.2601417444143692, -347.5531968255698416 ) ) ;
#14951 = CARTESIAN_POINT ( 'NONE',  ( 795.1360043628807261, -20.08914811296592973, 360.2193346964456282 ) ) ;
#14952 = CARTESIAN_POINT ( 'NONE',  ( 798.0661480581538854, -194.5328690171415644, -309.5768839229118043 ) ) ;
#14953 = DIRECTION ( 'NONE',  ( 1.000000000000000000, 0.000000000000000000, -0.000000000000000000 ) ) ;
#14954 = CARTESIAN_POINT ( 'NONE',  ( 783.7566961878529810, -336.8965053807774552, 305.1792804349288417 ) ) ;
#14955 = CARTESIAN_POINT ( 'NONE',  ( 801.9419747391806368, -162.4527844766018632, 351.9812246680014027 ) ) ;
#14956 = ORIENTED_EDGE ( 'NONE', *, *, #132, .F. ) ;
#14957 = CARTESIAN_POINT ( 'NONE',  ( 771.2633955100217236, -143.9073299311473590, -363.4237431249939618 ) ) ;
#14958 = CARTESIAN_POINT ( 'NONE',  ( 759.7806653035534055, -342.9982390220557136, 324.8639956371180801 ) ) ;
#14959 = CARTESIAN_POINT ( 'NONE',  ( 763.0537975583475827, -48.45278447660219712, -371.0346526505627480 ) ) ;
#14960 = CIRCLE ( 'NONE', #40758, 10.00000000000000888 ) ;
#14961 = EDGE_CURVE ( 'NONE', #21828, #8827, #19479, .T. ) ;
#14962 = VERTEX_POINT ( 'NONE', #11283 ) ;
#14963 = CARTESIAN_POINT ( 'NONE',  ( 791.0478386215596629, -453.8272453906066630, -306.7653713866226326 ) ) ;
#14964 = ORIENTED_EDGE ( 'NONE', *, *, #24944, .F. ) ;
#14965 = CARTESIAN_POINT ( 'NONE',  ( 766.9102291470427417, -306.5545181178797520, -318.6633372737382501 ) ) ;
#14967 = CARTESIAN_POINT ( 'NONE',  ( 769.9779781133707957, -379.0999726633341993, 316.7813123517150871 ) ) ;
#14966 = CARTESIAN_POINT ( 'NONE',  ( 771.1735550268778070, -57.18005720387489532, 316.3353852180827630 ) ) ;
#14968 = CARTESIAN_POINT ( 'NONE',  ( 804.6798772138708955, -279.7255117493288026, -334.6312213355107019 ) ) ;
#14970 = CARTESIAN_POINT ( 'NONE',  ( 814.8230680027162407, -293.8055962898685607, 333.7305795820267917 ) ) ;
#14969 = CARTESIAN_POINT ( 'NONE',  ( 808.0189434323515343, -398.0891481129647218, 319.0252816721025511 ) ) ;
#14971 = CARTESIAN_POINT ( 'NONE',  ( 783.7566961878529810, -72.89650538077830788, 305.1792804349288417 ) ) ;
#14972 = CARTESIAN_POINT ( 'NONE',  ( 793.0897708529556667, -294.5545181178797520, -361.3366627262616362 ) ) ;
#14973 = CARTESIAN_POINT ( 'NONE',  ( 788.7366044899766848, -275.9073299311469896, -316.5762568750059813 ) ) ;
#14974 = DIRECTION ( 'NONE',  ( 0.000000000000000000, 0.000000000000000000, -1.000000000000000000 ) ) ;
#14975 = CARTESIAN_POINT ( 'NONE',  ( 762.1405469898971887, -121.5436935675110419, -357.8594530101015607 ) ) ;
#14976 = DIRECTION ( 'NONE',  ( 1.000000000000000000, 0.000000000000000000, 0.000000000000000000 ) ) ;
#14977 = VERTEX_POINT ( 'NONE', #41279 ) ;
#14978 = CARTESIAN_POINT ( 'NONE',  ( 767.6429770376289525, -441.1800572038735027, 306.8695393053162093 ) ) ;
#14980 = CARTESIAN_POINT ( 'NONE',  ( 927.9999999999993179, 219.9999999999998863, 359.9749999999999659 ) ) ;
#14979 = CARTESIAN_POINT ( 'NONE',  ( 777.0937506421101943, 18.86692508245304367, 309.9999999999999432 ) ) ;
#14981 = CARTESIAN_POINT ( 'NONE',  ( 768.9521613784389729, -81.82724539060772884, -373.2346286133773106 ) ) ;
#14982 = LINE ( 'NONE', #18233, #27086 ) ;
#14983 = FACE_OUTER_BOUND ( 'NONE', #39848, .T. ) ;
#14984 = CARTESIAN_POINT ( 'NONE',  ( 805.2837595273609850, -266.7363362996981095, 340.5290396650784714 ) ) ;
#14985 = CARTESIAN_POINT ( 'NONE',  ( 805.1927285166397041, -160.8164208402382371, 341.8018195045277707 ) ) ;
#14986 = ORIENTED_EDGE ( 'NONE', *, *, #26602, .T. ) ;
#14987 = CARTESIAN_POINT ( 'NONE',  ( 748.9653473494365699, -98.63460265842023489, -356.9462024416520762 ) ) ;
#14988 = CARTESIAN_POINT ( 'NONE',  ( 764.0069404352550464, -327.0783235625956991, 359.2566176426627180 ) ) ;
#14989 = LINE ( 'NONE', #24446, #41100 ) ;
#14990 = CARTESIAN_POINT ( 'NONE',  ( 781.2370466360911223, -44.73633629969875614, 304.9990715423533629 ) ) ;
#14991 = CARTESIAN_POINT ( 'NONE',  ( 808.0189434323515343, -230.0891481129652618, -319.0252816721025511 ) ) ;
#14992 = CARTESIAN_POINT ( 'NONE',  ( 778.1981804954714335, -106.2709662947838467, 314.8072714833589885 ) ) ;
#14993 = CIRCLE ( 'NONE', #21610, 2.749999999999842792 ) ;
#14994 = LINE ( 'NONE', #3691, #23238 ) ;
#14995 = CARTESIAN_POINT ( 'NONE',  ( 786.2056067578752163, -323.8055962898684470, -374.4686193811670023 ) ) ;
#14996 = CARTESIAN_POINT ( 'NONE',  ( 747.6481478633932056, -445.0999726633338582, 353.4146539503763620 ) ) ;
#14997 = CARTESIAN_POINT ( 'NONE',  ( 814.2001403089898304, -305.3618753856922581, -347.4397851343538264 ) ) ;
#14998 = CARTESIAN_POINT ( 'NONE',  ( 799.9999999999993179, -462.9681489794448339, 370.0000000000000568 ) ) ;
#14999 = CARTESIAN_POINT ( 'NONE',  ( 772.3691319403857278, -383.2601417444137155, 315.8894580844506663 ) ) ;
#15000 = ORIENTED_EDGE ( 'NONE', *, *, #39742, .F. ) ;
#15001 = CARTESIAN_POINT ( 'NONE',  ( 774.6858677611749044, -417.7255117493283478, -315.5713283507209894 ) ) ;
#15003 = EDGE_CURVE ( 'NONE', #27925, #40626, #26948, .T. ) ;
#15002 = CARTESIAN_POINT ( 'NONE',  ( 747.3154664389472828, -91.98741447168737295, -326.4474001241230781 ) ) ;
#15004 = LINE ( 'NONE', #8531, #10786 ) ;
#15005 = CARTESIAN_POINT ( 'NONE',  ( 744.8212110874229666, -210.8965053807778816, 336.2046728542121627 ) ) ;
#15006 = CARTESIAN_POINT ( 'NONE',  ( 755.5713283507202505, -53.36187538569310362, 334.6858677611754729 ) ) ;
#15007 = AXIS2_PLACEMENT_3D ( 'NONE', #38993, #13579, #27658 ) ;
#15008 = ORIENTED_EDGE ( 'NONE', *, *, #26387, .F. ) ;
#15009 = CARTESIAN_POINT ( 'NONE',  ( 773.3843516231979720, -229.4419599262323572, -364.4086373105754433 ) ) ;
#15010 = CARTESIAN_POINT ( 'NONE',  ( 765.0180583372156207, -216.9982390220562252, 360.0135310231089534 ) ) ;
#15011 = CARTESIAN_POINT ( 'NONE',  ( 771.2368401574024119, -61.44195992623291147, -374.2805881961240857 ) ) ;
#15012 = CARTESIAN_POINT ( 'NONE',  ( 802.1676090361155502, -350.6346026584193396, 327.8955696845344505 ) ) ;
#15013 = CARTESIAN_POINT ( 'NONE',  ( 794.5458710602071051, -452.9681489794447771, -360.4198067286714604 ) ) ;
#15014 = VERTEX_POINT ( 'NONE', #27188 ) ;
#15015 = CARTESIAN_POINT ( 'NONE',  ( 757.7880784355613741, -330.0090635724251342, -312.4576283171834916 ) ) ;
#15016 = CARTESIAN_POINT ( 'NONE',  ( 805.0032342141413437, -277.5436935675105588, 314.9967657858572352 ) ) ;
#15017 = CARTESIAN_POINT ( 'NONE',  ( 766.5853460496234675, 10.01258552831232329, 372.3518521366060554 ) ) ;
#15018 = CARTESIAN_POINT ( 'NONE',  ( 804.1105419155481968, -195.8272453906074304, -347.6308680596136469 ) ) ;
#15019 = CARTESIAN_POINT ( 'NONE',  ( 803.4237431249931660, -183.1800572038744974, -331.2633955100225194 ) ) ;
#15020 = AXIS2_PLACEMENT_3D ( 'NONE', #27913, #24430, #21438 ) ;
#15021 = CARTESIAN_POINT ( 'NONE',  ( 765.0180583372156207, -384.9982390220556567, -360.0135310231089534 ) ) ;
#15022 = ORIENTED_EDGE ( 'NONE', *, *, #3156, .T. ) ;
#15023 = CIRCLE ( 'NONE', #38625, 6.118999999999985562 ) ;
#15024 = CARTESIAN_POINT ( 'NONE',  ( 800.2193346964447755, -450.9982390220554294, -355.1360043628815788 ) ) ;
#15025 = EDGE_LOOP ( 'NONE', ( #19843, #22820, #43011, #42240 ) ) ;
#15026 = CARTESIAN_POINT ( 'NONE',  ( 749.2812353651451076, -294.4527844766013800, 323.2262854647983090 ) ) ;
#15027 = DIRECTION ( 'NONE',  ( -0.000000000000000000, 1.000000000000000000, -0.000000000000000000 ) ) ;
#15028 = CARTESIAN_POINT ( 'NONE',  ( 759.0159684113467620, -208.9181544815164102, 325.8855110935213020 ) ) ;
#15029 = DIRECTION ( 'NONE',  ( 0.000000000000000000, 0.000000000000000000, 1.000000000000000000 ) ) ;
#15030 = CARTESIAN_POINT ( 'NONE',  ( 799.2566176426618085, -144.0090635724257027, 324.0069404352559559 ) ) ;
#15031 = CARTESIAN_POINT ( 'NONE',  ( 781.8018195045266339, -46.27096629478404566, 365.1927285166406705 ) ) ;
#15032 = EDGE_LOOP ( 'NONE', ( #16313, #2561, #5751, #31806, #29396, #41934, #38897, #19945 ) ) ;
#15033 = CARTESIAN_POINT ( 'NONE',  ( 745.7194118038753459, -397.6454272087885329, -348.7631598425976449 ) ) ;
#15034 = CARTESIAN_POINT ( 'NONE',  ( 792.2312462859673587, -11.90732993114778182, -307.2067596250082602 ) ) ;
#15035 = CARTESIAN_POINT ( 'NONE',  ( 745.5313806188320314, -279.2817908451526137, 333.7943932421247268 ) ) ;
#15036 = CARTESIAN_POINT ( 'NONE',  ( 754.9735926884551418, -210.3510508353233490, 340.5236548041000333 ) ) ;
#15037 = CARTESIAN_POINT ( 'NONE',  ( 804.9363028652555840, -352.2709662947830225, -338.2165204200192079 ) ) ;
#15038 = PLANE ( 'NONE',  #17220 ) ;
#15039 = CIRCLE ( 'NONE', #37171, 2.749999999999835687 ) ;
#15040 = CARTESIAN_POINT ( 'NONE',  ( 800.9840315886518738, -460.9181544815156713, 354.1144889064786412 ) ) ;
#15041 =( NAMED_UNIT ( * ) PLANE_ANGLE_UNIT ( ) SI_UNIT ( $, .RADIAN. ) );
#15042 = CARTESIAN_POINT ( 'NONE',  ( 757.0176451133909268, -253.0999726633345119, -349.9200121543848354 ) ) ;
#15043 = CARTESIAN_POINT ( 'NONE',  ( 810.7187646348534145, -42.45278447660223264, 356.7737145352016341 ) ) ;
#15044 = CARTESIAN_POINT ( 'NONE',  ( 748.9653473494363425, -98.63460265842024910, 356.9462024416521331 ) ) ;
#15045 = FACE_OUTER_BOUND ( 'NONE', #17514, .T. ) ;
#15046 = FILL_AREA_STYLE ('',( #25668 ) ) ;
#15047 = CARTESIAN_POINT ( 'NONE',  ( 746.4236121716829757, -375.8272453906069472, 328.8385539511384650 ) ) ;
#15048 = CARTESIAN_POINT ( 'NONE',  ( 454.7528517110262101, 199.9999999999999432, -122.7905160835442615 ) ) ;
#15049 = CARTESIAN_POINT ( 'NONE',  ( 800.9747183278959710, -372.9982390220557704, 311.9810565676471583 ) ) ;
#15050 = CARTESIAN_POINT ( 'NONE',  ( 771.2633955100217236, -311.9073299311468759, -363.4237431249939618 ) ) ;
#15051 = EDGE_CURVE ( 'NONE', #25954, #463, #5248, .T. ) ;
#15052 = PLANE ( 'NONE',  #18088 ) ;
#15053 = CARTESIAN_POINT ( 'NONE',  ( 800.2193346964447755, -426.9982390220554862, 355.1360043628815788 ) ) ;
#15054 = CIRCLE ( 'NONE', #8391, 20.00000000000001776 ) ;
#15055 = AXIS2_PLACEMENT_3D ( 'NONE', #43491, #29419, #11181 ) ;
#15056 = CARTESIAN_POINT ( 'NONE',  ( 760.7433823573367135, -180.0090635724255890, 355.9930595647440441 ) ) ;
#15057 = CARTESIAN_POINT ( 'NONE',  ( 811.3240766477731540, -52.37269993606237506, -355.6651683502462902 ) ) ;
#15058 = CARTESIAN_POINT ( 'NONE',  ( 761.2382568024794409, -135.6237781080508853, -356.9571628226838129 ) ) ;
#15059 = CARTESIAN_POINT ( 'NONE',  ( 761.9338519418445230, -86.53286901714194812, 370.4231160770881957 ) ) ;
#15060 = CARTESIAN_POINT ( 'NONE',  ( 774.6312213355098493, -431.3618753856918602, 364.6798772138717482 ) ) ;
#15061 = CARTESIAN_POINT ( 'NONE',  ( 771.1735550268778070, -9.180057203875058747, -316.3353852180827630 ) ) ;
#15063 = EDGE_LOOP ( 'NONE', ( #29111, #14739, #12678, #37397 ) ) ;
#15062 = CARTESIAN_POINT ( 'NONE',  ( 800.7704444035546203, -148.1692326535053610, -326.0291762391768771 ) ) ;
#15064 = CARTESIAN_POINT ( 'NONE',  ( 795.1360043628807261, -92.08914811296568814, -360.2193346964456282 ) ) ;
#15065 = EDGE_CURVE ( 'NONE', #14459, #33292, #28543, .T. ) ;
#15066 = CARTESIAN_POINT ( 'NONE',  ( 793.2243759319678702, -386.5328690171409676, -318.4439275373583200 ) ) ;
#15068 = CARTESIAN_POINT ( 'NONE',  ( 767.8955696845334842, -264.4527844766016074, 362.1676090361161755 ) ) ;
#15067 = CARTESIAN_POINT ( 'NONE',  ( 797.8594530101008786, -253.5436935675104735, 322.1405469898980982 ) ) ;
#15069 = DIRECTION ( 'NONE',  ( -0.000000000000000000, -0.000000000000000000, 1.000000000000000000 ) ) ;
#15070 = EDGE_LOOP ( 'NONE', ( #21494, #28118, #10303, #40058 ) ) ;
#15071 = CARTESIAN_POINT ( 'NONE',  ( 768.0187753319979720, -440.6346026584191122, 318.0580252608186242 ) ) ;
#15072 = VECTOR ( 'NONE', #30913, 1000.000000000000000 ) ;
#15073 = ORIENTED_EDGE ( 'NONE', *, *, #35323, .T. ) ;
#15074 = CARTESIAN_POINT ( 'NONE',  ( 751.9810565676468741, -194.0891481129654039, 360.9747183278973921 ) ) ;
#15075 = CARTESIAN_POINT ( 'NONE',  ( 755.8894580844503253, -255.8272453906072315, 332.3691319403863531 ) ) ;
#15076 = ORIENTED_EDGE ( 'NONE', *, *, #38818, .T. ) ;
#15077 = CARTESIAN_POINT ( 'NONE',  ( 763.8424801807145741, -66.00906357242595845, -320.5453621957614700 ) ) ;
#15078 = CARTESIAN_POINT ( 'NONE',  ( 791.1614460488616487, -227.2601417444141987, 373.5763878283158874 ) ) ;
#15079 = CARTESIAN_POINT ( 'NONE',  ( 781.8018195045267476, -262.2709662947832499, -365.1927285166407273 ) ) ;
#15080 = ORIENTED_EDGE ( 'NONE', *, *, #13885, .T. ) ;
#15081 = ADVANCED_FACE ( 'NONE', ( #20245 ), #26497, .F. ) ;
#15082 = CARTESIAN_POINT ( 'NONE',  ( 800.0135310231082713, -398.0891481129647218, -325.0180583372163028 ) ) ;
#15083 = CARTESIAN_POINT ( 'NONE',  ( 771.1735550268778070, -57.18005720387489532, -316.3353852180827630 ) ) ;
#15084 = EDGE_CURVE ( 'NONE', #35455, #15202, #5710, .T. ) ;
#15085 = CARTESIAN_POINT ( 'NONE',  ( 798.7617431975189675, -267.6237781080504305, 323.0428371773161871 ) ) ;
#15086 = CARTESIAN_POINT ( 'NONE',  ( -78.83651009197140525, 256.5000000000000568, -197.2499999999937188 ) ) ;
#15087 = DIRECTION ( 'NONE',  ( 1.000000000000000000, 0.000000000000000000, 0.000000000000000000 ) ) ;
#15088 = AXIS2_PLACEMENT_3D ( 'NONE', #39128, #3085, #20854 ) ;
#15089 = CARTESIAN_POINT ( 'NONE',  ( 788.8264449731200330, -21.18005720387502677, -363.6646147819171233 ) ) ;
#15090 = CARTESIAN_POINT ( 'NONE',  ( 879.9999999999990905, 479.9999999999998863, -199.9999999999999716 ) ) ;
#15091 = ORIENTED_EDGE ( 'NONE', *, *, #37961, .T. ) ;
#15092 = CARTESIAN_POINT ( 'NONE',  ( 807.2620300519052989, -312.0090635724251911, -318.0141637701419768 ) ) ;
#15093 = CIRCLE ( 'NONE', #3275, 9.999999999999980460 ) ;
#15094 = CARTESIAN_POINT ( 'NONE',  ( 815.3608509340175488, -170.7363362996983938, 341.2497674668889545 ) ) ;
#15096 = CARTESIAN_POINT ( 'NONE',  ( 771.1735550268778070, -273.1800572038742985, -316.3353852180827630 ) ) ;
#15095 = CARTESIAN_POINT ( 'NONE',  ( 879.9999999999992042, 99.99999999999984368, 350.0000000000000000 ) ) ;
#15097 = DIRECTION ( 'NONE',  ( -1.000000000000000000, -4.625929269271485914E-16, 0.000000000000000000 ) ) ;
#15098 = CARTESIAN_POINT ( 'NONE',  ( 757.4527132478984868, -136.3726999360621051, -329.1273215169538844 ) ) ;
#15099 = CYLINDRICAL_SURFACE ( 'NONE', #7743, 20.00000000000004974 ) ;
#15100 = CARTESIAN_POINT ( 'NONE',  ( 764.3348316497523456, -22.71468719896029853, -308.6759233522265617 ) ) ;
#15101 = CARTESIAN_POINT ( 'NONE',  ( 747.2067596250078623, -363.1800572038739006, -352.2312462859687230 ) ) ;
#15102 = CARTESIAN_POINT ( 'NONE',  ( 571.1634899080285095, 259.9999999999999432, -199.9999999999981526 ) ) ;
#15103 = CARTESIAN_POINT ( 'NONE',  ( 759.9864689768902508, -26.08914811296592262, 354.9819416627836404 ) ) ;
#15104 = AXIS2_PLACEMENT_3D ( 'NONE', #38508, #44994, #38294 ) ;
#15105 = EDGE_CURVE ( 'NONE', #27542, #4510, #21924, .T. ) ;
#15106 = CARTESIAN_POINT ( 'NONE',  ( 797.8822607201568644, -294.5545181178797520, 370.1134526219340160 ) ) ;
#15107 = CARTESIAN_POINT ( 'NONE',  ( 813.2346286133761168, -221.2601417444142271, -328.9521613784389160 ) ) ;
#15108 = CARTESIAN_POINT ( 'NONE',  ( 772.5602148656447525, -225.7255117493289163, 305.7998596910095443 ) ) ;
#15109 = CARTESIAN_POINT ( 'NONE',  ( 763.0537975583475827, -0.4527844766023628176, -371.0346526505627480 ) ) ;
#15110 = DIRECTION ( 'NONE',  ( 0.000000000000000000, 0.000000000000000000, 1.000000000000000000 ) ) ;
#15111 = CIRCLE ( 'NONE', #32038, 2.749999999999863665 ) ;
#15112 = EDGE_CURVE ( 'NONE', #15121, #22938, #13329, .T. ) ;
#15113 = VERTEX_POINT ( 'NONE', #12636 ) ;
#15114 = CARTESIAN_POINT ( 'NONE',  ( 778.2165204200184689, -334.8164208402376403, 364.9363028652563230 ) ) ;
#15115 = CARTESIAN_POINT ( 'NONE',  ( 798.5707757039680246, -101.4636090269713264, 356.7845633553585003 ) ) ;
#15116 = CARTESIAN_POINT ( 'NONE',  ( 803.8651313633788504, -5.260141744414903897, -332.4468031744301015 ) ) ;
#15117 = FACE_OUTER_BOUND ( 'NONE', #24312, .T. ) ;
#15118 = CARTESIAN_POINT ( 'NONE',  ( 919.9999999999993179, 154.9999999999998863, -360.0000000000000000 ) ) ;
#15120 = CARTESIAN_POINT ( 'NONE',  ( 804.6798772138708955, -351.7255117493284047, 334.6312213355107019 ) ) ;
#15119 = CARTESIAN_POINT ( 'NONE',  ( 796.7845633553578182, -153.6237781080508000, 358.5707757039688204 ) ) ;
#15121 = VERTEX_POINT ( 'NONE', #34336 ) ;
#15122 = ADVANCED_FACE ( 'NONE', ( #20020 ), #23696, .F. ) ;
#15123 = CARTESIAN_POINT ( 'NONE',  ( 763.2154366446407039, -309.6237781080502600, -321.4292242960311228 ) ) ;
#15124 = CARTESIAN_POINT ( 'NONE',  ( 785.3687786644884454, -155.3618753856927128, 315.3201227861279676 ) ) ;
#15125=STYLED_ITEM('',(#45758),#3320);
#15126 = CARTESIAN_POINT ( 'NONE',  ( 810.1134526219336749, -320.5328690171411949, -357.8822607201570349 ) ) ;
#15127 = CARTESIAN_POINT ( 'NONE',  ( -919.9999999999993179, 219.9999999999998863, 339.9999999999999432 ) ) ;
#15128 = CARTESIAN_POINT ( 'NONE',  ( 807.5423716828161105, -441.0783235625953580, 362.2119215644372048 ) ) ;
#15129 = ORIENTED_EDGE ( 'NONE', *, *, #10566, .T. ) ;
#15130 = CARTESIAN_POINT ( 'NONE',  ( 785.3141322388236176, -309.7255117493287457, 364.4286716492789537 ) ) ;
#15131 = VECTOR ( 'NONE', #27702, 1000.000000000000000 ) ;
#15132 = CARTESIAN_POINT ( 'NONE',  ( 790.8726784830453198, -82.71468719896012090, -362.5472867521010585 ) ) ;
#15133 = ORIENTED_EDGE ( 'NONE', *, *, #17129, .T. ) ;
#15134 = CARTESIAN_POINT ( 'NONE',  ( 795.1360043628807261, -428.0891481129644944, 360.2193346964456282 ) ) ;
#15135 = CARTESIAN_POINT ( 'NONE',  ( 804.7487373415286811, -187.5436935675108430, -364.7487373415288516 ) ) ;
#15136 = ORIENTED_EDGE ( 'NONE', *, *, #42455, .F. ) ;
#15137 = CARTESIAN_POINT ( 'NONE',  ( 771.1735550268780344, -129.1800572038746679, -316.3353852180828198 ) ) ;
#15138 = VERTEX_POINT ( 'NONE', #30879 ) ;
#15139 = CARTESIAN_POINT ( 'NONE',  ( 763.0428371773158460, -419.4636090269702891, -358.7617431975195359 ) ) ;
#15140 = VECTOR ( 'NONE', #29539, 1000.000000000000000 ) ;
#15141 = EDGE_CURVE ( 'NONE', #23098, #22342, #27815, .T. ) ;
#15142 = CARTESIAN_POINT ( 'NONE',  ( 778.2165204200184689, 1.183579159761269040, 364.9363028652563230 ) ) ;
#15143 = CARTESIAN_POINT ( 'NONE',  ( 748.9653473494363425, -218.6346026584197944, 356.9462024416521331 ) ) ;
#15144 = CARTESIAN_POINT ( 'NONE',  ( 801.3366627262608972, -152.5328690171416781, 353.0897708529566899 ) ) ;
#15146 = CARTESIAN_POINT ( 'NONE',  ( -775.4999999999993179, -513.1383975375929367, -349.9999999999999432 ) ) ;
#15145 = DIRECTION ( 'NONE',  ( 1.000000000000000000, 0.000000000000000000, 0.000000000000000000 ) ) ;
#15147 = AXIS2_PLACEMENT_3D ( 'NONE', #44707, #29697, #12384 ) ;
#15148 = CIRCLE ( 'NONE', #40943, 10.00000000000000888 ) ;
#15149 = ORIENTED_EDGE ( 'NONE', *, *, #40478, .F. ) ;
#15150 = CARTESIAN_POINT ( 'NONE',  ( 761.4292242960306112, -401.4636090269704027, -323.2154366446414429 ) ) ;
#15151 = DIRECTION ( 'NONE',  ( 0.000000000000000000, 0.000000000000000000, 1.000000000000000000 ) ) ;
#15152 = CARTESIAN_POINT ( 'NONE',  ( 809.0717654672305343, -196.9181544815164386, -360.1688906516309885 ) ) ;
#15153 = CARTESIAN_POINT ( 'NONE',  ( 804.1009440267234822, -71.46360902697141171, 314.0944755984392600 ) ) ;
#15155 = LINE ( 'NONE', #21395, #26230 ) ;
#15154 = CARTESIAN_POINT ( 'NONE',  ( 919.9999999999993179, 154.9999999999998863, 350.0000000000000000 ) ) ;
#15156 = CARTESIAN_POINT ( 'NONE',  ( 772.3691319403857278, -311.2601417444139429, -315.8894580844506663 ) ) ;
#15157 = CARTESIAN_POINT ( 'NONE',  ( 769.9999999999992042, 205.0000000000000568, -339.9999999999999432 ) ) ;
#15158 = CARTESIAN_POINT ( 'NONE',  ( 783.7953271457878373, -200.1908817542436907, -375.1787889125761239 ) ) ;
#15159 = CARTESIAN_POINT ( 'NONE',  ( 919.9999999999993179, 154.9999999999998863, 359.9749999999999659 ) ) ;
#15160 = FACE_OUTER_BOUND ( 'NONE', #11259, .T. ) ;
#15161 = CARTESIAN_POINT ( 'NONE',  ( 802.5472867521000353, -412.3726999360612808, 350.8726784830461156 ) ) ;
#15162 = AXIS2_PLACEMENT_3D ( 'NONE', #27088, #44400, #12754 ) ;
#15163 = AXIS2_PLACEMENT_3D ( 'NONE', #24899, #4573, #18665 ) ;
#15164 = CARTESIAN_POINT ( 'NONE',  ( 777.4774526936600978, -226.2709662947834488, -304.7301800767028226 ) ) ;
#15165 = FACE_OUTER_BOUND ( 'NONE', #7450, .T. ) ;
#15166 = CARTESIAN_POINT ( 'NONE',  ( 767.8955696845333705, -0.4527844766023628176, -362.1676090361162323 ) ) ;
#15167 = AXIS2_PLACEMENT_3D ( 'NONE', #18609, #7531, #25757 ) ;
#15168 = EDGE_CURVE ( 'NONE', #3612, #17065, #23014, .T. ) ;
#15169 = CARTESIAN_POINT ( 'NONE',  ( 788.6739635108323228, -175.6454272087892718, 373.9316612368139090 ) ) ;
#15170 = CARTESIAN_POINT ( 'NONE',  ( 786.2056067578752163, -131.8055962898690439, -374.4686193811670023 ) ) ;
#15171 = CARTESIAN_POINT ( 'NONE',  ( 805.0032342141412300, -133.5436935675110135, 314.9967657858571783 ) ) ;
#15172 = CARTESIAN_POINT ( 'NONE',  ( 782.5225473063381969, -358.2709662947829088, -375.2698199232970637 ) ) ;
#15173 = FACE_OUTER_BOUND ( 'NONE', #36081, .T. ) ;
#15175 = EDGE_CURVE ( 'NONE', #30803, #15113, #16105, .T. ) ;
#15174 = FACE_OUTER_BOUND ( 'NONE', #26172, .T. ) ;
#15176 = CARTESIAN_POINT ( 'NONE',  ( 804.6798772138708955, -231.7255117493288310, 334.6312213355107019 ) ) ;
#15177 = CARTESIAN_POINT ( 'NONE',  ( 798.5707757039680246, -29.46360902697153250, 356.7845633553585003 ) ) ;
#15178 = CARTESIAN_POINT ( 'NONE',  ( 801.9858362298568863, -411.0783235625954717, -312.7379699480935642 ) ) ;
#15179 = CIRCLE ( 'NONE', #40972, 30.00000000000008171 ) ;
#15180 = CARTESIAN_POINT ( 'NONE',  ( 814.2805881961230625, -1.645427208789804308, -331.2368401574024119 ) ) ;
#15181 = DIRECTION ( 'NONE',  ( 0.000000000000000000, 0.000000000000000000, 1.000000000000000000 ) ) ;
#15182 = CARTESIAN_POINT ( 'NONE',  ( 815.1787889125755555, -30.89650538077846065, 343.7953271457877804 ) ) ;
#15183 = VERTEX_POINT ( 'NONE', #30411 ) ;
#15184 = AXIS2_PLACEMENT_3D ( 'NONE', #20150, #9540, #37710 ) ;
#15185 = APPLICATION_CONTEXT ( 'automotive_design' ) ;
#15186 = PRODUCT_RELATED_PRODUCT_CATEGORY ( 'part', '', ( #38824 ) ) ;
#15187 = CARTESIAN_POINT ( 'NONE',  ( 803.2186876482843445, -199.9874144716870603, -350.0220218866286928 ) ) ;
#15188 = CARTESIAN_POINT ( 'NONE',  ( 755.3201227861273992, -27.72551174932954510, 345.3687786644892981 ) ) ;
#15189 = CARTESIAN_POINT ( 'NONE',  ( 768.8385539511368734, -239.2601417444141987, -306.4236121716840557 ) ) ;
#15190 =( LENGTH_UNIT ( ) NAMED_UNIT ( * ) SI_UNIT ( .MILLI., .METRE. ) );
#15191 = CARTESIAN_POINT ( 'NONE',  ( 751.2241431872005251, -352.1692326535046504, 359.9636004259367610 ) ) ;
#15192 = CARTESIAN_POINT ( 'NONE',  ( 778.2165204200184689, -166.8164208402382087, 364.9363028652563230 ) ) ;
#15193 = CARTESIAN_POINT ( 'NONE',  ( 778.1981804954714335, -82.27096629478388934, -314.8072714833589885 ) ) ;
#15194 = VERTEX_POINT ( 'NONE', #23246 ) ;
#15195 = CARTESIAN_POINT ( 'NONE',  ( 791.1614460488616487, -419.2601417444136587, 373.5763878283158874 ) ) ;
#15196 = CARTESIAN_POINT ( 'NONE',  ( 800.2193346964447755, -138.9982390220563957, -355.1360043628815788 ) ) ;
#15197 = CARTESIAN_POINT ( 'NONE',  ( 804.6798772138708955, -351.7255117493284047, 334.6312213355107019 ) ) ;
#15198 = CARTESIAN_POINT ( 'NONE',  ( 763.2262854647970016, -32.63460265842044095, -309.2812353651462445 ) ) ;
#15199 = EDGE_LOOP ( 'NONE', ( #1423, #4825, #2515, #37608 ) ) ;
#15200 = CARTESIAN_POINT ( 'NONE',  ( 811.3240766477731540, -436.3726999360612240, -355.6651683502462902 ) ) ;
#15201 = AXIS2_PLACEMENT_3D ( 'NONE', #40976, #1276, #29454 ) ;
#15202 = VERTEX_POINT ( 'NONE', #34096 ) ;
#15203 = CARTESIAN_POINT ( 'NONE',  ( 804.6971507214547046, -315.2817908451525000, -344.0799538623459739 ) ) ;
#15205 = CARTESIAN_POINT ( 'NONE',  ( 786.5483106153019435, -367.6454272087886466, 364.1601925771022366 ) ) ;
#15204 = CARTESIAN_POINT ( 'NONE',  ( 778.2165204200184689, -70.81642084023850714, 364.9363028652563230 ) ) ;
#15206 = CARTESIAN_POINT ( 'NONE',  ( 800.2193346964447755, -282.9982390220558841, -355.1360043628815788 ) ) ;
#15207 = AXIS2_PLACEMENT_3D ( 'NONE', #4524, #21844, #4744 ) ;
#15209 = CARTESIAN_POINT ( 'NONE',  ( 800.1688906516307043, -274.1692326535049915, 369.0717654672308186 ) ) ;
#15208 = CARTESIAN_POINT ( 'NONE',  ( 748.9653473494365699, -386.6346026584192828, 356.9462024416520762 ) ) ;
#15210 = CARTESIAN_POINT ( 'NONE',  ( 815.0009284576459549, -102.3510508353236901, 338.7629533639073429 ) ) ;
#15211 = CARTESIAN_POINT ( 'NONE',  ( 798.5707757039680246, -293.4636090269707438, -356.7845633553585003 ) ) ;
#15212 = CARTESIAN_POINT ( 'NONE',  ( 755.0636971347428243, -292.2709662947831930, -341.7834795799807353 ) ) ;
#15213 = CARTESIAN_POINT ( 'NONE',  ( 701.1634899080286232, 259.9999999999999432, -199.9999999999990337 ) ) ;
#15214 = CARTESIAN_POINT ( 'NONE',  ( 762.1405469898971887, -169.5436935675108430, -357.8594530101015607 ) ) ;
#15215 = CARTESIAN_POINT ( 'NONE',  ( -786.4999999999993179, -496.5085659523897448, -356.8883017825714319 ) ) ;
#15216 = CARTESIAN_POINT ( 'NONE',  ( 745.4481719005789273, -411.7255117493282910, 347.5162901302853129 ) ) ;
#15217 = AXIS2_PLACEMENT_3D ( 'NONE', #23605, #6296, #2838 ) ;
#15219 = DIRECTION ( 'NONE',  ( 0.000000000000000000, 0.000000000000000000, 1.000000000000000000 ) ) ;
#15218 = LINE ( 'NONE', #28610, #10819 ) ;
#15220 = CARTESIAN_POINT ( 'NONE',  ( 752.7379699480933368, -84.00906357242590161, -361.9858362298580232 ) ) ;
#15221 = LINE ( 'NONE', #1552, #32237 ) ;
#15222 = DIRECTION ( 'NONE',  ( 1.000000000000000000, 0.000000000000000000, 0.000000000000000000 ) ) ;
#15223 = AXIS2_PLACEMENT_3D ( 'NONE', #32930, #12354, #43742 ) ;
#15224 = CARTESIAN_POINT ( 'NONE',  ( 757.0176451133909268, -301.0999726633342561, 349.9200121543848354 ) ) ;
#15225 = CARTESIAN_POINT ( 'NONE',  ( 781.7834795799800531, -154.8164208402382371, 315.0636971347436202 ) ) ;
#15226 = ORIENTED_EDGE ( 'NONE', *, *, #41564, .T. ) ;
#15227 = CARTESIAN_POINT ( 'NONE',  ( 792.3570229623691148, -141.1800572038746395, -373.1304606946836770 ) ) ;
#15228 = CARTESIAN_POINT ( 'NONE',  ( 779.4709603349208464, -312.3510508353230080, 314.7162404726379918 ) ) ;
#15229 = CARTESIAN_POINT ( 'NONE',  ( -949.5497976682736407, 230.0000000000002274, -210.0000000000000000 ) ) ;
#15230 = CARTESIAN_POINT ( 'NONE',  ( 760.0363995740630116, -82.91815448151682233, 368.7758568127991907 ) ) ;
#15231 = CARTESIAN_POINT ( 'NONE',  ( 751.6929314249748586, -270.9982390220561115, -318.8095938919659034 ) ) ;
#15232 = CARTESIAN_POINT ( 'NONE',  ( 804.4286716492782716, -113.3618753856929260, 345.3141322388244703 ) ) ;
#15233 = SURFACE_STYLE_FILL_AREA ( #27255 ) ;
#15234 = CARTESIAN_POINT ( 'NONE',  ( 815.1787889125755555, -318.8965053807775121, -343.7953271457877804 ) ) ;
#15235 = VECTOR ( 'NONE', #30810, 1000.000000000000000 ) ;
#15236 = CARTESIAN_POINT ( 'NONE',  ( 804.8461984189677878, -2.190881754244347945, 336.9566956441385628 ) ) ;
#15237 = CARTESIAN_POINT ( 'NONE',  ( 763.0537975583475827, -360.4527844766010958, -371.0346526505627480 ) ) ;
#15238 = CARTESIAN_POINT ( 'NONE',  ( 441.1634899080286232, 259.9999999999999432, -191.9749999999972374 ) ) ;
#15239 = CARTESIAN_POINT ( 'NONE',  ( 804.1601925771018387, -391.4419599262317888, 346.5483106153029098 ) ) ;
#15240 = ORIENTED_EDGE ( 'NONE', *, *, #43518, .F. ) ;
#15242 = AXIS2_PLACEMENT_3D ( 'NONE', #14926, #36162, #373 ) ;
#15241 = CARTESIAN_POINT ( 'NONE',  ( 756.3353852180819104, -413.9073299311465348, -331.1735550268788302 ) ) ;
#15243 = CARTESIAN_POINT ( 'NONE',  ( 765.0180583372156207, -216.9982390220562252, -360.0135310231089534 ) ) ;
#15244 = CARTESIAN_POINT ( 'NONE',  ( 801.9858362298568863, -75.07832356259649487, -312.7379699480935642 ) ) ;
#15245 = DIRECTION ( 'NONE',  ( -0.000000000000000000, -0.000000000000000000, 1.000000000000000000 ) ) ;
#15246 = CARTESIAN_POINT ( 'NONE',  ( 815.1787889125755555, -246.8965053807777679, 343.7953271457877804 ) ) ;
#15247 = CARTESIAN_POINT ( 'NONE',  ( 804.9363028652555840, -64.27096629478397460, 338.2165204200192079 ) ) ;
#15248 = CARTESIAN_POINT ( 'NONE',  ( 776.9566956441375396, -228.8965053807778816, -364.8461984189686405 ) ) ;
#15249 = CARTESIAN_POINT ( 'NONE',  ( 762.1405469898971887, -241.5436935675106156, 357.8594530101015607 ) ) ;
#15250 = CIRCLE ( 'NONE', #13019, 18.00000000000001421 ) ;
#15251 = CARTESIAN_POINT ( 'NONE',  ( 815.1787889125755555, -54.89650538077837183, -343.7953271457877804 ) ) ;
#15252 = CARTESIAN_POINT ( 'NONE',  ( 808.1998602359702772, -452.9681489794448908, -337.6500903519150825 ) ) ;
#15253 = ORIENTED_EDGE ( 'NONE', *, *, #25811, .F. ) ;
#15254 = CARTESIAN_POINT ( 'NONE',  ( 805.6418435158337843, -341.4636090269705733, -363.8556311672236916 ) ) ;
#15255 = CARTESIAN_POINT ( 'NONE',  ( 772.5602148656447525, -297.7255117493286889, 305.7998596910095443 ) ) ;
#15256 = CARTESIAN_POINT ( 'NONE',  ( 793.4146539503750546, -25.98741447168755769, 307.6481478633938877 ) ) ;
#15257 = CARTESIAN_POINT ( 'NONE',  ( 766.9102291470427417, -186.5545181178801215, -318.6633372737382501 ) ) ;
#15258 = CARTESIAN_POINT ( 'NONE',  ( 800.0135310231082713, -182.0891481129654323, -325.0180583372163028 ) ) ;
#15259 = CARTESIAN_POINT ( 'NONE',  ( 759.9864689768902508, -386.0891481129647786, -354.9819416627836404 ) ) ;
#15260 = VERTEX_POINT ( 'NONE', #19797 ) ;
#15261 = CARTESIAN_POINT ( 'NONE',  ( 798.7617431975189675, 20.37622189194865285, -323.0428371773161871 ) ) ;
#15262 = VERTEX_POINT ( 'NONE', #37808 ) ;
#15263 = CARTESIAN_POINT ( 'NONE',  ( 746.8695393053150156, -317.9073299311468190, 327.6429770376306010 ) ) ;
#15264 = LINE ( 'NONE', #15699, #6367 ) ;
#15265 = CARTESIAN_POINT ( 'NONE',  ( 766.9102291470427417, -210.5545181178800647, 318.6633372737382501 ) ) ;
#15266 = AXIS2_PLACEMENT_3D ( 'NONE', #42877, #7786, #11478 ) ;
#15267 = CARTESIAN_POINT ( 'NONE',  ( 801.3366627262608972, -368.5328690171409676, 353.0897708529566899 ) ) ;
#15268 = VECTOR ( 'NONE', #20181, 1000.000000000000000 ) ;
#15269 = DIRECTION ( 'NONE',  ( 1.000000000000000000, 0.000000000000000000, 0.000000000000000000 ) ) ;
#15270 = CARTESIAN_POINT ( 'NONE',  ( 796.1575198192839480, -198.0090635724255606, 359.4546378042384163 ) ) ;
#15271 = CARTESIAN_POINT ( 'NONE',  ( 764.8639956371174549, -56.08914811296580893, 319.7806653035542013 ) ) ;
#15272 = EDGE_LOOP ( 'NONE', ( #34038, #7620, #45226, #44553 ) ) ;
#15273 = CARTESIAN_POINT ( 'NONE',  ( 747.6481478633932056, -421.0999726633340288, -353.4146539503763620 ) ) ;
#15274 = AXIS2_PLACEMENT_3D ( 'NONE', #1337, #25125, #15442 ) ;
#15275 = CARTESIAN_POINT ( 'NONE',  ( 814.5518280994195948, -15.72551174932958951, -332.4837098697145166 ) ) ;
#15276 = CARTESIAN_POINT ( 'NONE',  ( 805.0264073115434940, -222.3510508353233206, 339.4763451958999099 ) ) ;
#15277 = AXIS2_PLACEMENT_3D ( 'NONE', #29405, #36778, #19008 ) ;
#15278 = CARTESIAN_POINT ( 'NONE',  ( 767.8955696845333705, -408.4527844766009252, -362.1676090361162323 ) ) ;
#15279 = CARTESIAN_POINT ( 'NONE',  ( 764.8639956371174549, -8.089148112965974136, -319.7806653035542581 ) ) ;
#15280 = CARTESIAN_POINT ( 'NONE',  ( 793.9708237608222134, -454.9181544815156713, 319.2295555964448681 ) ) ;
#15281 = DIRECTION ( 'NONE',  ( 0.000000000000000000, 0.000000000000000000, 1.000000000000000000 ) ) ;
#15282 = CARTESIAN_POINT ( 'NONE',  ( 790.9844846989617508, -262.3726999360617924, -317.2208543904092721 ) ) ;
#15283 = VECTOR ( 'NONE', #25357, 1000.000000000000000 ) ;
#15284 = CARTESIAN_POINT ( 'NONE',  ( 796.9462024416508257, -36.45278447660223975, 308.9653473494370246 ) ) ;
#15285 = CARTESIAN_POINT ( 'NONE',  ( 787.5162901302840055, -107.3618753856928976, 305.4481719005792684 ) ) ;
#15286 = DIRECTION ( 'NONE',  ( 1.000000000000000000, 0.000000000000000000, 0.000000000000000000 ) ) ;
#15287 = EDGE_CURVE ( 'NONE', #45297, #38829, #6157, .T. ) ;
#15288 = DIRECTION ( 'NONE',  ( 1.000000000000000000, 0.000000000000000000, 0.000000000000000000 ) ) ;
#15289 = CARTESIAN_POINT ( 'NONE',  ( 795.8262568251477660, -382.3726999360613945, 308.3538107759623585 ) ) ;
#15290 = LINE ( 'NONE', #4434, #8767 ) ;
#15291 = CARTESIAN_POINT ( 'NONE',  ( 804.7487373415286811, -379.5436935675102745, 364.7487373415288516 ) ) ;
#15292 = CARTESIAN_POINT ( 'NONE',  ( 778.2165204200184689, -310.8164208402377540, -364.9363028652563230 ) ) ;
#15293 = CARTESIAN_POINT ( 'NONE',  ( 779.4709603349208464, -0.3510508353240099355, 314.7162404726379918 ) ) ;
#15294 = CARTESIAN_POINT ( 'NONE',  ( 769.9779781133707957, -187.0999726633346825, 316.7813123517150871 ) ) ;
#15295 = CARTESIAN_POINT ( 'NONE',  ( 802.2119215644370342, -54.00906357242601530, -367.5423716828165084 ) ) ;
#15296 = CARTESIAN_POINT ( 'NONE',  ( 755.8398074228967971, -115.4419599262327409, -333.4516893846970333 ) ) ;
#15297 = CARTESIAN_POINT ( 'NONE',  ( 803.8556311672234642, -129.6237781080508853, 365.6418435158340117 ) ) ;
#15298 = CARTESIAN_POINT ( 'NONE',  ( 797.8594530101009923, -445.5436935675099335, 322.1405469898982119 ) ) ;
#15299 = CARTESIAN_POINT ( 'NONE',  ( 774.6312213355099630, -23.36187538569318889, -364.6798772138717482 ) ) ;
#15300 = CARTESIAN_POINT ( 'NONE',  ( 804.1601925771018387, -127.4419599262326983, -346.5483106153029098 ) ) ;
#15301 = CARTESIAN_POINT ( 'NONE',  ( 797.8594530101008786, -133.5436935675110135, -322.1405469898980982 ) ) ;
#15302 = VECTOR ( 'NONE', #5929, 1000.000000000000000 ) ;
#15303 = CARTESIAN_POINT ( 'NONE',  ( 758.6633372737375112, -428.5328690171409107, -326.9102291470432533 ) ) ;
#15305 = CARTESIAN_POINT ( 'NONE',  ( 788.7366044899766848, -251.9073299311470748, 316.5762568750059813 ) ) ;
#15304 = CARTESIAN_POINT ( 'NONE',  ( 774.6312213355099630, -263.3618753856924855, 364.6798772138717482 ) ) ;
#15306 = DIRECTION ( 'NONE',  ( 0.000000000000000000, 0.000000000000000000, 1.000000000000000000 ) ) ;
#15307 = ORIENTED_EDGE ( 'NONE', *, *, #45291, .F. ) ;
#15308 = CARTESIAN_POINT ( 'NONE',  ( 759.2295555964440155, 7.830767346494148740, 353.9708237608231229 ) ) ;
#15309 = VECTOR ( 'NONE', #29878, 1000.000000000000000 ) ;
#15310 = ORIENTED_EDGE ( 'NONE', *, *, #28382, .T. ) ;
#15311 = CIRCLE ( 'NONE', #531, 20.00000000000004619 ) ;
#15312 = CARTESIAN_POINT ( 'NONE',  ( 814.5518280994195948, -183.7255117493290300, 332.4837098697145166 ) ) ;
#15313 = CARTESIAN_POINT ( 'NONE',  ( 755.5913626894240451, -277.6454272087889308, 346.6156483768012890 ) ) ;
#15314 = EDGE_LOOP ( 'NONE', ( #11064, #9506, #28707, #7733 ) ) ;
#15315 = CARTESIAN_POINT ( 'NONE',  ( 755.1538015810308480, -86.19088175424408860, -343.0433043558613804 ) ) ;
#15316 = CARTESIAN_POINT ( 'NONE',  ( 801.9858362298568863, -219.0783235625960401, 312.7379699480935642 ) ) ;
#15317 = CARTESIAN_POINT ( 'NONE',  ( 767.8955696845334842, -288.4527844766014937, -362.1676090361161755 ) ) ;
#15318 = EDGE_LOOP ( 'NONE', ( #1088, #26857 ) ) ;
#15319 = CARTESIAN_POINT ( 'NONE',  ( 795.1360043628807261, -404.0891481129646081, -360.2193346964456282 ) ) ;
#15320 = CARTESIAN_POINT ( 'NONE',  ( 801.9419747391806368, -66.45278447660216159, -351.9812246680014027 ) ) ;
#15321 = CARTESIAN_POINT ( 'NONE',  ( 755.0488828828309806, -257.8055962898686744, 344.1219089521771934 ) ) ;
#15322 = PLANE ( 'NONE',  #40325 ) ;
#15323 = FACE_OUTER_BOUND ( 'NONE', #28244, .T. ) ;
#15324 = CARTESIAN_POINT ( 'NONE',  ( 750.9282345327678740, -16.91815448151702839, -319.8311093483690115 ) ) ;
#15325 = CARTESIAN_POINT ( 'NONE',  ( 879.9999999999992042, 429.9999999999999432, -224.9999999999999716 ) ) ;
#15326 = ORIENTED_EDGE ( 'NONE', *, *, #17347, .F. ) ;
#15327 = CARTESIAN_POINT ( 'NONE',  ( 813.5763878283155464, -291.8272453906071746, -351.1614460488615350 ) ) ;
#15328 = CARTESIAN_POINT ( 'NONE',  ( 781.2370466360911223, -164.7363362996983938, 304.9990715423533629 ) ) ;
#15330 = CARTESIAN_POINT ( 'NONE',  ( 791.9812246680005501, -308.6346026584195670, -361.9419747391813189 ) ) ;
#15329 = DIRECTION ( 'NONE',  ( 1.000000000000000000, 0.000000000000000000, 0.000000000000000000 ) ) ;
#15331 = LINE ( 'NONE', #32430, #18634 ) ;
#15332 = CARTESIAN_POINT ( 'NONE',  ( 805.2837595273609850, -146.7363362996984506, -340.5290396650784714 ) ) ;
#15333 = EDGE_CURVE ( 'NONE', #34117, #19382, #21193, .T. ) ;
#15334 = DIRECTION ( 'NONE',  ( 1.000000000000000000, 0.000000000000000000, 0.000000000000000000 ) ) ;
#15335 = CARTESIAN_POINT ( 'NONE',  ( 813.9316612368132837, -7.441959926233078448, -348.6739635108323228 ) ) ;
#15336 = CARTESIAN_POINT ( 'NONE',  ( 772.4837098697145166, -335.3618753856921444, -374.5518280994205611 ) ) ;
#15337 = DIRECTION ( 'NONE',  ( -0.000000000000000000, 1.000000000000000000, -0.000000000000000000 ) ) ;
#15338 = CARTESIAN_POINT ( 'NONE',  ( 758.0580252608178853, -54.45278447660219001, 328.0187753319985404 ) ) ;
#15339 = AXIS2_PLACEMENT_3D ( 'NONE', #9550, #28006, #6998 ) ;
#15340 = CARTESIAN_POINT ( 'NONE',  ( 764.1737431748507561, -298.3726999360616787, 371.6461892240376415 ) ) ;
#15341 = CARTESIAN_POINT ( 'NONE',  ( 783.7566961878529810, -240.8965053807777963, -305.1792804349288417 ) ) ;
#15342 = CARTESIAN_POINT ( 'NONE',  ( 767.6429770376289525, -249.1800572038742416, 306.8695393053162093 ) ) ;
#15343 = CARTESIAN_POINT ( 'NONE',  ( 807.5423716828161105, -441.0783235625953580, -362.2119215644372048 ) ) ;
#15344 = DIRECTION ( 'NONE',  ( -1.000000000000000000, -0.000000000000000000, 0.000000000000000000 ) ) ;
#15345 = ORIENTED_EDGE ( 'NONE', *, *, #6009, .F. ) ;
#15346 = CARTESIAN_POINT ( 'NONE',  ( 800.2193346964447755, -330.9982390220558273, 355.1360043628815788 ) ) ;
#15347 = CARTESIAN_POINT ( 'NONE',  ( 779.4763451958990572, -80.73633629969864955, 365.0264073115438919 ) ) ;
#15348 = CARTESIAN_POINT ( 'NONE',  ( 772.3691319403857278, -23.26014174441484883, -315.8894580844506663 ) ) ;
#15349 = PLANE ( 'NONE',  #22504 ) ;
#15350 = CARTESIAN_POINT ( 'NONE',  ( 879.9999999999990905, 479.9999999999998863, -210.0000000000000000 ) ) ;
#15351 = CARTESIAN_POINT ( 'NONE',  ( 761.9338519418445230, -134.5328690171417350, 370.4231160770881957 ) ) ;
#15353 = CARTESIAN_POINT ( 'NONE',  ( 781.8018195045266339, -406.2709662947829088, 365.1927285166406705 ) ) ;
#15352 = CARTESIAN_POINT ( 'NONE',  ( 786.6156483768007774, -169.4419599262325562, 315.5913626894246136 ) ) ;
#15354 = ORIENTED_EDGE ( 'NONE', *, *, #23000, .F. ) ;
#15355 = CARTESIAN_POINT ( 'NONE',  ( 800.7704444035546203, -316.1692326535048210, -326.0291762391768771 ) ) ;
#15356 = CARTESIAN_POINT ( 'NONE',  ( 791.9812246680005501, -164.6346026584200217, 361.9419747391813189 ) ) ;
#15357 = UNCERTAINTY_MEASURE_WITH_UNIT (LENGTH_MEASURE( 1.000000000000000082E-05 ), #25332, 'distance_accuracy_value', 'NONE');
#15358 = CARTESIAN_POINT ( 'NONE',  ( 746.0683387631852383, -331.4419599262320162, -331.3260364891676204 ) ) ;
#15359 = DIRECTION ( 'NONE',  ( 0.000000000000000000, -1.000000000000000000, 0.000000000000000000 ) ) ;
#15360 = CARTESIAN_POINT ( 'NONE',  ( 811.0346526505616112, 9.365397341579420498, 323.0537975583477532 ) ) ;
#15361 = ORIENTED_EDGE ( 'NONE', *, *, #24394, .T. ) ;
#15362 = CARTESIAN_POINT ( 'NONE',  ( 788.7366044899766848, -371.9073299311465917, 316.5762568750059813 ) ) ;
#15363 = EDGE_LOOP ( 'NONE', ( #22382, #549, #26810, #8611 ) ) ;
#15364 = CARTESIAN_POINT ( 'NONE',  ( 759.7806653035534055, -438.9982390220553157, 324.8639956371180801 ) ) ;
#15365 = CARTESIAN_POINT ( 'NONE',  ( 751.6929314249748586, -174.9982390220563673, -318.8095938919659034 ) ) ;
#15366 = ORIENTED_EDGE ( 'NONE', *, *, #27158, .F. ) ;
#15367 = CARTESIAN_POINT ( 'NONE',  ( 774.6858677611749044, -177.7255117493290868, -315.5713283507209894 ) ) ;
#15368 = ORIENTED_EDGE ( 'NONE', *, *, #40459, .F. ) ;
#15369 = AXIS2_PLACEMENT_3D ( 'NONE', #20783, #45284, #5801 ) ;
#15370 = CARTESIAN_POINT ( 'NONE',  ( 798.5707757039680246, -437.4636090269703459, -356.7845633553585003 ) ) ;
#15371 = CARTESIAN_POINT ( 'NONE',  ( 756.5762568750052424, -3.180057203875080063, 348.7366044899774238 ) ) ;
#15372 = CARTESIAN_POINT ( 'NONE',  ( 745.7998596910086917, -221.3618753856925707, 332.5602148656461168 ) ) ;
#15373 = CARTESIAN_POINT ( 'NONE',  ( 805.0264073115434940, -150.3510508353235480, 339.4763451958999099 ) ) ;
#15375 = CARTESIAN_POINT ( 'NONE',  ( -786.4999999999993179, -512.9681489794448908, -339.9999999999999432 ) ) ;
#15374 = DIRECTION ( 'NONE',  ( 1.000000000000000000, -0.000000000000000000, -0.000000000000000000 ) ) ;
#15376 = EDGE_CURVE ( 'NONE', #22437, #38191, #2463, .T. ) ;
#15377 = ORIENTED_EDGE ( 'NONE', *, *, #38278, .T. ) ;
#15378 = CARTESIAN_POINT ( 'NONE',  ( 775.8780910478218402, -417.2817908451522158, -364.9511171171680530 ) ) ;
#15379 = CARTESIAN_POINT ( 'NONE',  ( 1238.921997096861332, 430.0000000000002842, -244.9999999999999716 ) ) ;
#15380 = CARTESIAN_POINT ( 'NONE',  ( 776.2046728542105711, -188.1908817542437760, -304.8212110874238761 ) ) ;
#15381 = CARTESIAN_POINT ( 'NONE',  ( 814.8207195650702488, -74.19088175424410281, 336.2433038121456548 ) ) ;
#15383 = DIRECTION ( 'NONE',  ( 0.000000000000000000, -0.9235249282889854694, -0.3835384033298675499 ) ) ;
#15382 = CARTESIAN_POINT ( 'NONE',  ( -454.7528517110260964, 230.0000000000001421, -122.7905160835438068 ) ) ;
#15384 = CARTESIAN_POINT ( 'NONE',  ( 798.7617431975189675, -339.6237781080502600, -323.0428371773161871 ) ) ;
#15385 = DIRECTION ( 'NONE',  ( -0.000000000000000000, 1.000000000000000000, -0.000000000000000000 ) ) ;
#15386 = CARTESIAN_POINT ( 'NONE',  ( 760.0363995740630116, -202.9181544815164386, -368.7758568127991907 ) ) ;
#15387 = LINE ( 'NONE', #35941, #25958 ) ;
#15389 = EDGE_CURVE ( 'NONE', #10881, #12019, #44975, .T. ) ;
#15388 = DIRECTION ( 'NONE',  ( -1.000000000000000000, 0.000000000000000000, 0.000000000000000000 ) ) ;
#15390 = EDGE_CURVE ( 'NONE', #8326, #35766, #2234, .T. ) ;
#15391 = CARTESIAN_POINT ( 'NONE',  ( 777.5031285880264704, -238.8164208402379813, -374.9108240113588408 ) ) ;
#15392 = DIRECTION ( 'NONE',  ( 0.000000000000000000, -1.000000000000000000, -1.672022627447525240E-16 ) ) ;
#15393 = CARTESIAN_POINT ( 'NONE',  ( 804.4286716492782716, -17.36187538569322086, -345.3141322388244703 ) ) ;
#15394 = CARTESIAN_POINT ( 'NONE',  ( 745.1792804349281596, -182.1908817542437760, 343.7566961878542884 ) ) ;
#15395 = CARTESIAN_POINT ( 'NONE',  ( 793.4146539503750546, -121.9874144716872593, -307.6481478633938877 ) ) ;
#15396 = CARTESIAN_POINT ( 'NONE',  ( 755.2512626584698410, -151.5436935675109851, 315.2512626584710915 ) ) ;
#15397 = CARTESIAN_POINT ( 'NONE',  ( 767.7687537140311633, -359.9073299311467053, -372.7932403749916830 ) ) ;
#15398 = FACE_BOUND ( 'NONE', #24156, .T. ) ;
#15399 = CARTESIAN_POINT ( 'NONE',  ( 794.9999999999993179, 205.0000000000000568, -255.0000000000000000 ) ) ;
#15400 = CARTESIAN_POINT ( 'NONE',  ( 778.2165204200184689, -214.8164208402380666, 364.9363028652563230 ) ) ;
#15401 = CARTESIAN_POINT ( 'NONE',  ( 755.8894580844503253, -15.82724539060794200, 332.3691319403863531 ) ) ;
#15402 = EDGE_CURVE ( 'NONE', #32155, #39971, #6842, .T. ) ;
#15403 = CARTESIAN_POINT ( 'NONE',  ( 767.8955696845333705, -384.4527844766011526, -362.1676090361162323 ) ) ;
#15404 = AXIS2_PLACEMENT_3D ( 'NONE', #35263, #29264, #35955 ) ;
#15405 = CARTESIAN_POINT ( 'NONE',  ( 763.2262854647970016, -440.6346026584191122, -309.2812353651462445 ) ) ;
#15407 = EDGE_CURVE ( 'NONE', #41109, #26139, #21170, .T. ) ;
#15406 = DIRECTION ( 'NONE',  ( -1.880165489482579047E-16, -1.000000000000000000, -0.000000000000000000 ) ) ;
#15408 = CARTESIAN_POINT ( 'NONE',  ( 752.4576283171824116, -21.07832356259667250, 317.7880784355627952 ) ) ;
#15409 = ORIENTED_EDGE ( 'NONE', *, *, #41940, .T. ) ;
#15410 = CARTESIAN_POINT ( 'NONE',  ( 796.7845633553578182, -177.6237781080507148, -358.5707757039688204 ) ) ;
#15411 = ADVANCED_FACE ( 'NONE', ( #17242 ), #24610, .T. ) ;
#15412 = CARTESIAN_POINT ( 'NONE',  ( 774.6858677611749044, -9.725511749329603717, 315.5713283507209894 ) ) ;
#15413 = CARTESIAN_POINT ( 'NONE',  ( 781.2497674668890113, -228.3510508353232922, -375.3608509340180603 ) ) ;
#15414 = DIRECTION ( 'NONE',  ( 0.000000000000000000, 0.000000000000000000, -1.000000000000000000 ) ) ;
#15415 = CARTESIAN_POINT ( 'NONE',  ( 798.0661480581538854, -362.5328690171410813, 309.5768839229118043 ) ) ;
#15416 = CARTESIAN_POINT ( 'NONE',  ( 781.7834795799800531, -82.81642084023846451, -315.0636971347436202 ) ) ;
#15417 = ORIENTED_EDGE ( 'NONE', *, *, #40798, .T. ) ;
#15418 = CARTESIAN_POINT ( 'NONE',  ( 752.4576283171824116, -429.0783235625953580, 317.7880784355627952 ) ) ;
#15419 = CARTESIAN_POINT ( 'NONE',  ( 767.8955696845333705, -144.4527844766018632, -362.1676090361162323 ) ) ;
#15420 = CARTESIAN_POINT ( 'NONE',  ( 754.8072714833581358, -340.8164208402376971, 338.1981804954720587 ) ) ;
#15421 = CARTESIAN_POINT ( 'NONE',  ( 751.9810565676468741, -74.08914811296577341, -360.9747183278973921 ) ) ;
#15422 = CARTESIAN_POINT ( 'NONE',  ( 759.7806653035535192, -54.99823902205672965, -324.8639956371181370 ) ) ;
#15423 = ORIENTED_EDGE ( 'NONE', *, *, #19631, .T. ) ;
#15424 = CARTESIAN_POINT ( 'NONE',  ( 804.4086373105744769, -25.64542720878973014, -333.3843516231986541 ) ) ;
#15425 = ORIENTED_EDGE ( 'NONE', *, *, #30524, .F. ) ;
#15426 = CARTESIAN_POINT ( 'NONE',  ( 793.9708237608222134, -310.9181544815160123, -319.2295555964448681 ) ) ;
#15427 = EDGE_CURVE ( 'NONE', #43717, #28582, #3396, .T. ) ;
#15429 = CARTESIAN_POINT ( 'NONE',  ( 804.8461984189677878, -362.1908817542432644, 336.9566956441385628 ) ) ;
#15428 = CARTESIAN_POINT ( 'NONE',  ( 797.6776695296629214, -43.54369356751131903, 357.6776695296636603 ) ) ;
#15430 = CARTESIAN_POINT ( 'NONE',  ( 791.9812246680005501, -332.6346026584195101, -361.9419747391813189 ) ) ;
#15432 = CARTESIAN_POINT ( 'NONE',  ( 752.4576283171824116, -309.0783235625957559, 317.7880784355627952 ) ) ;
#15431 = CARTESIAN_POINT ( 'NONE',  ( 746.8695393053151292, -413.9073299311465348, 327.6429770376306578 ) ) ;
#15433 = EDGE_CURVE ( 'NONE', #15624, #25647, #34788, .T. ) ;
#15434 = CARTESIAN_POINT ( 'NONE',  ( 790.9844846989617508, -310.3726999360616219, -317.2208543904092721 ) ) ;
#15435 = CARTESIAN_POINT ( 'NONE',  ( 792.1044303154645831, -300.4527844766012663, -317.8323909638837677 ) ) ;
#15436 = DIRECTION ( 'NONE',  ( -0.000000000000000000, -0.000000000000000000, 1.000000000000000000 ) ) ;
#15437 = CARTESIAN_POINT ( 'NONE',  ( 788.7366044899766848, -155.9073299311473306, -316.5762568750059813 ) ) ;
#15438 = CARTESIAN_POINT ( 'NONE',  ( -180.7583438952258916, 294.6698570112193920, -244.9999999999999716 ) ) ;
#15439 = CIRCLE ( 'NONE', #41241, 10.00000000000006395 ) ;
#15440 = CARTESIAN_POINT ( 'NONE',  ( 808.3070685750230950, -426.9982390220554862, 361.1904061080339261 ) ) ;
#15442 = DIRECTION ( 'NONE',  ( 0.000000000000000000, 0.000000000000000000, 1.000000000000000000 ) ) ;
#15441 = DIRECTION ( 'NONE',  ( 1.337618101958019798E-16, -1.000000000000000000, 0.000000000000000000 ) ) ;
#15443 = CARTESIAN_POINT ( 'NONE',  ( 791.0478386215596629, -69.82724539060775726, -306.7653713866226326 ) ) ;
#15444 = DIRECTION ( 'NONE',  ( 0.000000000000000000, 0.000000000000000000, -1.000000000000000000 ) ) ;
#15446 = ADVANCED_FACE ( 'NONE', ( #23924 ), #14480, .F. ) ;
#15445 = LINE ( 'NONE', #29522, #25980 ) ;
#15447 = CARTESIAN_POINT ( 'NONE',  ( 763.8424801807145741, -306.0090635724252479, 320.5453621957614700 ) ) ;
#15448 = CARTESIAN_POINT ( 'NONE',  ( 758.0580252608178853, -150.4527844766018916, 328.0187753319985404 ) ) ;
#15449 = EDGE_LOOP ( 'NONE', ( #32787, #27682, #7146, #23055 ) ) ;
#15450 = CARTESIAN_POINT ( 'NONE',  ( 804.7487373415286811, -139.5436935675110135, -364.7487373415288516 ) ) ;
#15451 = CARTESIAN_POINT ( 'NONE',  ( 755.0488828828309806, -329.8055962898683902, 344.1219089521771934 ) ) ;
#15452 = CARTESIAN_POINT ( 'NONE',  ( 1007.605605532488426, 26.27639943461424110, 900.0000000000004547 ) ) ;
#15453 = CARTESIAN_POINT ( 'NONE',  ( 804.1601925771018387, -415.4419599262318457, -346.5483106153029098 ) ) ;
#15454 = CARTESIAN_POINT ( 'NONE',  ( 813.5763878283155464, -75.82724539060775726, 351.1614460488615350 ) ) ;
#15455 = CARTESIAN_POINT ( 'NONE',  ( 814.5518280994195948, -279.7255117493288026, -332.4837098697145734 ) ) ;
#15456 = CARTESIAN_POINT ( 'NONE',  ( 768.0187753319979720, -128.6346026584201354, 318.0580252608186242 ) ) ;
#15457 = ORIENTED_EDGE ( 'NONE', *, *, #43836, .F. ) ;
#15458 = CARTESIAN_POINT ( 'NONE',  ( 754.0944755984390895, -351.6237781080502032, -364.1009440267246760 ) ) ;
#15459 = CARTESIAN_POINT ( 'NONE',  ( 769.0155153010367712, -10.37269993606250473, 362.7791456095907279 ) ) ;
#15460 = CARTESIAN_POINT ( 'NONE',  ( 749.2812353651451076, -342.4527844766013231, -323.2262854647983090 ) ) ;
#15461 = CARTESIAN_POINT ( 'NONE',  ( 998.9999999999992042, 249.9999999999998863, 360.0000000000000000 ) ) ;
#15462 = CARTESIAN_POINT ( 'NONE',  ( 764.0069404352550464, -399.0783235625955285, 359.2566176426627180 ) ) ;
#15463 = ORIENTED_EDGE ( 'NONE', *, *, #5233, .T. ) ;
#15464 = CARTESIAN_POINT ( 'NONE',  ( 780.5290396650775619, -84.35105083532374692, 365.2837595273619513 ) ) ;
#15465 = CARTESIAN_POINT ( 'NONE',  ( 788.8264449731200330, -429.1800572038737869, -363.6646147819171233 ) ) ;
#15466 = CARTESIAN_POINT ( 'NONE',  ( 800.2193346964447755, -210.9982390220561967, -355.1360043628815788 ) ) ;
#15467 = CARTESIAN_POINT ( 'NONE',  ( 812.6845335610512393, -103.9874144716873161, -353.5525998758768651 ) ) ;
#15468 = FACE_OUTER_BOUND ( 'NONE', #38078, .T. ) ;
#15469 = CARTESIAN_POINT ( 'NONE',  ( 805.9055244015594326, -243.6237781080504590, 315.8990559732753240 ) ) ;
#15470 = CARTESIAN_POINT ( 'NONE',  ( 800.0135310231082713, -38.08914811296587999, 325.0180583372163028 ) ) ;
#15471 = VERTEX_POINT ( 'NONE', #31568 ) ;
#15472 = CARTESIAN_POINT ( 'NONE',  ( 798.7617431975189675, -243.6237781080504590, -323.0428371773161871 ) ) ;
#15473 = CARTESIAN_POINT ( 'NONE',  ( 797.6776695296629214, -235.5436935675107293, 357.6776695296636603 ) ) ;
#15474 = CARTESIAN_POINT ( 'NONE',  ( 763.2262854647970016, 15.36539734157940629, -309.2812353651462445 ) ) ;
#15475 = CARTESIAN_POINT ( 'NONE',  ( 781.2497674668890113, -60.35105083532383219, -375.3608509340180603 ) ) ;
#15476 = FACE_OUTER_BOUND ( 'NONE', #22390, .T. ) ;
#15477 = ORIENTED_EDGE ( 'NONE', *, *, #41497, .T. ) ;
#15478 = ORIENTED_EDGE ( 'NONE', *, *, #19296, .T. ) ;
#15479 = CARTESIAN_POINT ( 'NONE',  ( 745.1792804349281596, -374.1908817542432075, -343.7566961878542884 ) ) ;
#15480 = CARTESIAN_POINT ( 'NONE',  ( 787.4397851343537695, -285.7255117493286889, 374.2001403089903988 ) ) ;
#15481 = CARTESIAN_POINT ( 'NONE',  ( 748.3538107759620743, -16.71468719896031985, 355.8262568251490165 ) ) ;
#15482 = CARTESIAN_POINT ( 'NONE',  ( 763.0428371773158460, -179.4636090269710849, -358.7617431975195359 ) ) ;
#15483 = CARTESIAN_POINT ( 'NONE',  ( 756.3353852180819104, -173.9073299311472169, -331.1735550268788302 ) ) ;
#15484 = CARTESIAN_POINT ( 'NONE',  ( 781.7834795799800531, -394.8164208402374697, -315.0636971347436202 ) ) ;
#15485 = EDGE_LOOP ( 'NONE', ( #28941, #2632, #14678, #29895 ) ) ;
#15486 = CARTESIAN_POINT ( 'NONE',  ( 787.6308680596127942, 12.73985825558503926, -364.1105419155492768 ) ) ;
#15487 = ORIENTED_EDGE ( 'NONE', *, *, #32318, .T. ) ;
#15488 = CARTESIAN_POINT ( 'NONE',  ( 813.1304606946830518, -329.9073299311467053, 352.3570229623690580 ) ) ;
#15489 = LINE ( 'NONE', #923, #10061 ) ;
#15490 = DIRECTION ( 'NONE',  ( -1.000000000000000000, 0.000000000000000000, 0.000000000000000000 ) ) ;
#15491 = CARTESIAN_POINT ( 'NONE',  ( -769.9999999999992042, 240.0000000000000853, -360.0000000000000000 ) ) ;
#15492 = CARTESIAN_POINT ( 'NONE',  ( 793.9708237608222134, -190.9181544815164955, 319.2295555964448681 ) ) ;
#15493 = CARTESIAN_POINT ( 'NONE',  ( 801.9419747391806368, -42.45278447660223264, 351.9812246680014027 ) ) ;
#15494 = ORIENTED_EDGE ( 'NONE', *, *, #7791, .F. ) ;
#15495 = CARTESIAN_POINT ( 'NONE',  ( 795.8262568251477660, -430.3726999360611671, -308.3538107759623585 ) ) ;
#15496 = CARTESIAN_POINT ( 'NONE',  ( 772.4837098697145166, -23.36187538569319244, -374.5518280994205611 ) ) ;
#15497 = CARTESIAN_POINT ( 'NONE',  ( 769.1273215169530886, -238.7146871989596661, 317.4527132478988847 ) ) ;
#15498 = CARTESIAN_POINT ( 'NONE',  ( 759.7806653035534055, -390.9982390220557136, -324.8639956371180801 ) ) ;
#15499 = CARTESIAN_POINT ( 'NONE',  ( 754.8072714833583632, -4.816420840238714085, -338.1981804954721156 ) ) ;
#15500 = CARTESIAN_POINT ( 'NONE',  ( 815.2698199232961542, -448.8164208402371855, 342.5225473063383106 ) ) ;
#15501 = LINE ( 'NONE', #1397, #18570 ) ;
#15502 = CARTESIAN_POINT ( 'NONE',  ( 790.0220218866281812, -247.0999726633344835, -363.2186876482849129 ) ) ;
#15503 = CARTESIAN_POINT ( 'NONE',  ( 745.7998596910086917, -149.3618753856928265, -332.5602148656461168 ) ) ;
#15504 = CARTESIAN_POINT ( 'NONE',  ( 744.7301800767019131, -52.81642084023856398, 337.4774526936615757 ) ) ;
#15505 = CARTESIAN_POINT ( 'NONE',  ( 796.7737145352015204, -92.63460265842026331, 370.7187646348536987 ) ) ;
#15506 = CARTESIAN_POINT ( 'NONE',  ( 776.3558828440975503, 16.45630643248848557, -314.5934542695748064 ) ) ;
#15507 = DIRECTION ( 'NONE',  ( -1.000000000000000000, -0.000000000000000000, -0.000000000000000000 ) ) ;
#15508 = CARTESIAN_POINT ( 'NONE',  ( 781.2370466360911223, -380.7363362996977116, 304.9990715423533629 ) ) ;
#15509 = CARTESIAN_POINT ( 'NONE',  ( 190.7583438952259485, 394.6698570112193920, -274.9999999999999432 ) ) ;
#15510 = CARTESIAN_POINT ( 'NONE',  ( 772.4837098697144029, -359.3618753856920875, 374.5518280994205611 ) ) ;
#15511 = CARTESIAN_POINT ( 'NONE',  ( 758.0580252608178853, -318.4527844766014368, -328.0187753319985404 ) ) ;
#15512 = CARTESIAN_POINT ( 'NONE',  ( 790.8726784830453198, 13.28531280103958423, 362.5472867521010585 ) ) ;
#15513 = CARTESIAN_POINT ( 'NONE',  ( 760.0363995740630116, -106.9181544815167371, -368.7758568127991907 ) ) ;
#15514 = CARTESIAN_POINT ( 'NONE',  ( 769.1273215169530886, -118.7146871989600072, -317.4527132478988847 ) ) ;
#15515 = CARTESIAN_POINT ( 'NONE',  ( 793.4146539503750546, -121.9874144716872593, 307.6481478633938877 ) ) ;
#15516 = CARTESIAN_POINT ( 'NONE',  ( 791.0208441182601291, -452.8006503659887585, 362.4663821942984328 ) ) ;
#15517 = CARTESIAN_POINT ( 'NONE',  ( 803.4237431249931660, -15.18005720387504631, -331.2633955100225194 ) ) ;
#15518 = CARTESIAN_POINT ( 'NONE',  ( 780.5290396650775619, -132.3510508353235764, -365.2837595273619513 ) ) ;
#15519 = CARTESIAN_POINT ( 'NONE',  ( 803.6646147819161570, -137.9073299311473875, -348.8264449731210561 ) ) ;
#15520 = CARTESIAN_POINT ( 'NONE',  ( 804.6798772138708955, -135.7255117493291152, 334.6312213355107019 ) ) ;
#15521 = CARTESIAN_POINT ( 'NONE',  ( 764.0069404352550464, -423.0783235625953580, -359.2566176426627180 ) ) ;
#15523 = CARTESIAN_POINT ( 'NONE',  ( 804.9363028652555840, -256.2709662947834204, 338.2165204200192079 ) ) ;
#15522 = CARTESIAN_POINT ( 'NONE',  ( 756.5762568750052424, -267.1800572038742985, 348.7366044899774238 ) ) ;
#15524 = LINE ( 'NONE', #22884, #7962 ) ;
#15525 = ORIENTED_EDGE ( 'NONE', *, *, #12245, .T. ) ;
#15526 = CARTESIAN_POINT ( 'NONE',  ( 772.3691319403857278, 24.73985825558500551, 315.8894580844506663 ) ) ;
#15527 = ORIENTED_EDGE ( 'NONE', *, *, #40142, .F. ) ;
#15528 = CARTESIAN_POINT ( 'NONE',  ( 772.5602148656447525, -201.7255117493290015, 305.7998596910095443 ) ) ;
#15529 = CARTESIAN_POINT ( 'NONE',  ( 787.5531968255692163, -285.8272453906071178, 316.1348686366205811 ) ) ;
#15530 = CARTESIAN_POINT ( 'NONE',  ( 784.0799538623451781, -395.8055962898682765, 364.6971507214555572 ) ) ;
#15531 = VERTEX_POINT ( 'NONE', #38490 ) ;
#15532 = CARTESIAN_POINT ( 'NONE',  ( 802.9823548866075953, -97.09997266333496668, -330.0799878456151077 ) ) ;
#15533 = CARTESIAN_POINT ( 'NONE',  ( 774.6858677611749044, -273.7255117493288026, -315.5713283507209894 ) ) ;
#15534 = VERTEX_POINT ( 'NONE', #13798 ) ;
#15535 = CARTESIAN_POINT ( 'NONE',  ( 758.0580252608178853, -390.4527844766011526, -328.0187753319985404 ) ) ;
#15536 = CARTESIAN_POINT ( 'NONE',  ( 804.6798772138708955, -39.72551174932951312, -334.6312213355107019 ) ) ;
#15537 = CARTESIAN_POINT ( 'NONE',  ( 754.8983024940795303, -258.8965053807777963, 336.9254006560228163 ) ) ;
#15538 = FACE_BOUND ( 'NONE', #16425, .T. ) ;
#15539 = CARTESIAN_POINT ( 'NONE',  ( -208.8365100919714052, 260.0000000000001137, -199.9999999999926956 ) ) ;
#15540 = CARTESIAN_POINT ( 'NONE',  ( 804.1009440267234822, -23.46360902697155026, -314.0944755984392600 ) ) ;
#15541 = CARTESIAN_POINT ( 'NONE',  ( -468.8365100919714337, 240.0000000000001705, -202.7499999999907345 ) ) ;
#15542 = ORIENTED_EDGE ( 'NONE', *, *, #39901, .T. ) ;
#15543 = CARTESIAN_POINT ( 'NONE',  ( 781.2370466360911223, -308.7363362996979390, -304.9990715423533629 ) ) ;
#15544 = CARTESIAN_POINT ( 'NONE',  ( 805.6418435158337843, -173.4636090269710849, 363.8556311672236916 ) ) ;
#15546 = CARTESIAN_POINT ( 'NONE',  ( 768.0187753319979720, -296.6346026584195670, -318.0580252608186242 ) ) ;
#15545 = CARTESIAN_POINT ( 'NONE',  ( 794.9999999999993179, -365.3551492539851893, 18.13243251470705886 ) ) ;
#15547 = LINE ( 'NONE', #30293, #1565 ) ;
#15548 = CARTESIAN_POINT ( 'NONE',  ( 763.8424801807145741, -162.0090635724256742, -320.5453621957614700 ) ) ;
#15549 = DIRECTION ( 'NONE',  ( 1.000000000000000000, 0.000000000000000000, 0.000000000000000000 ) ) ;
#15550 = CARTESIAN_POINT ( 'NONE',  ( 810.1134526219336749, -8.532869017142163059, -357.8822607201570349 ) ) ;
#15551 = CARTESIAN_POINT ( 'NONE',  ( 792.2312462859673587, -347.9073299311467053, -307.2067596250082602 ) ) ;
#15552 = CARTESIAN_POINT ( 'NONE',  ( -180.7583438952260622, 240.0000000000012506, -244.9999999999999716 ) ) ;
#15553 = CARTESIAN_POINT ( 'NONE',  ( 778.2165204200184689, -46.81642084023858530, 364.9363028652563230 ) ) ;
#15554 = CARTESIAN_POINT ( 'NONE',  ( 747.6481478633932056, -301.0999726633342561, 353.4146539503763620 ) ) ;
#15555 = CARTESIAN_POINT ( 'NONE',  ( 772.4837098697144029, -263.3618753856924855, 374.5518280994205611 ) ) ;
#15556 = CARTESIAN_POINT ( 'NONE',  ( 793.4146539503750546, -433.9874144716862361, -307.6481478633938877 ) ) ;
#15557 = LINE ( 'NONE', #1670, #35773 ) ;
#15558 = FACE_OUTER_BOUND ( 'NONE', #27000, .T. ) ;
#15559 = CARTESIAN_POINT ( 'NONE',  ( 771.1735550268778070, -369.1800572038739574, 316.3353852180827630 ) ) ;
#15560 = CARTESIAN_POINT ( 'NONE',  ( 779.4763451958990572, -128.7363362996984790, 365.0264073115438919 ) ) ;
#15561 = CARTESIAN_POINT ( 'NONE',  ( 766.7756240680305382, -14.53286901714214707, -361.5560724626415663 ) ) ;
#15562 = CARTESIAN_POINT ( 'NONE',  ( 180.7583438952258348, 394.6698570112193920, -274.9999999999999432 ) ) ;
#15563 = CYLINDRICAL_SURFACE ( 'NONE', #14451, 6.118999999999985562 ) ;
#15564 = CARTESIAN_POINT ( 'NONE',  ( 801.9419747391806368, -378.4527844766011526, 351.9812246680014027 ) ) ;
#15565 = VERTEX_POINT ( 'NONE', #13557 ) ;
#15566 = CARTESIAN_POINT ( 'NONE',  ( 794.1144889064781864, -322.1692326535048210, -360.9840315886528401 ) ) ;
#15567 = CARTESIAN_POINT ( 'NONE',  ( 801.9419747391806368, -162.4527844766018632, 351.9812246680014027 ) ) ;
#15568 = CARTESIAN_POINT ( 'NONE',  ( 813.9316612368132837, -343.4419599262320162, -348.6739635108323228 ) ) ;
#15569 = FACE_OUTER_BOUND ( 'NONE', #26989, .T. ) ;
#15570 = EDGE_CURVE ( 'NONE', #27963, #19960, #28088, .T. ) ;
#15571 = ORIENTED_EDGE ( 'NONE', *, *, #31782, .F. ) ;
#15572 = CARTESIAN_POINT ( 'NONE',  ( 778.1981804954714335, -346.2709662947830793, 314.8072714833589885 ) ) ;
#15573 = ORIENTED_EDGE ( 'NONE', *, *, #5443, .F. ) ;
#15574 = CARTESIAN_POINT ( 'NONE',  ( 788.7366044899766848, -443.9073299311464780, 316.5762568750059813 ) ) ;
#15575 = EDGE_CURVE ( 'NONE', #9331, #6874, #39681, .T. ) ;
#15576 = CARTESIAN_POINT ( 'NONE',  ( 745.7998596910086917, -173.3618753856927128, -332.5602148656461168 ) ) ;
#15577 = CARTESIAN_POINT ( 'NONE',  ( 754.9967657858570647, -97.54369356751114140, 365.0032342141425943 ) ) ;
#15578 = VERTEX_POINT ( 'NONE', #3846 ) ;
#15579 = CARTESIAN_POINT ( 'NONE',  ( 759.9864689768902508, -170.0891481129654608, -354.9819416627836404 ) ) ;
#15580 = EDGE_LOOP ( 'NONE', ( #30005, #31715 ) ) ;
#15581 = CARTESIAN_POINT ( 'NONE',  ( 790.0220218866281812, -439.0999726633339719, -363.2186876482849129 ) ) ;
#15582 = CARTESIAN_POINT ( 'NONE',  ( 762.3223304703356007, -7.543693567511430942, 322.3223304703362828 ) ) ;
#15583 = CARTESIAN_POINT ( 'NONE',  ( 766.7756240680305382, -158.5328690171417065, 361.5560724626415663 ) ) ;
#15585 = DIRECTION ( 'NONE',  ( 1.000000000000000000, -0.000000000000000000, -0.000000000000000000 ) ) ;
#15584 = FACE_OUTER_BOUND ( 'NONE', #10124, .T. ) ;
#15586 = VERTEX_POINT ( 'NONE', #31328 ) ;
#15587 = CARTESIAN_POINT ( 'NONE',  ( 755.5913626894240451, -421.6454272087885329, -346.6156483768012890 ) ) ;
#15588 = CARTESIAN_POINT ( 'NONE',  ( 784.4999999999993179, -512.9681489794448908, -352.0000000000000000 ) ) ;
#15589 = CARTESIAN_POINT ( 'NONE',  ( 814.8207195650702488, -194.1908817542437475, -336.2433038121456548 ) ) ;
#15590 = CARTESIAN_POINT ( 'NONE',  ( 776.2046728542105711, -68.19088175424413123, 304.8212110874238761 ) ) ;
#15592 = CARTESIAN_POINT ( 'NONE',  ( 794.9819416627830151, -204.9982390220562820, -319.9864689768909898 ) ) ;
#15591 = LINE ( 'NONE', #33156, #4238 ) ;
#15593 = CARTESIAN_POINT ( 'NONE',  ( 802.7791456095903868, -316.7146871989593819, -329.0155153010375102 ) ) ;
#15594 = CARTESIAN_POINT ( 'NONE',  ( 794.9999999999993179, 205.0000000000000568, -235.0000000000000000 ) ) ;
#15595 = CARTESIAN_POINT ( 'NONE',  ( 814.4686193811664907, -219.2817908451527558, -346.2056067578752732 ) ) ;
#15596 = DIRECTION ( 'NONE',  ( -0.000000000000000000, -0.3826834323650838421, -0.9238795325112891810 ) ) ;
#15597 = CARTESIAN_POINT ( 'NONE',  ( 799.9999999999993179, 166.4563064324884465, 319.9999999999999432 ) ) ;
#15598 = CARTESIAN_POINT ( 'NONE',  ( 798.5707757039680246, -53.46360902697146855, -356.7845633553585003 ) ) ;
#15599 = CARTESIAN_POINT ( 'NONE',  ( 796.1575198192839480, -414.0090635724249637, 359.4546378042384163 ) ) ;
#15600 = CARTESIAN_POINT ( 'NONE',  ( 782.5225473063383106, -238.2709662947833920, -375.2698199232970637 ) ) ;
#15601 = CARTESIAN_POINT ( 'NONE',  ( -789.9999999999992042, 240.0000000000000568, -319.9999999999999432 ) ) ;
#15602 = CARTESIAN_POINT ( 'NONE',  ( 755.0636971347428243, -28.27096629478409540, -341.7834795799807353 ) ) ;
#15603 = CARTESIAN_POINT ( 'NONE',  ( 745.7194118038753459, -181.6454272087892434, 348.7631598425976449 ) ) ;
#15604 = CARTESIAN_POINT ( 'NONE',  ( 811.6461892240364477, -148.7146871989598935, -324.1737431748509835 ) ) ;
#15605 = CARTESIAN_POINT ( 'NONE',  ( 748.9653473494363425, -146.6346026584200217, 356.9462024416521331 ) ) ;
#15606 = CARTESIAN_POINT ( 'NONE',  ( 763.0537975583475827, -384.4527844766011526, -371.0346526505627480 ) ) ;
#15607 = CARTESIAN_POINT ( 'NONE',  ( 989.9999999999992042, 469.9999999999999432, 210.0000000000000000 ) ) ;
#15608 = CARTESIAN_POINT ( 'NONE',  ( 799.9999999999993179, 205.0000000000000568, 350.0000000000000000 ) ) ;
#15609 = CARTESIAN_POINT ( 'NONE',  ( 788.7366044899766848, -251.9073299311470748, 316.5762568750059813 ) ) ;
#15610 = CARTESIAN_POINT ( 'NONE',  ( 775.8780910478218402, -9.281790845153418346, 364.9511171171680530 ) ) ;
#15611 = CARTESIAN_POINT ( 'NONE',  ( 797.6776695296629214, -379.5436935675102745, -357.6776695296636603 ) ) ;
#15612 = DIRECTION ( 'NONE',  ( 0.000000000000000000, 0.000000000000000000, 1.000000000000000000 ) ) ;
#15613 = CARTESIAN_POINT ( 'NONE',  ( 796.9462024416508257, -444.4527844766009821, -308.9653473494370246 ) ) ;
#15614 = CARTESIAN_POINT ( 'NONE',  ( -879.9999999999992042, 240.0000000000002274, -244.9999999999999716 ) ) ;
#15616 = CARTESIAN_POINT ( 'NONE',  ( 804.4286716492782716, -305.3618753856922581, 345.3141322388244703 ) ) ;
#15615 = CARTESIAN_POINT ( 'NONE',  ( 754.9735926884551418, -66.35105083532378956, 340.5236548041000333 ) ) ;
#15617 = ORIENTED_EDGE ( 'NONE', *, *, #5541, .T. ) ;
#15618 = ADVANCED_FACE ( 'NONE', ( #45668, #42184 ), #3151, .F. ) ;
#15619 = CARTESIAN_POINT ( 'NONE',  ( 773.3843516231979720, -229.4419599262323572, -364.4086373105754433 ) ) ;
#15620 = CARTESIAN_POINT ( 'NONE',  ( 785.3687786644884454, -11.36187538569323863, 315.3201227861279676 ) ) ;
#15621 = CIRCLE ( 'NONE', #13420, 10.00000000000000888 ) ;
#15622 = CARTESIAN_POINT ( 'NONE',  ( 815.0009284576459549, -222.3510508353233206, -338.7629533639073429 ) ) ;
#15623 = CARTESIAN_POINT ( 'NONE',  ( 815.0009284576459549, -342.3510508353228943, 338.7629533639073429 ) ) ;
#15624 = VERTEX_POINT ( 'NONE', #14020 ) ;
#15625 = CARTESIAN_POINT ( 'NONE',  ( 755.3201227861273992, -339.7255117493285184, 345.3687786644892981 ) ) ;
#15626 = ADVANCED_FACE ( 'NONE', ( #38045 ), #41739, .F. ) ;
#15627 = CARTESIAN_POINT ( 'NONE',  ( 748.9653473494363425, -74.63460265842032015, -356.9462024416521331 ) ) ;
#15628 = EDGE_CURVE ( 'NONE', #5961, #42633, #149, .T. ) ;
#15629 = CARTESIAN_POINT ( 'NONE',  ( 755.0636971347428243, -76.27096629478394618, -341.7834795799807353 ) ) ;
#15630 = ORIENTED_EDGE ( 'NONE', *, *, #10865, .T. ) ;
#15631 = CARTESIAN_POINT ( 'NONE',  ( 766.0291762391763086, -10.91815448151704793, -360.7704444035551319 ) ) ;
#15632 = VERTEX_POINT ( 'NONE', #10314 ) ;
#15633 = CARTESIAN_POINT ( 'NONE',  ( 755.3028492785439312, -303.2817908451525000, -335.9200461376539693 ) ) ;
#15635 = CARTESIAN_POINT ( 'NONE',  ( 766.9102291470427417, -354.5545181178796383, 318.6633372737382501 ) ) ;
#15634 = CARTESIAN_POINT ( 'NONE',  ( 781.8018195045266339, -70.27096629478397460, 365.1927285166406705 ) ) ;
#15638 = CARTESIAN_POINT ( 'NONE',  ( 746.7653713866222915, -329.2601417444138860, 351.0478386215610271 ) ) ;
#15637 = CARTESIAN_POINT ( 'NONE',  ( 789.5584187865343893, -452.9681489794450613, 363.1011989789364520 ) ) ;
#15636 = CARTESIAN_POINT ( 'NONE',  ( 808.3070685750232087, -426.9982390220555430, 361.1904061080339829 ) ) ;
#15639 = CARTESIAN_POINT ( 'NONE',  ( 807.5423716828161105, -105.0783235625964096, 362.2119215644372048 ) ) ;
#15640 = CARTESIAN_POINT ( 'NONE',  ( 755.8894580844503253, -327.8272453906069472, -332.3691319403863531 ) ) ;
#15641 = CARTESIAN_POINT ( 'NONE',  ( 785.3687786644884454, -323.3618753856923149, -315.3201227861279676 ) ) ;
#15642 = CARTESIAN_POINT ( 'NONE',  ( 803.4237431249931660, -159.1800572038746111, -331.2633955100225194 ) ) ;
#15643 = ADVANCED_FACE ( 'NONE', ( #10092 ), #45435, .F. ) ;
#15644 = CARTESIAN_POINT ( 'NONE',  ( 745.0891759886404770, -412.2709662947829088, 342.4968714119734159 ) ) ;
#15645 = SHAPE_REPRESENTATION ( 'Metal Bar', ( #26858 ), #23892 ) ;
#15647 = DIRECTION ( 'NONE',  ( -1.000000000000000000, 0.000000000000000000, 0.000000000000000000 ) ) ;
#15646 = DIRECTION ( 'NONE',  ( -0.7071067811865697772, 0.000000000000000000, -0.7071067811865252573 ) ) ;
#15648 = EDGE_CURVE ( 'NONE', #5823, #26364, #24386, .T. ) ;
#15649 = CARTESIAN_POINT ( 'NONE',  ( 815.3608509340175488, -122.7363362996985074, -341.2497674668889545 ) ) ;
#15650 = DIRECTION ( 'NONE',  ( -1.000000000000000000, -0.000000000000000000, -0.000000000000000000 ) ) ;
#15651 = LINE ( 'NONE', #29731, #20833 ) ;
#15652 = CARTESIAN_POINT ( 'NONE',  ( 755.3028492785439312, -303.2817908451525000, 335.9200461376539693 ) ) ;
#15653 = CARTESIAN_POINT ( 'NONE',  ( 797.8594530101008786, -181.5436935675108145, 322.1405469898980982 ) ) ;
#15654 = EDGE_CURVE ( 'NONE', #4054, #25632, #20485, .T. ) ;
#15655 = ORIENTED_EDGE ( 'NONE', *, *, #37723, .T. ) ;
#15656 = AXIS2_PLACEMENT_3D ( 'NONE', #4748, #8445, #23640 ) ;
#15657 = CARTESIAN_POINT ( 'NONE',  ( 782.5225473063383106, -142.2709662947837330, -375.2698199232970637 ) ) ;
#15658 = DIRECTION ( 'NONE',  ( -0.000000000000000000, 1.000000000000000000, -0.000000000000000000 ) ) ;
#15659 = CARTESIAN_POINT ( 'NONE',  ( 754.3581564841646241, -89.46360902697134065, 316.1443688327762516 ) ) ;
#15660 = CARTESIAN_POINT ( 'NONE',  ( 813.1304606946830518, -257.9073299311469896, -352.3570229623690580 ) ) ;
#15661 = CARTESIAN_POINT ( 'NONE',  ( 814.5518280994195948, -447.7255117493281205, -332.4837098697145166 ) ) ;
#15662 = CARTESIAN_POINT ( 'NONE',  ( 797.8594530101008786, -109.5436935675110988, 322.1405469898980982 ) ) ;
#15663 = CARTESIAN_POINT ( 'NONE',  ( 745.1769319972822814, -329.8055962898683902, -346.2694204179732083 ) ) ;
#15664 = CARTESIAN_POINT ( 'NONE',  ( 763.2262854647970016, -80.63460265842029173, -309.2812353651462445 ) ) ;
#15665 = EDGE_CURVE ( 'NONE', #44996, #24418, #38275, .T. ) ;
#15666 = CARTESIAN_POINT ( 'NONE',  ( 800.9840315886518738, -28.91815448151699286, 354.1144889064786412 ) ) ;
#15667 = CARTESIAN_POINT ( 'NONE',  ( 813.1304606946830518, -353.9073299311467053, -352.3570229623690580 ) ) ;
#15668 = CARTESIAN_POINT ( 'NONE',  ( -775.4999999999993179, 22.32581219114657856, 895.6886905569881492 ) ) ;
#15669 = CARTESIAN_POINT ( 'NONE',  ( 760.5453621957607311, -381.0783235625954717, 323.8424801807151425 ) ) ;
#15670 = ORIENTED_EDGE ( 'NONE', *, *, #22881, .T. ) ;
#15671 = EDGE_CURVE ( 'NONE', #34011, #31920, #18852, .T. ) ;
#15672 = CARTESIAN_POINT ( 'NONE',  ( 788.8264449731200330, -213.1800572038743553, -363.6646147819171233 ) ) ;
#15673 = CIRCLE ( 'NONE', #41495, 2.749999999999863665 ) ;
#15674 = CARTESIAN_POINT ( 'NONE',  ( 800.1688906516307043, -106.1692326535054889, -369.0717654672308186 ) ) ;
#15675 = CYLINDRICAL_SURFACE ( 'NONE', #7864, 6.118999999999985562 ) ;
#15676 = CARTESIAN_POINT ( 'NONE',  ( 771.2368401574024119, -253.4419599262323572, 374.2805881961240857 ) ) ;
#15677 = CARTESIAN_POINT ( 'NONE',  ( 781.7834795799800531, -34.81642084023861372, 315.0636971347436202 ) ) ;
#15678 = CARTESIAN_POINT ( 'NONE',  ( 787.6308680596127942, -251.2601417444141134, -364.1105419155492768 ) ) ;
#15679 = ADVANCED_FACE ( 'NONE', ( #14930 ), #4528, .F. ) ;
#15680 = CARTESIAN_POINT ( 'NONE',  ( 762.3223304703356007, -223.5436935675107577, 322.3223304703362828 ) ) ;
#15681 = EDGE_CURVE ( 'NONE', #17123, #38546, #23021, .T. ) ;
#15682 = CARTESIAN_POINT ( 'NONE',  ( 791.1614460488616487, -419.2601417444136587, -373.5763878283158874 ) ) ;
#15683 = CARTESIAN_POINT ( 'NONE',  ( 805.9055244015594326, -75.62377810805104161, -315.8990559732753240 ) ) ;
#15684 = CARTESIAN_POINT ( 'NONE',  ( 779.9999999999992042, 16.45630643248849267, 370.0000000000000568 ) ) ;
#15685 = ORIENTED_EDGE ( 'NONE', *, *, #45012, .F. ) ;
#15686 = VERTEX_POINT ( 'NONE', #1498 ) ;
#15687 = CARTESIAN_POINT ( 'NONE',  ( 811.3240766477731540, -364.3726999360614514, -355.6651683502462902 ) ) ;
#15688 = CARTESIAN_POINT ( 'NONE',  ( 785.3687786644884454, -227.3618753856925707, -315.3201227861279676 ) ) ;
#15689 = CARTESIAN_POINT ( 'NONE',  ( 751.9810565676468741, -314.0891481129650629, 360.9747183278973921 ) ) ;
#15690 = CARTESIAN_POINT ( 'NONE',  ( 752.4576283171824116, -21.07832356259667250, 317.7880784355627952 ) ) ;
#15691 = CARTESIAN_POINT ( 'NONE',  ( 802.9823548866075953, -217.0999726633345972, -330.0799878456151077 ) ) ;
#15692 = CARTESIAN_POINT ( 'NONE',  ( 788.8264449731200330, -189.1800572038744122, -363.6646147819171233 ) ) ;
#15693 = CARTESIAN_POINT ( 'NONE',  ( 803.6646147819162707, -377.9073299311465917, -348.8264449731211130 ) ) ;
#15694 = ORIENTED_EDGE ( 'NONE', *, *, #25580, .F. ) ;
#15695 = CARTESIAN_POINT ( 'NONE',  ( 794.9819416627830151, -204.9982390220562820, 319.9864689768909898 ) ) ;
#15696 = CARTESIAN_POINT ( 'NONE',  ( 794.9819416627830151, -108.9982390220565804, -319.9864689768909898 ) ) ;
#15697 = ORIENTED_EDGE ( 'NONE', *, *, #30109, .T. ) ;
#15698 = CARTESIAN_POINT ( 'NONE',  ( 754.9967657858570647, -337.5436935675102177, 365.0032342141425374 ) ) ;
#15699 = CARTESIAN_POINT ( 'NONE',  ( -26.63011601220122060, -496.5085659523897448, -356.8883017825714319 ) ) ;
#15700 = DIRECTION ( 'NONE',  ( 0.000000000000000000, 0.000000000000000000, 1.000000000000000000 ) ) ;
#15701 = CARTESIAN_POINT ( 'NONE',  ( 799.9999999999993179, -512.9681489794448908, -339.9999999999999432 ) ) ;
#15702 = CARTESIAN_POINT ( 'NONE',  ( 766.0291762391763086, -178.9181544815165239, 360.7704444035551319 ) ) ;
#15703 = CARTESIAN_POINT ( 'NONE',  ( 774.6312213355099630, -71.36187538569302546, 364.6798772138717482 ) ) ;
#15704 = VERTEX_POINT ( 'NONE', #4077 ) ;
#15705 = CARTESIAN_POINT ( 'NONE',  ( 761.4292242960306112, 6.536390973028352924, -323.2154366446414429 ) ) ;
#15706 = AXIS2_PLACEMENT_3D ( 'NONE', #3847, #24611, #38728 ) ;
#15707 = CARTESIAN_POINT ( 'NONE',  ( 814.9108240113580450, -40.27096629478405987, -337.5031285880265273 ) ) ;
#15708 = AXIS2_PLACEMENT_3D ( 'NONE', #30058, #2104, #43911 ) ;
#15709 = CARTESIAN_POINT ( 'NONE',  ( 799.4546378042377910, -225.0783235625959833, 356.1575198192848006 ) ) ;
#15710 = CARTESIAN_POINT ( 'NONE',  ( 797.8594530101008786, -397.5436935675100472, -322.1405469898980982 ) ) ;
#15711 = CARTESIAN_POINT ( 'NONE',  ( 778.2165204200184689, -22.81642084023865280, -364.9363028652563230 ) ) ;
#15712 = CARTESIAN_POINT ( 'NONE',  ( 811.0346526505616112, -422.6346026584192259, 323.0537975583477532 ) ) ;
#15713 = CARTESIAN_POINT ( 'NONE',  ( 779.9999999999992042, 16.45630643248849267, 339.9999999999999432 ) ) ;
#15714 = CARTESIAN_POINT ( 'NONE',  ( 793.9708237608222134, -262.9181544815162965, -319.2295555964448681 ) ) ;
#15715 = CARTESIAN_POINT ( 'NONE',  ( 808.0189434323515343, -158.0891481129655176, -319.0252816721025511 ) ) ;
#15716 = CARTESIAN_POINT ( 'NONE',  ( 772.4837098697144029, -47.36187538569312494, 374.5518280994205611 ) ) ;
#15717 = CARTESIAN_POINT ( 'NONE',  ( 758.8095938919642549, -128.0891481129655176, 311.6929314249763365 ) ) ;
#15718 = CARTESIAN_POINT ( 'NONE',  ( 770.7832876896738981, 16.45630643248850333, -316.4833103687052471 ) ) ;
#15719 = ADVANCED_FACE ( 'NONE', ( #39658 ), #1288, .F. ) ;
#15720 = CARTESIAN_POINT ( 'NONE',  ( -786.4999999999993179, 35.55895481007114967, 914.5706932916501728 ) ) ;
#15721 = CARTESIAN_POINT ( 'NONE',  ( 805.0032342141412300, -373.5436935675101040, 314.9967657858571783 ) ) ;
#15722 = CARTESIAN_POINT ( 'NONE',  ( 794.9819416627830151, -324.9982390220559409, -319.9864689768909898 ) ) ;
#15723 = CARTESIAN_POINT ( 'NONE',  ( 754.9735926884551418, 5.648949164675971524, 340.5236548041000333 ) ) ;
#15724 = CARTESIAN_POINT ( 'NONE',  ( 762.1177392798416577, -114.5545181178803631, -309.8865473780659272 ) ) ;
#15725 = CARTESIAN_POINT ( 'NONE',  ( 763.2154366446407039, -117.6237781080509279, -321.4292242960311228 ) ) ;
#15726 = CARTESIAN_POINT ( 'NONE',  ( 815.0009284576459549, -126.3510508353236048, 338.7629533639073429 ) ) ;
#15727 = CARTESIAN_POINT ( 'NONE',  ( 797.6776695296629214, -451.5436935675099903, 357.6776695296636603 ) ) ;
#15728 = CARTESIAN_POINT ( 'NONE',  ( 778.1981804954714335, -34.27096629478407408, -314.8072714833589885 ) ) ;
#15729 = CARTESIAN_POINT ( 'NONE',  ( 786.6156483768007774, -121.4419599262327267, -315.5913626894246136 ) ) ;
#15730 = CARTESIAN_POINT ( 'NONE',  ( 803.4237431249931660, -135.1800572038746679, -331.2633955100225194 ) ) ;
#15731 = CARTESIAN_POINT ( 'NONE',  ( 781.7834795799800531, -130.8164208402383224, 315.0636971347436202 ) ) ;
#15732 = CARTESIAN_POINT ( 'NONE',  ( 789.6640940660590786, -442.9180389616178672, -363.1300863558843162 ) ) ;
#15734 = CARTESIAN_POINT ( 'NONE',  ( 785.3687786644885591, -251.3618753856923718, 315.3201227861280813 ) ) ;
#15733 = CARTESIAN_POINT ( 'NONE',  ( 755.0636971347428243, -268.2709662947833067, 341.7834795799807353 ) ) ;
#15735 = AXIS2_PLACEMENT_3D ( 'NONE', #19133, #40823, #5717 ) ;
#15736 = DIRECTION ( 'NONE',  ( -1.000000000000000000, -0.000000000000000000, -0.000000000000000000 ) ) ;
#15737 = ORIENTED_EDGE ( 'NONE', *, *, #40568, .T. ) ;
#15738 = CARTESIAN_POINT ( 'NONE',  ( 804.9363028652555840, -448.2709662947827951, 338.2165204200192079 ) ) ;
#15739 = AXIS2_PLACEMENT_3D ( 'NONE', #35347, #18285, #17586 ) ;
#15740 = CARTESIAN_POINT ( 'NONE',  ( 748.6759233522253680, -280.3726999360616787, -324.3348316497537098 ) ) ;
#15741 = ORIENTED_EDGE ( 'NONE', *, *, #10512, .T. ) ;
#15742 = DIRECTION ( 'NONE',  ( 1.000000000000000000, 0.000000000000000000, 0.000000000000000000 ) ) ;
#15743 = CARTESIAN_POINT ( 'NONE',  ( 796.7737145352015204, -212.6346026584198796, 370.7187646348536987 ) ) ;
#15744 = CARTESIAN_POINT ( 'NONE',  ( 804.6971507214547046, -291.2817908451525000, 344.0799538623459739 ) ) ;
#15745 = CARTESIAN_POINT ( 'NONE',  ( 799.4546378042377910, -393.0783235625954717, 356.1575198192848006 ) ) ;
#15746 = ORIENTED_EDGE ( 'NONE', *, *, #27251, .F. ) ;
#15747 = CARTESIAN_POINT ( 'NONE',  ( 779.4763451958990572, -104.7363362996985785, -365.0264073115438919 ) ) ;
#15748 = CARTESIAN_POINT ( 'NONE',  ( 757.8323909638828582, -290.6346026584196238, -352.1044303154654358 ) ) ;
#15749 = VERTEX_POINT ( 'NONE', #11012 ) ;
#15750 = CARTESIAN_POINT ( 'NONE',  ( 791.9812246680005501, -380.6346026584192828, -361.9419747391813189 ) ) ;
#15751 = CARTESIAN_POINT ( 'NONE',  ( 785.3687786644884454, -83.36187538569296862, -315.3201227861279676 ) ) ;
#15752 = CIRCLE ( 'NONE', #27547, 12.00000000000001066 ) ;
#15753 = CARTESIAN_POINT ( 'NONE',  ( 764.0069404352550464, -279.0783235625958127, 359.2566176426627180 ) ) ;
#15754 = DIRECTION ( 'NONE',  ( 0.000000000000000000, 0.000000000000000000, 1.000000000000000000 ) ) ;
#15755 = DIRECTION ( 'NONE',  ( 0.7071067811865753283, 0.000000000000000000, 0.7071067811865198172 ) ) ;
#15756 = CARTESIAN_POINT ( 'NONE',  ( 766.4474001241216001, -19.09997266333520116, -307.3154664389482491 ) ) ;
#15757 = LINE ( 'NONE', #15325, #30675 ) ;
#15758 = ORIENTED_EDGE ( 'NONE', *, *, #35167, .T. ) ;
#15759 = CARTESIAN_POINT ( 'NONE',  ( 786.2694204179717872, -309.2817908451525568, -305.1769319972829067 ) ) ;
#15760 = CARTESIAN_POINT ( 'NONE',  ( 748.6759233522253680, -208.3726999360619061, 324.3348316497537098 ) ) ;
#15762 = CARTESIAN_POINT ( 'NONE',  ( 792.1044303154645831, -276.4527844766013800, -317.8323909638837677 ) ) ;
#15761 = DIRECTION ( 'NONE',  ( 0.000000000000000000, 0.000000000000000000, 1.000000000000000000 ) ) ;
#15763 = FACE_OUTER_BOUND ( 'NONE', #3304, .T. ) ;
#15764 = CARTESIAN_POINT ( 'NONE',  ( 784.1219089521767955, -165.2817908451529547, -315.0488828828318333 ) ) ;
#15765 = CARTESIAN_POINT ( 'NONE',  ( 755.2512626584698410, -7.543693567511430942, 315.2512626584710915 ) ) ;
#15766 = AXIS2_PLACEMENT_3D ( 'NONE', #45200, #13336, #17248 ) ;
#15767 = CARTESIAN_POINT ( 'NONE',  ( 794.9999999999993179, 240.0000000000000853, -275.0000000000000000 ) ) ;
#15768 = CARTESIAN_POINT ( 'NONE',  ( 772.5602148656447525, -345.7255117493285184, -305.7998596910095443 ) ) ;
#15769 = PRESENTATION_LAYER_ASSIGNMENT (  '', '', ( #18746 ) ) ;
#15770 = SURFACE_SIDE_STYLE ('',( #5597 ) ) ;
#15771 = CARTESIAN_POINT ( 'NONE',  ( 757.8323909638827445, -50.63460265842036989, 352.1044303154654358 ) ) ;
#15772 = CARTESIAN_POINT ( 'NONE',  ( 764.1737431748507561, -274.3726999360617356, 371.6461892240376415 ) ) ;
#15773 = CARTESIAN_POINT ( 'NONE',  ( 782.5225473063381969, -262.2709662947831930, 375.2698199232970637 ) ) ;
#15774 = CARTESIAN_POINT ( 'NONE',  ( 767.6429770376289525, 14.81994279612486309, -306.8695393053162093 ) ) ;
#15775 = FACE_BOUND ( 'NONE', #36415, .T. ) ;
#15776 = DIRECTION ( 'NONE',  ( -1.000000000000000000, 0.000000000000000000, 0.000000000000000000 ) ) ;
#15777 = CARTESIAN_POINT ( 'NONE',  ( 778.1981804954714335, -346.2709662947830793, 314.8072714833589885 ) ) ;
#15778 = CARTESIAN_POINT ( 'NONE',  ( 776.9254006560222479, -116.1908817542440033, 314.8983024940802125 ) ) ;
#15779 = CARTESIAN_POINT ( 'NONE',  ( 765.8855110935204493, 1.830767346494167391, -319.0159684113471599 ) ) ;
#15780 = DIRECTION ( 'NONE',  ( 0.000000000000000000, 0.000000000000000000, 1.000000000000000000 ) ) ;
#15781 = AXIS2_PLACEMENT_3D ( 'NONE', #4917, #19445, #15761 ) ;
#15782 = DIRECTION ( 'NONE',  ( 0.000000000000000000, -0.6438296778008156807, -0.7651688349527167032 ) ) ;
#15783 = CARTESIAN_POINT ( 'NONE',  ( 756.5762568750052424, -387.1800572038738437, 348.7366044899774238 ) ) ;
#15784 = ORIENTED_EDGE ( 'NONE', *, *, #18463, .T. ) ;
#15785 = CARTESIAN_POINT ( 'NONE',  ( 796.7845633553578182, -345.6237781080501463, -358.5707757039688204 ) ) ;
#15786 = CARTESIAN_POINT ( 'NONE',  ( 768.0187753319979720, -152.6346026584200786, 318.0580252608186242 ) ) ;
#15787 = PRODUCT_DEFINITION_CONTEXT ( 'detailed design', #127, 'design' ) ;
#15788 = CARTESIAN_POINT ( 'NONE',  ( 814.8230680027162407, -317.8055962898684470, -333.7305795820267917 ) ) ;
#15789 = DIRECTION ( 'NONE',  ( 0.000000000000000000, 0.000000000000000000, 1.000000000000000000 ) ) ;
#15790 = VERTEX_POINT ( 'NONE', #32942 ) ;
#15791 = CARTESIAN_POINT ( 'NONE',  ( 797.8594530101008786, -349.5436935675102745, 322.1405469898980982 ) ) ;
#15792 = ORIENTED_EDGE ( 'NONE', *, *, #30587, .F. ) ;
#15793 = CARTESIAN_POINT ( 'NONE',  ( 767.6429770376289525, -177.1800572038744690, -306.8695393053162093 ) ) ;
#15794 = CARTESIAN_POINT ( 'NONE',  ( 805.0032342141413437, -85.54369356751118403, 314.9967657858572352 ) ) ;
#15795 = ORIENTED_EDGE ( 'NONE', *, *, #34190, .F. ) ;
#15796 = CARTESIAN_POINT ( 'NONE',  ( 774.6312213355098493, -167.3618753856927412, -364.6798772138717482 ) ) ;
#15797 = AXIS2_PLACEMENT_3D ( 'NONE', #9747, #21286, #24503 ) ;
#15798 = ORIENTED_EDGE ( 'NONE', *, *, #24975, .F. ) ;
#15799 = CARTESIAN_POINT ( 'NONE',  ( 790.0220218866281812, -415.0999726633340288, -363.2186876482849129 ) ) ;
#15800 = CARTESIAN_POINT ( 'NONE',  ( 754.9967657858570647, -241.5436935675106156, 365.0032342141425374 ) ) ;
#15801 = CARTESIAN_POINT ( 'NONE',  ( 757.2208543904082489, -160.7146871989598651, 350.9844846989624330 ) ) ;
#15804 = CARTESIAN_POINT ( 'NONE',  ( 811.6461892240364477, -412.7146871989590409, 324.1737431748509835 ) ) ;
#15803 = DIRECTION ( 'NONE',  ( 0.000000000000000000, 0.000000000000000000, -1.000000000000000000 ) ) ;
#15802 = CARTESIAN_POINT ( 'NONE',  ( -39.63011601220123481, -544.8427095258973623, -350.0000000000000000 ) ) ;
#15805 = ORIENTED_EDGE ( 'NONE', *, *, #26636, .T. ) ;
#15806 = CARTESIAN_POINT ( 'NONE',  ( 786.5483106153019435, -439.6454272087884760, -364.1601925771022366 ) ) ;
#15807 = CARTESIAN_POINT ( 'NONE',  ( 914.9999999999992042, 99.99999999999984368, 350.0000000000000000 ) ) ;
#15808 = CARTESIAN_POINT ( 'NONE',  ( 814.4686193811664907, -195.2817908451528410, -346.2056067578752732 ) ) ;
#15809 = CARTESIAN_POINT ( 'NONE',  ( 778.7629533639073998, -56.73633629969872771, 375.0009284576466371 ) ) ;
#15810 = VECTOR ( 'NONE', #22144, 1000.000000000000000 ) ;
#15812 = CARTESIAN_POINT ( 'NONE',  ( 755.0636971347428243, -172.2709662947836478, -341.7834795799807353 ) ) ;
#15811 = FACE_OUTER_BOUND ( 'NONE', #13161, .T. ) ;
#15813 = CARTESIAN_POINT ( 'NONE',  ( 754.8983024940795303, -378.8965053807772847, -336.9254006560228163 ) ) ;
#15814 = LINE ( 'NONE', #35939, #44638 ) ;
#15815 = CARTESIAN_POINT ( 'NONE',  ( 768.9521613784389729, -225.8272453906072599, -373.2346286133773106 ) ) ;
#15816 = CARTESIAN_POINT ( 'NONE',  ( 792.0613484971601110, -458.0032201311295807, 367.4685979341032294 ) ) ;
#15817 = CARTESIAN_POINT ( 'NONE',  ( 809.9999999999993179, -512.9681489794448908, -350.0000000000000000 ) ) ;
#15818 = CARTESIAN_POINT ( 'NONE',  ( 760.7433823573367135, -60.00906357242598688, -355.9930595647440441 ) ) ;
#15819 = CARTESIAN_POINT ( 'NONE',  ( 755.5913626894240451, -397.6454272087885329, 346.6156483768012890 ) ) ;
#15820 = VECTOR ( 'NONE', #26231, 1000.000000000000000 ) ;
#15821 = CARTESIAN_POINT ( 'NONE',  ( 810.7187646348534145, -258.4527844766016074, -356.7737145352016341 ) ) ;
#15822 = CARTESIAN_POINT ( 'NONE',  ( 939.9999999999993179, -414.5899773927343404, 210.0000000000000000 ) ) ;
#15823 = DIRECTION ( 'NONE',  ( 0.000000000000000000, 0.000000000000000000, 1.000000000000000000 ) ) ;
#15824 = CARTESIAN_POINT ( 'NONE',  ( 792.1044303154645831, -36.45278447660223975, -317.8323909638837677 ) ) ;
#15825 = CARTESIAN_POINT ( 'NONE',  ( 778.7629533639073998, -176.7363362996983369, 375.0009284576466371 ) ) ;
#15826 = CARTESIAN_POINT ( 'NONE',  ( 814.8230680027162407, -149.8055962898689870, -333.7305795820267917 ) ) ;
#15827 = CARTESIAN_POINT ( 'NONE',  ( 800.9747183278959710, -156.9982390220564241, 311.9810565676471583 ) ) ;
#15828 = CARTESIAN_POINT ( 'NONE',  ( 815.2698199232961542, -376.8164208402375834, -342.5225473063383106 ) ) ;
#15829 = DIRECTION ( 'NONE',  ( -1.000000000000000000, -0.000000000000000000, 0.000000000000000000 ) ) ;
#15830 = CARTESIAN_POINT ( 'NONE',  ( 801.9419747391806368, -258.4527844766016074, 351.9812246680014027 ) ) ;
#15831 =( GEOMETRIC_REPRESENTATION_CONTEXT ( 3 ) GLOBAL_UNCERTAINTY_ASSIGNED_CONTEXT ( ( #11200 ) ) GLOBAL_UNIT_ASSIGNED_CONTEXT ( ( #7908, #36065, #32827 ) ) REPRESENTATION_CONTEXT ( 'NONE', 'WORKASPACE' ) );
#15832 = CARTESIAN_POINT ( 'NONE',  ( 773.4516893846965786, -19.64542720878974791, 315.8398074228977066 ) ) ;
#15833 = CARTESIAN_POINT ( 'NONE',  ( 765.0180583372156207, -384.9982390220556567, -360.0135310231089534 ) ) ;
#15834 = AXIS2_PLACEMENT_3D ( 'NONE', #22025, #7713, #318 ) ;
#15835 = CARTESIAN_POINT ( 'NONE',  ( 355.8971257818259915, 290.0000000000001137, -244.9999999999999716 ) ) ;
#15836 = CARTESIAN_POINT ( 'NONE',  ( 757.7880784355613741, 5.990936427573807954, -312.4576283171834916 ) ) ;
#15837 = DIRECTION ( 'NONE',  ( 1.000000000000000000, 0.000000000000000000, 0.000000000000000000 ) ) ;
#15839 = CARTESIAN_POINT ( 'NONE',  ( 800.2193346964447755, -306.9982390220558273, 355.1360043628815788 ) ) ;
#15838 = CARTESIAN_POINT ( 'NONE',  ( 787.6308680596127942, -83.26014174441466764, 364.1105419155492768 ) ) ;
#15840 = ORIENTED_EDGE ( 'NONE', *, *, #17010, .F. ) ;
#15841 = CARTESIAN_POINT ( 'NONE',  ( 760.5453621957607311, -213.0783235625960401, -323.8424801807151425 ) ) ;
#15842 = CARTESIAN_POINT ( 'NONE',  ( 801.9419747391806368, -66.45278447660216159, 351.9812246680014027 ) ) ;
#15843 = CARTESIAN_POINT ( 'NONE',  ( 783.7566961878529810, -216.8965053807778816, -305.1792804349288417 ) ) ;
#15844 = LINE ( 'NONE', #2434, #4679 ) ;
#15845 = CARTESIAN_POINT ( 'NONE',  ( 766.5853460496234675, -349.9874144716865771, 372.3518521366060554 ) ) ;
#15846 = ORIENTED_EDGE ( 'NONE', *, *, #21942, .T. ) ;
#15847 = AXIS2_PLACEMENT_3D ( 'NONE', #22589, #1785, #2027 ) ;
#15848 = CARTESIAN_POINT ( 'NONE',  ( 815.0009284576459549, -438.3510508353226669, 338.7629533639073429 ) ) ;
#15849 = CARTESIAN_POINT ( 'NONE',  ( 756.5762568750052424, -363.1800572038739006, 348.7366044899774238 ) ) ;
#15850 = CIRCLE ( 'NONE', #39489, 7.999999999999896083 ) ;
#15851 = CARTESIAN_POINT ( 'NONE',  ( 805.0032342141412300, -61.54369356751124087, -314.9967657858571783 ) ) ;
#15852 = CIRCLE ( 'NONE', #41683, 8.024999999999948841 ) ;
#15853 = EDGE_CURVE ( 'NONE', #33957, #15534, #15387, .T. ) ;
#15854 = CARTESIAN_POINT ( 'NONE',  ( 771.1735550268780344, -81.18005720387482427, -316.3353852180828198 ) ) ;
#15855 = ORIENTED_EDGE ( 'NONE', *, *, #8274, .T. ) ;
#15856 = CARTESIAN_POINT ( 'NONE',  ( 754.7162404726377645, -14.73633629969885384, -339.4709603349214717 ) ) ;
#15857 = VERTEX_POINT ( 'NONE', #25079 ) ;
#15858 = CARTESIAN_POINT ( 'NONE',  ( 796.9571628226829034, -311.4636090269706870, -321.2382568024804641 ) ) ;
#15860 = CARTESIAN_POINT ( 'NONE',  ( 754.7162404726377645, -374.7363362996978253, 339.4709603349214717 ) ) ;
#15859 = CARTESIAN_POINT ( 'NONE',  ( 800.0135310231082713, -110.0891481129656597, 325.0180583372163028 ) ) ;
#15863 = CARTESIAN_POINT ( 'NONE',  ( 745.1769319972822814, -329.8055962898683902, 346.2694204179732083 ) ) ;
#15862 = DIRECTION ( 'NONE',  ( 1.000000000000000000, 4.625929269271485914E-16, 0.000000000000000000 ) ) ;
#15861 = CARTESIAN_POINT ( 'NONE',  ( 745.7998596910086917, -437.3618753856919170, 332.5602148656461168 ) ) ;
#15864 = VECTOR ( 'NONE', #2190, 1000.000000000000000 ) ;
#15865 = CARTESIAN_POINT ( 'NONE',  ( 768.8385539511368734, -95.26014174441461080, 306.4236121716840557 ) ) ;
#15866 = CARTESIAN_POINT ( 'NONE',  ( 786.5483106153019435, -319.6454272087888739, -364.1601925771022366 ) ) ;
#15867 = CARTESIAN_POINT ( 'NONE',  ( 781.8018195045266339, -334.2709662947829656, -365.1927285166406705 ) ) ;
#15868 = CARTESIAN_POINT ( 'NONE',  ( 804.9363028652555840, -136.2709662947837330, -338.2165204200192079 ) ) ;
#15869 = VECTOR ( 'NONE', #28630, 1000.000000000000000 ) ;
#15870 = CARTESIAN_POINT ( 'NONE',  ( 746.8695393053150156, -437.9073299311463074, 327.6429770376306010 ) ) ;
#15871 = VECTOR ( 'NONE', #6220, 1000.000000000000000 ) ;
#15873 = LINE ( 'NONE', #16563, #18959 ) ;
#15872 = DIRECTION ( 'NONE',  ( -0.000000000000000000, -4.857225732735055920E-15, 1.000000000000000000 ) ) ;
#15874 = CARTESIAN_POINT ( 'NONE',  ( 760.0363995740630116, -130.9181544815166660, -368.7758568127991907 ) ) ;
#15875 = DIRECTION ( 'NONE',  ( 0.000000000000000000, 1.000000000000000000, 0.000000000000000000 ) ) ;
#15876 = CARTESIAN_POINT ( 'NONE',  ( 928.0249999999991815, 219.9999999999998863, -360.0000000000000000 ) ) ;
#15877 = EDGE_CURVE ( 'NONE', #23028, #40984, #9015, .T. ) ;
#15878 = CARTESIAN_POINT ( 'NONE',  ( 784.1219089521767955, -309.2817908451525568, 315.0488828828318333 ) ) ;
#15879 = CARTESIAN_POINT ( 'NONE',  ( 802.1676090361156639, -182.6346026584199649, 327.8955696845344505 ) ) ;
#15880 = ORIENTED_EDGE ( 'NONE', *, *, #11926, .T. ) ;
#15881 = CARTESIAN_POINT ( 'NONE',  ( 760.0363995740630116, -274.9181544815161828, 368.7758568127991907 ) ) ;
#15882 = CARTESIAN_POINT ( 'NONE',  ( 745.4481719005789273, -147.7255117493291721, -347.5162901302853697 ) ) ;
#15883 = CARTESIAN_POINT ( 'NONE',  ( 799.9999999999993179, 205.0000000000000568, -360.0000000000000000 ) ) ;
#15884 = VECTOR ( 'NONE', #37076, 1000.000000000000114 ) ;
#15885 = CARTESIAN_POINT ( 'NONE',  ( 766.4474001241216001, -67.09997266333506616, 307.3154664389482491 ) ) ;
#15886 = CARTESIAN_POINT ( 'NONE',  ( 801.1904061080336987, -260.0891481129650060, -368.3070685750235498 ) ) ;
#15887 = EDGE_CURVE ( 'NONE', #31020, #29157, #36625, .T. ) ;
#15888 = VECTOR ( 'NONE', #23604, 1000.000000000000000 ) ;
#15889 = CARTESIAN_POINT ( 'NONE',  ( 746.8695393053151292, -437.9073299311464211, -327.6429770376306578 ) ) ;
#15890 = CARTESIAN_POINT ( 'NONE',  ( 785.3687786644884454, -155.3618753856927128, 315.3201227861279676 ) ) ;
#15891 = CARTESIAN_POINT ( 'NONE',  ( 773.7943932421234194, -335.8055962898683902, -305.5313806188329409 ) ) ;
#15892 = CARTESIAN_POINT ( 'NONE',  ( 796.9462024416508257, -84.45278447660206211, -308.9653473494370246 ) ) ;
#15893 = CARTESIAN_POINT ( 'NONE',  ( 755.1538015810308480, -14.19088175424431242, 343.0433043558613804 ) ) ;
#15894 = CARTESIAN_POINT ( 'NONE',  ( 772.4837098697144029, -359.3618753856920875, -374.5518280994205611 ) ) ;
#15895 = CARTESIAN_POINT ( 'NONE',  ( 1820.038553321469863, -589.9999999999998863, -201.9999999999998579 ) ) ;
#15896 = CARTESIAN_POINT ( 'NONE',  ( 769.1273215169530886, -382.7146871989591546, 317.4527132478988847 ) ) ;
#15897 = ORIENTED_EDGE ( 'NONE', *, *, #31160, .T. ) ;
#15898 = CARTESIAN_POINT ( 'NONE',  ( 786.2056067578752163, -131.8055962898690439, -374.4686193811670023 ) ) ;
#15899 = PLANE ( 'NONE',  #36598 ) ;
#15900 = CARTESIAN_POINT ( 'NONE',  ( 786.2056067578752163, -227.8055962898687596, 374.4686193811670023 ) ) ;
#15901 = CARTESIAN_POINT ( 'NONE',  ( 759.7806653035535192, -102.9982390220565662, 324.8639956371181370 ) ) ;
#15902 = VERTEX_POINT ( 'NONE', #43539 ) ;
#15903 = VECTOR ( 'NONE', #28295, 1000.000000000000000 ) ;
#15904 = EDGE_CURVE ( 'NONE', #20268, #18154, #4309, .T. ) ;
#15905 = CARTESIAN_POINT ( 'NONE',  ( 765.8855110935204493, 1.830767346494167391, -319.0159684113471599 ) ) ;
#15906 = CARTESIAN_POINT ( 'NONE',  ( 791.9812246680005501, -236.6346026584198228, 361.9419747391813189 ) ) ;
#15907 = CARTESIAN_POINT ( 'NONE',  ( 800.1688906516307043, -418.1692326535044799, -369.0717654672308186 ) ) ;
#15908 = DIRECTION ( 'NONE',  ( -0.000000000000000000, -0.6438296778008192334, 0.7651688349527135946 ) ) ;
#15909 = VERTEX_POINT ( 'NONE', #39193 ) ;
#15910 = ORIENTED_EDGE ( 'NONE', *, *, #35429, .T. ) ;
#15911 = CARTESIAN_POINT ( 'NONE',  ( 778.7629533639073998, -392.7363362996977116, -375.0009284576466371 ) ) ;
#15912 = VECTOR ( 'NONE', #8187, 1000.000000000000000 ) ;
#15913 =( BOUNDED_CURVE ( )  B_SPLINE_CURVE ( 3, ( #22302, #19922, #13453, #34465 ),
 .UNSPECIFIED., .F., .T. ) 
 B_SPLINE_CURVE_WITH_KNOTS ( ( 4, 4 ),
 ( 4.712388980384689674, 6.283185307179586232 ),
 .UNSPECIFIED. ) 
 CURVE ( )  GEOMETRIC_REPRESENTATION_ITEM ( )  RATIONAL_B_SPLINE_CURVE ( ( 1.000000000000000000, 0.8047378541243649375, 0.8047378541243649375, 1.000000000000000000 ) ) 
 REPRESENTATION_ITEM ( '' )  );
#15914 = CARTESIAN_POINT ( 'NONE',  ( 771.2633955100217236, -239.9073299311470748, -363.4237431249939618 ) ) ;
#15915 = AXIS2_PLACEMENT_3D ( 'NONE', #4736, #5633, #30338 ) ;
#15916 = CARTESIAN_POINT ( 'NONE',  ( 792.3570229623691148, -333.1800572038740142, 373.1304606946836770 ) ) ;
#15917 = CARTESIAN_POINT ( 'NONE',  ( 759.8311093483677041, -46.16923265350568784, 310.9282345327691814 ) ) ;
#15918 = CARTESIAN_POINT ( 'NONE',  ( 758.4439275373578084, -228.5545181178799794, -353.2243759319684386 ) ) ;
#15919 = CARTESIAN_POINT ( 'NONE',  ( 804.6798772138708955, -231.7255117493288310, -334.6312213355107019 ) ) ;
#15920 = CARTESIAN_POINT ( 'NONE',  ( 756.3353852180820240, -389.9073299311465917, -331.1735550268787733 ) ) ;
#15921 = ORIENTED_EDGE ( 'NONE', *, *, #6544, .T. ) ;
#15922 = CARTESIAN_POINT ( 'NONE',  ( 759.9864689768902508, -218.0891481129653187, 354.9819416627836404 ) ) ;
#15923 = CARTESIAN_POINT ( 'NONE',  ( 803.6646147819161570, -89.90732993114750116, -348.8264449731210561 ) ) ;
#15924 = ORIENTED_EDGE ( 'NONE', *, *, #16239, .F. ) ;
#15925 = CARTESIAN_POINT ( 'NONE',  ( 787.5162901302840055, -323.3618753856923149, 305.4481719005792684 ) ) ;
#15926 = EDGE_CURVE ( 'NONE', #34816, #7814, #8010, .T. ) ;
#15927 = CYLINDRICAL_SURFACE ( 'NONE', #41779, 9.999999999999982236 ) ;
#15928 = DIRECTION ( 'NONE',  ( -0.000000000000000000, -0.000000000000000000, 1.000000000000000000 ) ) ;
#15929 = CARTESIAN_POINT ( 'NONE',  ( 787.4999999999992042, -512.9681489794448908, 339.9999999999999432 ) ) ;
#15930 = EDGE_CURVE ( 'NONE', #1390, #43251, #909, .T. ) ;
#15931 = CARTESIAN_POINT ( 'NONE',  ( 801.5560724626406000, -192.5545181178801215, 326.7756240680316182 ) ) ;
#15932 = CARTESIAN_POINT ( 'NONE',  ( 765.0180583372156207, -96.99823902205660886, 360.0135310231089534 ) ) ;
#15933 = ORIENTED_EDGE ( 'NONE', *, *, #36268, .F. ) ;
#15934 = CARTESIAN_POINT ( 'NONE',  ( 804.1009440267234822, -431.4636090269702322, -314.0944755984392600 ) ) ;
#15935 = CARTESIAN_POINT ( 'NONE',  ( 782.5225473063383106, -46.27096629478403855, -375.2698199232970637 ) ) ;
#15936 = CARTESIAN_POINT ( 'NONE',  ( 787.6308680596127942, -251.2601417444141134, 364.1105419155492768 ) ) ;
#15937 = AXIS2_PLACEMENT_3D ( 'NONE', #15375, #15585, #29667 ) ;
#15938 = CARTESIAN_POINT ( 'NONE',  ( 781.8018195045266339, -382.2709662947828519, -365.1927285166406705 ) ) ;
#15939 = CARTESIAN_POINT ( 'NONE',  ( 774.6312213355098493, -23.36187538569319244, -364.6798772138717482 ) ) ;
#15940 = CARTESIAN_POINT ( 'NONE',  ( 808.0189434323515343, -422.0891481129647218, 319.0252816721025511 ) ) ;
#15941 = CARTESIAN_POINT ( 'NONE',  ( -37.63011601220122770, -544.8427095258973623, -350.0000000000000000 ) ) ;
#15942 = VECTOR ( 'NONE', #14184, 1000.000000000000000 ) ;
#15943 = CARTESIAN_POINT ( 'NONE',  ( 755.5913626894240451, -301.6454272087889308, -346.6156483768012890 ) ) ;
#15944 = ADVANCED_FACE ( 'NONE', ( #42866 ), #11906, .T. ) ;
#15945 = CARTESIAN_POINT ( 'NONE',  ( 751.6929314249748586, -174.9982390220563673, -318.8095938919659034 ) ) ;
#15946 = EDGE_CURVE ( 'NONE', #34100, #20728, #18601, .T. ) ;
#15947 = CARTESIAN_POINT ( 'NONE',  ( 792.2312462859673587, -59.90732993114762905, 307.2067596250082602 ) ) ;
#15948 = CARTESIAN_POINT ( 'NONE',  ( 745.7998596910086917, -149.3618753856928265, 332.5602148656461168 ) ) ;
#15949 = CARTESIAN_POINT ( 'NONE',  ( 793.3891180349545493, 16.45630643248849978, -314.6660875939051607 ) ) ;
#15950 = CARTESIAN_POINT ( 'NONE',  ( 919.9999999999993179, 219.9999999999998863, 360.0000000000000000 ) ) ;
#15951 = AXIS2_PLACEMENT_3D ( 'NONE', #1134, #8297, #39954 ) ;
#15952 = CARTESIAN_POINT ( 'NONE',  ( -338.8365100919713200, 260.0000000000001137, -191.9749999999917804 ) ) ;
#15953 = CARTESIAN_POINT ( 'NONE',  ( 745.0891759886404770, -364.2709662947830793, 342.4968714119734159 ) ) ;
#15954 = CARTESIAN_POINT ( 'NONE',  ( 771.1735550268778070, -345.1800572038739006, -316.3353852180827630 ) ) ;
#15955 = CARTESIAN_POINT ( 'NONE',  ( 769.1273215169530886, 1.285312801039623753, 317.4527132478988847 ) ) ;
#15956 = CARTESIAN_POINT ( 'NONE',  ( 799.9636004259356241, -94.91815448151677970, -311.2241431872006956 ) ) ;
#15957 = CARTESIAN_POINT ( 'NONE',  ( 800.7704444035546203, -124.1692326535054463, -326.0291762391768771 ) ) ;
#15958 = ADVANCED_FACE ( 'NONE', ( #43096 ), #11462, .F. ) ;
#15959 = CARTESIAN_POINT ( 'NONE',  ( 811.6461892240364477, -148.7146871989598935, 324.1737431748509835 ) ) ;
#15960 = CARTESIAN_POINT ( 'NONE',  ( 767.8955696845334842, -0.4527844766023629286, 362.1676090361161755 ) ) ;
#15961 = ADVANCED_FACE ( 'NONE', ( #43327, #39880 ), #32252, .F. ) ;
#15962 = CARTESIAN_POINT ( 'NONE',  ( 788.7631598425961101, -169.4419599262325562, 305.7194118038759143 ) ) ;
#15963 = CARTESIAN_POINT ( 'NONE',  ( 785.3687786644884454, -35.36187538569316047, -315.3201227861279676 ) ) ;
#15964 = CARTESIAN_POINT ( 'NONE',  ( 801.3366627262608972, -128.5328690171417634, -353.0897708529566899 ) ) ;
#15965 = CARTESIAN_POINT ( 'NONE',  ( 805.1927285166397041, -136.8164208402382371, -341.8018195045277707 ) ) ;
#15966 = CARTESIAN_POINT ( 'NONE',  ( 801.9419747391806368, -138.4527844766019200, 351.9812246680014027 ) ) ;
#15967 = CARTESIAN_POINT ( 'NONE',  ( 798.0661480581538854, 21.46713098285774279, -309.5768839229118043 ) ) ;
#15968 = CARTESIAN_POINT ( 'NONE',  ( 762.3223304703356007, -271.5436935675106156, 322.3223304703362828 ) ) ;
#15969 = FACE_OUTER_BOUND ( 'NONE', #22160, .T. ) ;
#15970 = ORIENTED_EDGE ( 'NONE', *, *, #26611, .F. ) ;
#15971 = CARTESIAN_POINT ( 'NONE',  ( 763.2154366446407039, 2.376221891948710585, 321.4292242960311228 ) ) ;
#15973 = AXIS2_PLACEMENT_3D ( 'NONE', #26377, #16206, #4681 ) ;
#15972 = CARTESIAN_POINT ( 'NONE',  ( 795.8262568251477660, -286.3726999360617356, -308.3538107759623585 ) ) ;
#15974 = ORIENTED_EDGE ( 'NONE', *, *, #23535, .F. ) ;
#15975 = VECTOR ( 'NONE', #31264, 1000.000000000000000 ) ;
#15976 = CARTESIAN_POINT ( 'NONE',  ( 814.9108240113580450, -232.2709662947834488, 337.5031285880265273 ) ) ;
#15977 = CARTESIAN_POINT ( 'NONE',  ( 799.2566176426618085, -312.0090635724251911, 324.0069404352559559 ) ) ;
#15978 = CARTESIAN_POINT ( 'NONE',  ( 755.0488828828309806, -401.8055962898681059, 344.1219089521771934 ) ) ;
#15979 = ORIENTED_EDGE ( 'NONE', *, *, #10888, .T. ) ;
#15981 = VECTOR ( 'NONE', #42915, 1000.000000000000000 ) ;
#15980 = CARTESIAN_POINT ( 'NONE',  ( 780.5236548040995785, -116.7363362996985217, -314.9735926884559944 ) ) ;
#15982 = CARTESIAN_POINT ( 'NONE',  ( 797.6776695296629214, -115.5436935675110988, -357.6776695296636603 ) ) ;
#15983 = CARTESIAN_POINT ( 'NONE',  ( 758.0580252608178853, -294.4527844766013800, -328.0187753319985404 ) ) ;
#15984 = EDGE_CURVE ( 'NONE', #9272, #30100, #38501, .T. ) ;
#15985 = ORIENTED_EDGE ( 'NONE', *, *, #25000, .F. ) ;
#15986 = CARTESIAN_POINT ( 'NONE',  ( 781.7834795799800531, -418.8164208402374129, -315.0636971347436202 ) ) ;
#15987 = CARTESIAN_POINT ( 'NONE',  ( 762.3223304703356007, -79.54369356751119824, -322.3223304703362828 ) ) ;
#15988 = AXIS2_PLACEMENT_3D ( 'NONE', #925, #38843, #3945 ) ;
#15989 = EDGE_CURVE ( 'NONE', #38523, #41960, #20190, .T. ) ;
#15990 = CARTESIAN_POINT ( 'NONE',  ( 780.5290396650775619, -300.3510508353230080, 365.2837595273619513 ) ) ;
#15991 = CARTESIAN_POINT ( 'NONE',  ( 998.9999999999992042, 249.9999999999998863, -199.9999999999999716 ) ) ;
#15992 = DIRECTION ( 'NONE',  ( -1.000000000000000000, 0.000000000000000000, 0.000000000000000000 ) ) ;
#15993 = EDGE_CURVE ( 'NONE', #39863, #12219, #1950, .T. ) ;
#15994 = DIRECTION ( 'NONE',  ( -1.000000000000000000, -0.000000000000000000, -0.000000000000000000 ) ) ;
#15995 = ORIENTED_EDGE ( 'NONE', *, *, #7399, .T. ) ;
#15996 = CARTESIAN_POINT ( 'NONE',  ( 799.9636004259356241, -358.9181544815160123, -311.2241431872006956 ) ) ;
#15997 = CARTESIAN_POINT ( 'NONE',  ( 813.5763878283155464, -195.8272453906074304, 351.1614460488615350 ) ) ;
#15999 = CARTESIAN_POINT ( 'NONE',  ( 756.3353852180819104, -293.9073299311468759, -331.1735550268788302 ) ) ;
#15998 = DIRECTION ( 'NONE',  ( 8.659560562354807133E-17, 0.7071067811865578978, -0.7071067811865372477 ) ) ;
#16000 = CARTESIAN_POINT ( 'NONE',  ( 779.4763451958990572, -200.7363362996982801, -365.0264073115438919 ) ) ;
#16001 = CARTESIAN_POINT ( 'NONE',  ( 755.2512626584698410, -31.54369356751135456, 315.2512626584710915 ) ) ;
#16002 = LINE ( 'NONE', #1664, #43957 ) ;
#16003 = CARTESIAN_POINT ( 'NONE',  ( 811.0346526505617248, -398.6346026584193396, -323.0537975583478101 ) ) ;
#16004 = CARTESIAN_POINT ( 'NONE',  ( 914.9999999999992042, 74.99999999999984368, 350.0000000000000000 ) ) ;
#16005 = CARTESIAN_POINT ( 'NONE',  ( 756.5762568750052424, -51.18005720387493085, 348.7366044899774238 ) ) ;
#16006 = AXIS2_PLACEMENT_3D ( 'NONE', #21229, #21453, #28152 ) ;
#16007 = CARTESIAN_POINT ( 'NONE',  ( 766.4474001241216001, -307.0999726633343130, 307.3154664389482491 ) ) ;
#16008 = CARTESIAN_POINT ( 'NONE',  ( 751.9810565676468741, -242.0891481129652618, 360.9747183278973921 ) ) ;
#16009 = CARTESIAN_POINT ( 'NONE',  ( 745.7998596910086917, -29.36187538569318178, -332.5602148656461168 ) ) ;
#16010 = AXIS2_PLACEMENT_3D ( 'NONE', #9406, #37349, #40814 ) ;
#16011 = FACE_BOUND ( 'NONE', #11614, .T. ) ;
#16012 = CARTESIAN_POINT ( 'NONE',  ( -786.4999999999993179, 22.32581219114657856, 895.6886905569881492 ) ) ;
#16013 = CARTESIAN_POINT ( 'NONE',  ( 759.9864689768902508, -362.0891481129648923, 354.9819416627836404 ) ) ;
#16014 = CARTESIAN_POINT ( 'NONE',  ( 790.0220218866281812, -127.0999726633348672, 363.2186876482849129 ) ) ;
#16015 = CARTESIAN_POINT ( 'NONE',  ( 754.9735926884551418, -18.35105083532395298, -340.5236548041000333 ) ) ;
#16016 = CARTESIAN_POINT ( 'NONE',  ( 187.1337867209877857, -434.4637272565419153, -347.3621835540870961 ) ) ;
#16017 = DIRECTION ( 'NONE',  ( 1.000000000000000000, -0.000000000000000000, -0.000000000000000000 ) ) ;
#16018 = CARTESIAN_POINT ( 'NONE',  ( 776.2433038121456548, -132.8965053807781374, 374.8207195650711014 ) ) ;
#16019 = CARTESIAN_POINT ( 'NONE',  ( 757.8323909638827445, -410.6346026584191122, 352.1044303154654358 ) ) ;
#16020 = VERTEX_POINT ( 'NONE', #12580 ) ;
#16021 = CARTESIAN_POINT ( 'NONE',  ( 804.4286716492782716, -41.36187538569314626, -345.3141322388244703 ) ) ;
#16022 = CARTESIAN_POINT ( 'NONE',  ( 765.8855110935204493, -334.1692326535047073, -319.0159684113471599 ) ) ;
#16024 = CARTESIAN_POINT ( 'NONE',  ( 774.6858677611749044, -153.7255117493291721, 315.5713283507209894 ) ) ;
#16023 = CARTESIAN_POINT ( 'NONE',  ( 755.0636971347428243, -172.2709662947836478, 341.7834795799807353 ) ) ;
#16025 = CARTESIAN_POINT ( 'NONE',  ( 813.2346286133761168, -341.2601417444138292, -328.9521613784389160 ) ) ;
#16026 = DIRECTION ( 'NONE',  ( 1.000000000000000000, 0.000000000000000000, 0.000000000000000000 ) ) ;
#16027 = ORIENTED_EDGE ( 'NONE', *, *, #30039, .T. ) ;
#16028 = CARTESIAN_POINT ( 'NONE',  ( 803.6646147819161570, -353.9073299311467053, 348.8264449731210561 ) ) ;
#16029 = ORIENTED_EDGE ( 'NONE', *, *, #6076, .F. ) ;
#16030 = CARTESIAN_POINT ( 'NONE',  ( 759.0252816721024374, -192.9982390220562820, -368.0189434323527280 ) ) ;
#16031 = CARTESIAN_POINT ( 'NONE',  ( 749.2812353651451076, -102.4527844766020337, 323.2262854647983090 ) ) ;
#16032 = VERTEX_POINT ( 'NONE', #1712 ) ;
#16033 = CARTESIAN_POINT ( 'NONE',  ( 801.9419747391806368, -186.4527844766017779, -351.9812246680014027 ) ) ;
#16034 = EDGE_LOOP ( 'NONE', ( #37277, #37442, #34185, #15326 ) ) ;
#16035 = CARTESIAN_POINT ( 'NONE',  ( 761.4292242960306112, -449.4636090269702322, -323.2154366446414429 ) ) ;
#16036 = CARTESIAN_POINT ( 'NONE',  ( 763.2262854647970016, -248.6346026584197659, 309.2812353651462445 ) ) ;
#16037 = CARTESIAN_POINT ( 'NONE',  ( 801.3366627262608972, -176.5328690171416213, 353.0897708529566899 ) ) ;
#16039 = CARTESIAN_POINT ( 'NONE',  ( 831.1634899080286232, 256.4999999999998863, -193.8809999999999718 ) ) ;
#16038 = CARTESIAN_POINT ( 'NONE',  ( -78.83651009197140525, 240.0000000000000853, -202.7499999999934346 ) ) ;
#16040 = VERTEX_POINT ( 'NONE', #22958 ) ;
#16041 = APPLICATION_CONTEXT ( 'automotive_design' ) ;
#16042 = CARTESIAN_POINT ( 'NONE',  ( 793.0897708529556667, -414.5545181178795247, -361.3366627262616362 ) ) ;
#16043 = DIRECTION ( 'NONE',  ( -1.000000000000000000, -1.644774851296528363E-16, -0.000000000000000000 ) ) ;
#16044 = CARTESIAN_POINT ( 'NONE',  ( 788.6739635108323228, -223.6454272087891013, -373.9316612368139090 ) ) ;
#16045 = CARTESIAN_POINT ( 'NONE',  ( 745.1792804349281596, -110.1908817542440033, 343.7566961878542884 ) ) ;
#16046 = CIRCLE ( 'NONE', #35971, 10.00000000000000888 ) ;
#16048 = CARTESIAN_POINT ( 'NONE',  ( 756.3353852180819104, -173.9073299311472169, -331.1735550268788302 ) ) ;
#16047 = CARTESIAN_POINT ( 'NONE',  ( 829.9999999999992042, 529.9999999999997726, -360.0000000000000000 ) ) ;
#16049 = CARTESIAN_POINT ( 'NONE',  ( 805.0264073115434940, -366.3510508353228374, -339.4763451958999099 ) ) ;
#16050 = LINE ( 'NONE', #24493, #36530 ) ;
#16051 = CARTESIAN_POINT ( 'NONE',  ( 749.5768839229115201, -228.5545181178799794, -358.0661480581553064 ) ) ;
#16052 = DIRECTION ( 'NONE',  ( 1.000000000000000000, 0.000000000000000000, 0.000000000000000000 ) ) ;
#16053 = CARTESIAN_POINT ( 'NONE',  ( -115.7583438952258774, -600.0000000000000000, -244.9999999999999716 ) ) ;
#16054 = CARTESIAN_POINT ( 'NONE',  ( 775.8780910478218402, -33.28179084515333130, -364.9511171171680530 ) ) ;
#16055 = CARTESIAN_POINT ( 'NONE',  ( 763.0428371773158460, -443.4636090269702322, 358.7617431975195359 ) ) ;
#16056 = CARTESIAN_POINT ( 'NONE',  ( 800.9747183278959710, -252.9982390220560831, -311.9810565676471583 ) ) ;
#16057 = CARTESIAN_POINT ( 'NONE',  ( 790.0220218866281812, -247.0999726633344835, 363.2186876482849129 ) ) ;
#16058 = DIRECTION ( 'NONE',  ( 0.000000000000000000, 0.000000000000000000, -1.000000000000000000 ) ) ;
#16059 = DIRECTION ( 'NONE',  ( 0.000000000000000000, 0.000000000000000000, 1.000000000000000000 ) ) ;
#16060 = CARTESIAN_POINT ( 'NONE',  ( 781.7834795799800531, -58.81642084023854267, -315.0636971347436202 ) ) ;
#16061 = CARTESIAN_POINT ( 'NONE',  ( 781.2370466360911223, -164.7363362996983938, 304.9990715423533629 ) ) ;
#16062 = CARTESIAN_POINT ( 'NONE',  ( 748.3538107759620743, -136.7146871989600072, -355.8262568251490165 ) ) ;
#16063 = CARTESIAN_POINT ( 'NONE',  ( 801.1904061080336987, -164.0891481129655176, 368.3070685750235498 ) ) ;
#16064 = CARTESIAN_POINT ( 'NONE',  ( 792.3570229623688874, -381.1800572038737869, -373.1304606946836202 ) ) ;
#16065 = CARTESIAN_POINT ( 'NONE',  ( 311.1634899080286232, 256.5000000000000000, -199.9999999999963336 ) ) ;
#16066 = CARTESIAN_POINT ( 'NONE',  ( 781.8018195045266339, -238.2709662947833920, 365.1927285166406705 ) ) ;
#16067 = CARTESIAN_POINT ( 'NONE',  ( 755.8894580844503253, -39.82724539060786384, 332.3691319403863531 ) ) ;
#16068 = CARTESIAN_POINT ( 'NONE',  ( 778.2165204200184689, -406.8164208402375266, -364.9363028652563230 ) ) ;
#16069 = FACE_OUTER_BOUND ( 'NONE', #30193, .T. ) ;
#16070 = CARTESIAN_POINT ( 'NONE',  ( 754.3581564841646241, 6.536390973028352924, -316.1443688327762516 ) ) ;
#16071 = CARTESIAN_POINT ( 'NONE',  ( 521.6730038022808458, 199.9999999999999147, -122.7905160835442615 ) ) ;
#16072 = CARTESIAN_POINT ( 'NONE',  ( 786.6156483768007774, -73.44195992623286884, 315.5913626894246136 ) ) ;
#16073 = EDGE_LOOP ( 'NONE', ( #44536, #19765, #44906, #31596 ) ) ;
#16074 = CARTESIAN_POINT ( 'NONE',  ( 790.8726784830453198, -226.7146871989596661, -362.5472867521010585 ) ) ;
#16075 = CARTESIAN_POINT ( 'NONE',  ( 765.0180583372156207, -48.99823902205675807, 360.0135310231089534 ) ) ;
#16076 = CARTESIAN_POINT ( 'NONE',  ( 778.7502325331095108, -216.3510508353233490, -304.6391490659818828 ) ) ;
#16077 = DIRECTION ( 'NONE',  ( -1.000000000000000000, 0.000000000000000000, -0.000000000000000000 ) ) ;
#16078 = CARTESIAN_POINT ( 'NONE',  ( 813.2346286133761168, -389.2601417444136018, 328.9521613784389160 ) ) ;
#16079 = ORIENTED_EDGE ( 'NONE', *, *, #32297, .T. ) ;
#16080 = AXIS2_PLACEMENT_3D ( 'NONE', #11610, #4662, #17850 ) ;
#16081 = CARTESIAN_POINT ( 'NONE',  ( 748.9653473494363425, -2.634602658420536869, 356.9462024416521331 ) ) ;
#16082 = CARTESIAN_POINT ( 'NONE',  ( 805.1927285166397041, -184.8164208402380950, -341.8018195045277707 ) ) ;
#16083 = CARTESIAN_POINT ( 'NONE',  ( 797.6776695296629214, -379.5436935675102745, 357.6776695296636603 ) ) ;
#16084 = CARTESIAN_POINT ( 'NONE',  ( 808.3070685750230950, -66.99823902205672255, -361.1904061080339261 ) ) ;
#16085 = CARTESIAN_POINT ( 'NONE',  ( 767.8955696845334842, -72.45278447660213317, -362.1676090361161755 ) ) ;
#16086 = EDGE_LOOP ( 'NONE', ( #8871, #42059, #21319, #33035 ) ) ;
#16087 = CARTESIAN_POINT ( 'NONE',  ( 790.9844846989617508, 1.627300063937458408, -317.2208543904092721 ) ) ;
#16088 = ORIENTED_EDGE ( 'NONE', *, *, #6335, .F. ) ;
#16089 = CARTESIAN_POINT ( 'NONE',  ( 800.9840315886518738, -364.9181544815158986, -354.1144889064786412 ) ) ;
#16091 = CARTESIAN_POINT ( 'NONE',  ( 757.0176451133909268, -397.0999726633340288, 349.9200121543848354 ) ) ;
#16090 = CARTESIAN_POINT ( 'NONE',  ( 803.4237431249931660, -87.18005720387481006, 331.2633955100225194 ) ) ;
#16094 = CARTESIAN_POINT ( 'NONE',  ( 766.5853460496234675, -325.9874144716865771, 372.3518521366060554 ) ) ;
#16093 = LINE ( 'NONE', #2224, #12220 ) ;
#16092 = CARTESIAN_POINT ( 'NONE',  ( 759.0252816721024374, -432.9982390220555999, 368.0189434323527280 ) ) ;
#16095 = CARTESIAN_POINT ( 'NONE',  ( 744.9990715423526808, -90.35105083532373271, 341.2370466360926002 ) ) ;
#16096 = CARTESIAN_POINT ( 'NONE',  ( 802.9823548866075953, -337.0999726633342561, -330.0799878456151077 ) ) ;
#16097 = CARTESIAN_POINT ( 'NONE',  ( 797.6776695296629214, -307.5436935675104451, -357.6776695296636603 ) ) ;
#16098 = CARTESIAN_POINT ( 'NONE',  ( 788.8264449731200330, -165.1800572038745258, -363.6646147819171233 ) ) ;
#16099 = EDGE_CURVE ( 'NONE', #20290, #12560, #40753, .T. ) ;
#16100 = CARTESIAN_POINT ( 'NONE',  ( 745.5313806188320314, -15.28179084515340058, 333.7943932421247268 ) ) ;
#16102 = FACE_OUTER_BOUND ( 'NONE', #40860, .T. ) ;
#16101 = DIRECTION ( 'NONE',  ( 0.000000000000000000, 0.000000000000000000, 1.000000000000000000 ) ) ;
#16103 = CARTESIAN_POINT ( 'NONE',  ( 780.5290396650775619, -276.3510508353231785, -365.2837595273619513 ) ) ;
#16104 = CARTESIAN_POINT ( 'NONE',  ( 764.1737431748507561, -130.3726999360621619, -371.6461892240376415 ) ) ;
#16105 = LINE ( 'NONE', #2008, #9386 ) ;
#16106 = CARTESIAN_POINT ( 'NONE',  ( -769.9999999999992042, 240.0000000000000568, -319.9999999999999432 ) ) ;
#16107 = CARTESIAN_POINT ( 'NONE',  ( 755.3028492785439312, -327.2817908451525000, 335.9200461376539693 ) ) ;
#16108 = CARTESIAN_POINT ( 'NONE',  ( 794.9819416627830151, -180.9982390220563389, 319.9864689768909898 ) ) ;
#16109 = ORIENTED_EDGE ( 'NONE', *, *, #29187, .F. ) ;
#16110 = CARTESIAN_POINT ( 'NONE',  ( 814.5518280994195948, -135.7255117493291721, -332.4837098697145166 ) ) ;
#16111 = VECTOR ( 'NONE', #21253, 1000.000000000000114 ) ;
#16112 = CARTESIAN_POINT ( 'NONE',  ( 762.1177392798416577, -90.55451811788041994, 309.8865473780659272 ) ) ;
#16113 = CARTESIAN_POINT ( 'NONE',  ( 745.4481719005789273, -267.7255117493286320, -347.5162901302853129 ) ) ;
#16114 = CARTESIAN_POINT ( 'NONE',  ( -728.8365100919714905, 260.0000000000001705, -199.9999999999890861 ) ) ;
#16115 = CARTESIAN_POINT ( 'NONE',  ( 781.8018195045266339, -166.2709662947835909, 365.1927285166406705 ) ) ;
#16116 = EDGE_LOOP ( 'NONE', ( #44247, #16135, #24932, #41671 ) ) ;
#16117 = CARTESIAN_POINT ( 'NONE',  ( 746.0683387631852383, -331.4419599262320162, -331.3260364891676204 ) ) ;
#16118 = CARTESIAN_POINT ( 'NONE',  ( 782.5225473063381969, -94.27096629478386092, -375.2698199232970637 ) ) ;
#16119 = CARTESIAN_POINT ( 'NONE',  ( 802.5472867521000353, -28.37269993606244967, 350.8726784830461156 ) ) ;
#16120 = CARTESIAN_POINT ( 'NONE',  ( 749.2812353651451076, -366.4527844766012095, -323.2262854647983090 ) ) ;
#16121 = DIRECTION ( 'NONE',  ( 0.000000000000000000, 0.000000000000000000, 1.000000000000000000 ) ) ;
#16122 = CARTESIAN_POINT ( 'NONE',  ( 761.2382568024794409, -423.6237781080499190, 356.9571628226838129 ) ) ;
#16123 = EDGE_LOOP ( 'NONE', ( #40980, #1269, #42885, #43298 ) ) ;
#16124 = CARTESIAN_POINT ( 'NONE',  ( 769.1273215169530886, -70.71468719896014932, 317.4527132478988847 ) ) ;
#16125 = CARTESIAN_POINT ( 'NONE',  ( 773.7943932421234194, -119.8055962898690865, -305.5313806188329409 ) ) ;
#16126 = CARTESIAN_POINT ( 'NONE',  ( -858.8365100919713768, 260.0000000000002274, -206.1189999999881479 ) ) ;
#16127 = CARTESIAN_POINT ( 'NONE',  ( 773.7943932421234194, -287.8055962898685038, 305.5313806188329409 ) ) ;
#16128 = CARTESIAN_POINT ( 'NONE',  ( 781.8018195045267476, -70.27096629478397460, 365.1927285166407273 ) ) ;
#16129 = ORIENTED_EDGE ( 'NONE', *, *, #24162, .T. ) ;
#16130 = CARTESIAN_POINT ( 'NONE',  ( 769.1273215169530886, 1.285312801039623753, -317.4527132478988847 ) ) ;
#16131 = CARTESIAN_POINT ( 'NONE',  ( 795.1360043628807261, -260.0891481129650060, 360.2193346964456282 ) ) ;
#16132 = CARTESIAN_POINT ( 'NONE',  ( 801.9858362298568863, -435.0783235625953580, -312.7379699480935642 ) ) ;
#16133 = CARTESIAN_POINT ( 'NONE',  ( 759.9999999999992042, 205.0000000000000568, 329.9999999999999432 ) ) ;
#16134 = EDGE_LOOP ( 'NONE', ( #32096, #16837, #12621, #19213 ) ) ;
#16135 = ORIENTED_EDGE ( 'NONE', *, *, #17396, .T. ) ;
#16136 = CARTESIAN_POINT ( 'NONE',  ( 773.7305795820266212, -393.2817908451522726, -374.8230680027170365 ) ) ;
#16137 = AXIS2_PLACEMENT_3D ( 'NONE', #24049, #28206, #9979 ) ;
#16138 = CARTESIAN_POINT ( 'NONE',  ( 755.3201227861273992, -243.7255117493287742, -345.3687786644892981 ) ) ;
#16139 = EDGE_CURVE ( 'NONE', #42387, #37811, #9112, .T. ) ;
#16141 = CARTESIAN_POINT ( 'NONE',  ( 761.9338519418445230, -206.5328690171415360, 370.4231160770881957 ) ) ;
#16140 = CARTESIAN_POINT ( 'NONE',  ( 745.7998596910086917, -317.3618753856922581, 332.5602148656461168 ) ) ;
#16142 = CARTESIAN_POINT ( 'NONE',  ( 776.2433038121456548, -36.89650538077844288, 374.8207195650711014 ) ) ;
#16143 = CARTESIAN_POINT ( 'NONE',  ( 769.0155153010367712, -226.3726999360617924, -362.7791456095907279 ) ) ;
#16144 = CARTESIAN_POINT ( 'NONE',  ( 794.9819416627830151, -228.9982390220561683, -319.9864689768909898 ) ) ;
#16145 = CARTESIAN_POINT ( 'NONE',  ( 788.7366044899766848, -419.9073299311465348, -316.5762568750059813 ) ) ;
#16146 = ORIENTED_EDGE ( 'NONE', *, *, #9445, .T. ) ;
#16147 = CARTESIAN_POINT ( 'NONE',  ( 797.6776695296629214, -211.5436935675107861, 357.6776695296636603 ) ) ;
#16148 = CARTESIAN_POINT ( 'NONE',  ( 781.8018195045266339, -94.27096629478386092, -365.1927285166406705 ) ) ;
#16149 = ORIENTED_EDGE ( 'NONE', *, *, #30641, .T. ) ;
#16150 = CARTESIAN_POINT ( 'NONE',  ( 792.2312462859673587, -371.9073299311465917, 307.2067596250082602 ) ) ;
#16151 = DIRECTION ( 'NONE',  ( -0.000000000000000000, 1.000000000000000000, -0.000000000000000000 ) ) ;
#16152 = FACE_OUTER_BOUND ( 'NONE', #14649, .T. ) ;
#16153 = FACE_OUTER_BOUND ( 'NONE', #3083, .T. ) ;
#16154 = CARTESIAN_POINT ( 'NONE',  ( 760.7433823573367135, -180.0090635724255890, 355.9930595647440441 ) ) ;
#16155 = CARTESIAN_POINT ( 'NONE',  ( 797.6776695296629214, -67.54369356751125508, 357.6776695296636603 ) ) ;
#16156 = ORIENTED_EDGE ( 'NONE', *, *, #10295, .T. ) ;
#16157 = CARTESIAN_POINT ( 'NONE',  ( 750.9282345327678740, -448.9181544815156144, -319.8311093483690115 ) ) ;
#16158 = CARTESIAN_POINT ( 'NONE',  ( 758.8095938919644823, -32.08914811296589420, -311.6929314249762797 ) ) ;
#16159 = CARTESIAN_POINT ( 'NONE',  ( 796.7845633553578182, -249.6237781080505158, 358.5707757039688204 ) ) ;
#16160 = CARTESIAN_POINT ( 'NONE',  ( 801.9419747391806368, -402.4527844766010389, -351.9812246680014027 ) ) ;
#16161 = CARTESIAN_POINT ( 'NONE',  ( 800.2193346964446619, -18.99823902205684689, -355.1360043628816925 ) ) ;
#16162 = CARTESIAN_POINT ( 'NONE',  ( 755.2512626584698410, -439.5436935675101040, 315.2512626584710915 ) ) ;
#16163 = DIRECTION ( 'NONE',  ( 0.000000000000000000, 0.000000000000000000, 1.000000000000000000 ) ) ;
#16164 = CARTESIAN_POINT ( 'NONE',  ( 755.3028492785439312, -279.2817908451526137, -335.9200461376539693 ) ) ;
#16165 = CARTESIAN_POINT ( 'NONE',  ( 796.7737145352015204, -164.6346026584200217, -370.7187646348536987 ) ) ;
#16166 = CARTESIAN_POINT ( 'NONE',  ( 767.7687537140311633, -71.90732993114760063, 372.7932403749916830 ) ) ;
#16167 = CARTESIAN_POINT ( 'NONE',  ( 787.4397851343537695, -141.7255117493291721, 374.2001403089903988 ) ) ;
#16168 = LINE ( 'NONE', #30250, #23962 ) ;
#16169 = SURFACE_STYLE_FILL_AREA ( #19188 ) ;
#16170 = CARTESIAN_POINT ( 'NONE',  ( 761.9338519418445230, -254.5328690171413655, -370.4231160770881957 ) ) ;
#16171 = AXIS2_PLACEMENT_3D ( 'NONE', #18445, #29301, #22119 ) ;
#16172 = CARTESIAN_POINT ( 'NONE',  ( -775.4999999999993179, -544.8427095258973623, -369.9999999999999432 ) ) ;
#16173 = CARTESIAN_POINT ( 'NONE',  ( 814.5518280994195948, -399.7255117493283478, 332.4837098697145734 ) ) ;
#16174 = CARTESIAN_POINT ( 'NONE',  ( 810.7187646348534145, -18.45278447660230725, 356.7737145352016341 ) ) ;
#16175 = CARTESIAN_POINT ( 'NONE',  ( 759.7806653035534055, -366.9982390220556567, -324.8639956371180801 ) ) ;
#16176 = CARTESIAN_POINT ( 'NONE',  ( 799.4546378042377910, 14.92167643740321381, 356.1575198192848006 ) ) ;
#16177 = CARTESIAN_POINT ( 'NONE',  ( 744.6391490659812007, -110.7363362996985501, -338.7502325331110455 ) ) ;
#16178 = CARTESIAN_POINT ( 'NONE',  ( 769.1273215169530886, -166.7146871989598367, -317.4527132478988847 ) ) ;
#16179 = CARTESIAN_POINT ( 'NONE',  ( 791.1614460488616487, -131.2601417444144829, 373.5763878283158874 ) ) ;
#16180 = DIRECTION ( 'NONE',  ( -1.000000000000000000, -0.000000000000000000, -0.000000000000000000 ) ) ;
#16181 = CARTESIAN_POINT ( 'NONE',  ( 762.3223304703356007, -55.54369356751127640, -322.3223304703362828 ) ) ;
#16182 = CARTESIAN_POINT ( 'NONE',  ( 803.2186876482843445, -175.9874144716871172, -350.0220218866286928 ) ) ;
#16183 = CARTESIAN_POINT ( 'NONE',  ( 757.8323909638827445, -122.6346026584201354, -352.1044303154654358 ) ) ;
#16184 = CARTESIAN_POINT ( 'NONE',  ( 757.8323909638827445, -170.6346026584199649, 352.1044303154654358 ) ) ;
#16185 = EDGE_CURVE ( 'NONE', #5955, #20856, #8684, .T. ) ;
#16186 = CARTESIAN_POINT ( 'NONE',  ( 770.0799878456142551, -421.9874144716863498, -362.9823548866085616 ) ) ;
#16187 = CARTESIAN_POINT ( 'NONE',  ( 804.4286716492782716, -305.3618753856922581, 345.3141322388244703 ) ) ;
#16188 = FACE_OUTER_BOUND ( 'NONE', #41651, .T. ) ;
#16189 = ORIENTED_EDGE ( 'NONE', *, *, #15084, .T. ) ;
#16190 = CARTESIAN_POINT ( 'NONE',  ( 801.3366627262608972, -32.53286901714208312, 353.0897708529566899 ) ) ;
#16191 = CARTESIAN_POINT ( 'NONE',  ( 814.8207195650702488, -266.1908817542435486, -336.2433038121456548 ) ) ;
#16192 = ORIENTED_EDGE ( 'NONE', *, *, #30882, .T. ) ;
#16193 = DIRECTION ( 'NONE',  ( 1.000000000000000000, 0.000000000000000000, 0.000000000000000000 ) ) ;
#16194 = EDGE_CURVE ( 'NONE', #11328, #11789, #36291, .T. ) ;
#16195 = CARTESIAN_POINT ( 'NONE',  ( 808.0189434323515343, -230.0891481129652618, 319.0252816721025511 ) ) ;
#16196 = CARTESIAN_POINT ( 'NONE',  ( 793.0897708529556667, -294.5545181178797520, 361.3366627262616362 ) ) ;
#16197 = CARTESIAN_POINT ( 'NONE',  ( 756.7813123517142913, -403.9874144716863498, 329.9779781133712504 ) ) ;
#16198 = VERTEX_POINT ( 'NONE', #27134 ) ;
#16199 = CARTESIAN_POINT ( 'NONE',  ( 805.2837595273609850, -122.7363362996985074, -340.5290396650784714 ) ) ;
#16200 = CARTESIAN_POINT ( 'NONE',  ( 774.6858677611749044, -105.7255117493293000, -315.5713283507209894 ) ) ;
#16201 = CARTESIAN_POINT ( 'NONE',  ( 802.1676090361155502, -326.6346026584194533, -327.8955696845344505 ) ) ;
#16202 = VERTEX_POINT ( 'NONE', #9351 ) ;
#16203 = CARTESIAN_POINT ( 'NONE',  ( 801.9419747391806368, -426.4527844766010389, -351.9812246680014027 ) ) ;
#16204 = CARTESIAN_POINT ( 'NONE',  ( 758.0580252608178853, -78.45278447660211896, -328.0187753319985404 ) ) ;
#16205 = CARTESIAN_POINT ( 'NONE',  ( 793.2243759319678702, -314.5328690171411949, 318.4439275373583200 ) ) ;
#16206 = DIRECTION ( 'NONE',  ( 0.000000000000000000, 0.000000000000000000, 1.000000000000000000 ) ) ;
#16207 = DIRECTION ( 'NONE',  ( -0.000000000000000000, -0.000000000000000000, 1.000000000000000000 ) ) ;
#16208 = DIRECTION ( 'NONE',  ( 0.000000000000000000, 0.000000000000000000, 1.000000000000000000 ) ) ;
#16209 = EDGE_LOOP ( 'NONE', ( #11941, #23740, #6831, #27059 ) ) ;
#16210 = CARTESIAN_POINT ( 'NONE',  ( 776.2046728542105711, -356.1908817542432075, -304.8212110874238761 ) ) ;
#16211 = EDGE_CURVE ( 'NONE', #38247, #41282, #5649, .T. ) ;
#16212 = CARTESIAN_POINT ( 'NONE',  ( 745.5313806188320314, -207.2817908451527842, 333.7943932421247268 ) ) ;
#16213 = CARTESIAN_POINT ( 'NONE',  ( 804.6798772138708955, -303.7255117493287457, -334.6312213355107019 ) ) ;
#16214 = EDGE_CURVE ( 'NONE', #37728, #14381, #37522, .T. ) ;
#16215 = CARTESIAN_POINT ( 'NONE',  ( 0.000000000000000000, 0.000000000000000000, -224.9999999999999716 ) ) ;
#16216 = CARTESIAN_POINT ( 'NONE',  ( 796.1575198192839480, -198.0090635724255606, -359.4546378042384163 ) ) ;
#16217 = EDGE_CURVE ( 'NONE', #34493, #44752, #35337, .T. ) ;
#16218 = CARTESIAN_POINT ( 'NONE',  ( 814.5518280994195948, -39.72551174932951312, 332.4837098697145734 ) ) ;
#16219 = LINE ( 'NONE', #22692, #31335 ) ;
#16220 = CARTESIAN_POINT ( 'NONE',  ( 777.4774526936600978, -394.2709662947829088, -304.7301800767028226 ) ) ;
#16221 = PLANE ( 'NONE',  #43843 ) ;
#16222 = CARTESIAN_POINT ( 'NONE',  ( 764.8639956371174549, -32.08914811296588709, 319.7806653035542013 ) ) ;
#16223 = CARTESIAN_POINT ( 'NONE',  ( 771.3260364891663130, -331.6454272087888171, 306.0683387631859773 ) ) ;
#16224 = CARTESIAN_POINT ( 'NONE',  ( 763.2262854647970016, -248.6346026584197659, 309.2812353651462445 ) ) ;
#16225 = CARTESIAN_POINT ( 'NONE',  ( 758.8095938919642549, -8.089148112965974136, -311.6929314249763365 ) ) ;
#16226 = CARTESIAN_POINT ( 'NONE',  ( 764.8639956371174549, -248.0891481129651481, -319.7806653035542013 ) ) ;
#16227 = DIRECTION ( 'NONE',  ( 0.000000000000000000, 0.000000000000000000, 1.000000000000000000 ) ) ;
#16228 = CARTESIAN_POINT ( 'NONE',  ( 794.9819416627830151, -372.9982390220557704, 319.9864689768909898 ) ) ;
#16229 = CARTESIAN_POINT ( 'NONE',  ( 761.4292242960306112, -113.4636090269712554, 323.2154366446414429 ) ) ;
#16230 = CARTESIAN_POINT ( 'NONE',  ( 802.7791456095903868, -52.71468719896020616, -329.0155153010375102 ) ) ;
#16231 = CARTESIAN_POINT ( 'NONE',  ( 811.6461892240364477, -28.71468719896028077, 324.1737431748509835 ) ) ;
#16232 = CARTESIAN_POINT ( 'NONE',  ( 757.8323909638828582, -386.6346026584192828, 352.1044303154654358 ) ) ;
#16233 = FACE_OUTER_BOUND ( 'NONE', #24305, .T. ) ;
#16234 = EDGE_CURVE ( 'NONE', #11032, #9887, #23737, .T. ) ;
#16235 = CARTESIAN_POINT ( 'NONE',  ( 989.9999999999992042, 239.9999999999998863, -360.0000000000000000 ) ) ;
#16236 = CARTESIAN_POINT ( 'NONE',  ( 810.1134526219336749, -128.5328690171417634, 357.8822607201570349 ) ) ;
#16237 = CARTESIAN_POINT ( 'NONE',  ( 804.9363028652555840, -400.2709662947828519, 338.2165204200192079 ) ) ;
#16238 = ORIENTED_EDGE ( 'NONE', *, *, #14494, .T. ) ;
#16239 = EDGE_CURVE ( 'NONE', #11829, #44849, #3862, .T. ) ;
#16240 = CARTESIAN_POINT ( 'NONE',  ( 761.2382568024794409, -327.6237781080502600, -356.9571628226838129 ) ) ;
#16242 = CARTESIAN_POINT ( 'NONE',  ( 758.0580252608178853, -150.4527844766018916, 328.0187753319985404 ) ) ;
#16241 = CARTESIAN_POINT ( 'NONE',  ( 762.1405469898971887, -193.5436935675108714, 357.8594530101015607 ) ) ;
#16243 = CARTESIAN_POINT ( 'NONE',  ( 786.2056067578752163, -347.8055962898683333, -374.4686193811670023 ) ) ;
#16244 = FACE_OUTER_BOUND ( 'NONE', #13705, .T. ) ;
#16245 = ORIENTED_EDGE ( 'NONE', *, *, #4645, .T. ) ;
#16246 = CARTESIAN_POINT ( 'NONE',  ( 792.1044303154645831, -372.4527844766010958, 317.8323909638837677 ) ) ;
#16247 = ORIENTED_EDGE ( 'NONE', *, *, #22162, .F. ) ;
#16248 = ADVANCED_FACE ( 'NONE', ( #9580 ), #33367, .T. ) ;
#16249 = ADVANCED_FACE ( 'NONE', ( #2403 ), #23421, .F. ) ;
#16250 = CARTESIAN_POINT ( 'NONE',  ( 747.2067596250078623, -219.1800572038744122, -352.2312462859687230 ) ) ;
#16251 = CARTESIAN_POINT ( 'NONE',  ( 759.0252816721024374, -120.9982390220565378, 368.0189434323527280 ) ) ;
#16252 = ORIENTED_EDGE ( 'NONE', *, *, #30606, .F. ) ;
#16253 = CARTESIAN_POINT ( 'NONE',  ( 785.3687786644885591, -179.3618753856927128, -315.3201227861280813 ) ) ;
#16254 = EDGE_LOOP ( 'NONE', ( #29574, #31935, #32104, #8665, #25098, #15425, #37730, #1992, #28012, #40432, #29879, #12428, #29715, #20032, #1596, #36770 ) ) ;
#16255 = CARTESIAN_POINT ( 'NONE',  ( 805.1927285166397041, -328.8164208402375834, -341.8018195045277707 ) ) ;
#16256 = CARTESIAN_POINT ( 'NONE',  ( 781.7834795799800531, 13.18357915976123174, -315.0636971347436202 ) ) ;
#16257 = CARTESIAN_POINT ( 'NONE',  ( 751.6929314249748586, -246.9982390220560546, 318.8095938919659034 ) ) ;
#16258 = CARTESIAN_POINT ( 'NONE',  ( 772.3691319403857278, -191.2601417444143976, 315.8894580844506663 ) ) ;
#16260 = DIRECTION ( 'NONE',  ( 0.000000000000000000, 0.000000000000000000, 1.000000000000000000 ) ) ;
#16259 = FACE_OUTER_BOUND ( 'NONE', #33588, .T. ) ;
#16261 = CARTESIAN_POINT ( 'NONE',  ( 879.9999999999992042, 469.9999999999998863, 350.0000000000000000 ) ) ;
#16262 = PRODUCT_DEFINITION_SHAPE ( 'NONE', 'NONE',  #22809 ) ;
#16263 = VERTEX_POINT ( 'NONE', #30584 ) ;
#16264 = CARTESIAN_POINT ( 'NONE',  ( 772.4468031744293057, -441.8272453906066630, -363.8651313633793620 ) ) ;
#16265 = CARTESIAN_POINT ( 'NONE',  ( 879.9999999999992042, 99.99999999999984368, 350.0000000000000000 ) ) ;
#16266 = DIRECTION ( 'NONE',  ( 8.659560562354932858E-17, 0.7071067811865474617, -0.7071067811865474617 ) ) ;
#16267 = ORIENTED_EDGE ( 'NONE', *, *, #11140, .T. ) ;
#16268 = CARTESIAN_POINT ( 'NONE',  ( 812.3518521366052028, -241.0999726633345119, -326.5853460496235243 ) ) ;
#16269 = CARTESIAN_POINT ( 'NONE',  ( 788.6739635108323228, -103.6454272087894850, 373.9316612368139090 ) ) ;
#16271 = CARTESIAN_POINT ( 'NONE',  ( 778.1981804954714335, -202.2709662947834772, -314.8072714833589885 ) ) ;
#16270 = CARTESIAN_POINT ( 'NONE',  ( -784.4999999999993179, -501.1515549466498669, -368.0974687824633520 ) ) ;
#16272 = CARTESIAN_POINT ( 'NONE',  ( 796.7845633553578182, -369.6237781080500895, -358.5707757039688204 ) ) ;
#16273 = DIRECTION ( 'NONE',  ( -0.000000000000000000, 1.000000000000000000, -0.000000000000000000 ) ) ;
#16274 = CARTESIAN_POINT ( 'NONE',  ( 744.6391490659812007, -230.7363362996981664, -338.7502325331110455 ) ) ;
#16275 = CARTESIAN_POINT ( 'NONE',  ( 999.9999999999992042, 239.9999999999998863, 350.0000000000000000 ) ) ;
#16276 = DIRECTION ( 'NONE',  ( -1.000000000000000000, -0.000000000000000000, -0.000000000000000000 ) ) ;
#16277 = CARTESIAN_POINT ( 'NONE',  ( 802.5472867521000353, -76.37269993606228979, -350.8726784830461156 ) ) ;
#16278 = CARTESIAN_POINT ( 'NONE',  ( 755.5913626894240451, -445.6454272087883055, 346.6156483768012890 ) ) ;
#16279 = LINE ( 'NONE', #15452, #552 ) ;
#16280 = CARTESIAN_POINT ( 'NONE',  ( 756.7813123517142913, -427.9874144716862929, -329.9779781133712504 ) ) ;
#16281 = CARTESIAN_POINT ( 'NONE',  ( 805.0032342141413437, -277.5436935675105588, -314.9967657858572352 ) ) ;
#16282 = CARTESIAN_POINT ( 'NONE',  ( 769.9999999999992042, 205.0000000000000568, -350.0000000000000000 ) ) ;
#16283 = CARTESIAN_POINT ( 'NONE',  ( 115.7583438952258774, 290.0000000000001705, -244.9999999999999716 ) ) ;
#16284 = CARTESIAN_POINT ( 'NONE',  ( 804.4286716492782716, -41.36187538569314626, -345.3141322388244703 ) ) ;
#16285 = CARTESIAN_POINT ( 'NONE',  ( 745.5313806188320314, -231.2817908451527558, 333.7943932421247268 ) ) ;
#16286 = CARTESIAN_POINT ( 'NONE',  ( 791.1614460488616487, -155.2601417444144261, -373.5763878283158874 ) ) ;
#16287 = CARTESIAN_POINT ( 'NONE',  ( 792.3570229623688874, -165.1800572038745258, 373.1304606946836202 ) ) ;
#16288 = CARTESIAN_POINT ( 'NONE',  ( 811.0346526505616112, -398.6346026584193396, -323.0537975583477532 ) ) ;
#16289 = CYLINDRICAL_SURFACE ( 'NONE', #33520, 2.749999999999863665 ) ;
#16290 = CARTESIAN_POINT ( 'NONE',  ( 755.3201227861273992, -243.7255117493287742, 345.3687786644892981 ) ) ;
#16291 = CARTESIAN_POINT ( 'NONE',  ( 763.8424801807145741, -42.00906357242603661, 320.5453621957614700 ) ) ;
#16292 = CARTESIAN_POINT ( 'NONE',  ( 771.2633955100217236, -383.9073299311466485, -363.4237431249939618 ) ) ;
#16293 = LINE ( 'NONE', #30375, #32074 ) ;
#16294 = EDGE_CURVE ( 'NONE', #820, #1585, #20057, .T. ) ;
#16295 = CARTESIAN_POINT ( 'NONE',  ( -78.83651009197140525, 260.0000000000000568, -191.9749999999935994 ) ) ;
#16296 = CARTESIAN_POINT ( 'NONE',  ( 779.4709603349208464, -96.35105083532370429, 314.7162404726379918 ) ) ;
#16297 = VERTEX_POINT ( 'NONE', #37751 ) ;
#16298 = CARTESIAN_POINT ( 'NONE',  ( 794.1144889064781864, -226.1692326535051052, -360.9840315886528401 ) ) ;
#16299 = CARTESIAN_POINT ( 'NONE',  ( 762.3223304703356007, -55.54369356751127640, 322.3223304703362828 ) ) ;
#16300 = CARTESIAN_POINT ( 'NONE',  ( 781.2497674668890113, -276.3510508353231785, -375.3608509340180603 ) ) ;
#16301 = LINE ( 'NONE', #19995, #23081 ) ;
#16302 = CARTESIAN_POINT ( 'NONE',  ( 749.8865473780648472, -380.5328690171409676, 322.1177392798429082 ) ) ;
#16303 = VERTEX_POINT ( 'NONE', #2643 ) ;
#16304 = CARTESIAN_POINT ( 'NONE',  ( 759.7806653035534055, -270.9982390220561115, 324.8639956371180801 ) ) ;
#16305 = CARTESIAN_POINT ( 'NONE',  ( 814.9108240113580450, 7.729033705215793582, 337.5031285880265273 ) ) ;
#16306 = CARTESIAN_POINT ( 'NONE',  ( 794.9819416627830151, -156.9982390220564241, -319.9864689768909898 ) ) ;
#16307 = CARTESIAN_POINT ( 'NONE',  ( 795.1360043628807261, -380.0891481129646650, 360.2193346964456282 ) ) ;
#16308 = EDGE_CURVE ( 'NONE', #30518, #11526, #3119, .T. ) ;
#16309 = CARTESIAN_POINT ( 'NONE',  ( 749.2812353651451076, -78.45278447660211896, -323.2262854647983090 ) ) ;
#16310 = CARTESIAN_POINT ( 'NONE',  ( 781.7834795799800531, -82.81642084023846451, -315.0636971347436202 ) ) ;
#16311 = ORIENTED_EDGE ( 'NONE', *, *, #42547, .T. ) ;
#16312 = CARTESIAN_POINT ( 'NONE',  ( 761.4292242960306112, -17.46360902697157513, -323.2154366446414429 ) ) ;
#16313 = ORIENTED_EDGE ( 'NONE', *, *, #45051, .F. ) ;
#16314 = CARTESIAN_POINT ( 'NONE',  ( 802.9823548866075953, -361.0999726633341425, -330.0799878456151077 ) ) ;
#16316 = CARTESIAN_POINT ( 'NONE',  ( 802.5472867521000353, -388.3726999360613945, 350.8726784830461156 ) ) ;
#16315 = CARTESIAN_POINT ( 'NONE',  ( 771.2633955100217236, -95.90732993114751537, 363.4237431249939618 ) ) ;
#16319 = CARTESIAN_POINT ( 'NONE',  ( 798.0661480581538854, -314.5328690171411949, 309.5768839229118043 ) ) ;
#16318 = DIRECTION ( 'NONE',  ( 0.000000000000000000, -0.9238795325112894030, 0.3826834323650836200 ) ) ;
#16317 = CARTESIAN_POINT ( 'NONE',  ( 758.8095938919644823, -416.0891481129646650, 311.6929314249762797 ) ) ;
#16320 = CARTESIAN_POINT ( 'NONE',  ( 788.7631598425961101, -121.4419599262327267, 305.7194118038759143 ) ) ;
#16321 = CARTESIAN_POINT ( 'NONE',  ( 798.5707757039680246, -341.4636090269705733, -356.7845633553585003 ) ) ;
#16322 = CARTESIAN_POINT ( 'NONE',  ( 756.5762568750052424, -315.1800572038740711, -348.7366044899774238 ) ) ;
#16323 = CARTESIAN_POINT ( 'NONE',  ( 786.2694204179717872, -141.2817908451530400, -305.1769319972829067 ) ) ;
#16324 = CARTESIAN_POINT ( 'NONE',  ( 808.3070685750230950, -450.9982390220554294, 361.1904061080339261 ) ) ;
#16326 = CARTESIAN_POINT ( 'NONE',  ( 786.4999999999993179, -110.5936016518799221, 750.6326042729449455 ) ) ;
#16325 = LINE ( 'NONE', #28083, #22601 ) ;
#16327 = CARTESIAN_POINT ( 'NONE',  ( 789.9200121543843807, -265.9874144716867477, -317.0176451133914384 ) ) ;
#16328 = CARTESIAN_POINT ( 'NONE',  ( 811.3240766477731540, -124.3726999360621619, -355.6651683502462902 ) ) ;
#16329 = DIRECTION ( 'NONE',  ( 8.326672684688676025E-16, 1.000000000000000000, -0.000000000000000000 ) ) ;
#16330 = CARTESIAN_POINT ( 'NONE',  ( 784.4999999999993179, -359.5698779088871788, -26.28906389436296109 ) ) ;
#16331 = CARTESIAN_POINT ( 'NONE',  ( 796.1575198192839480, -342.0090635724251342, 359.4546378042384163 ) ) ;
#16332 = CARTESIAN_POINT ( 'NONE',  ( 774.6312213355099630, -191.3618753856925991, 364.6798772138717482 ) ) ;
#16333 = ORIENTED_EDGE ( 'NONE', *, *, #17349, .F. ) ;
#16334 = CARTESIAN_POINT ( 'NONE',  ( 815.3608509340175488, -290.7363362996980527, 341.2497674668889545 ) ) ;
#16335 = CARTESIAN_POINT ( 'NONE',  ( 808.0189434323515343, -158.0891481129655176, -319.0252816721025511 ) ) ;
#16336 = CARTESIAN_POINT ( 'NONE',  ( 759.2380499001254748, 21.41625977839825978, -318.3449445151863415 ) ) ;
#16337 = CARTESIAN_POINT ( 'NONE',  ( 797.8822607201568644, -102.5545181178804057, 370.1134526219340160 ) ) ;
#16338 = CARTESIAN_POINT ( 'NONE',  ( 767.7687537140311633, -311.9073299311468759, -372.7932403749916830 ) ) ;
#16339 = CARTESIAN_POINT ( 'NONE',  ( 800.9747183278959710, -444.9982390220554862, -311.9810565676471583 ) ) ;
#16340 = CARTESIAN_POINT ( 'NONE',  ( 774.6312213355099630, -167.3618753856927412, 364.6798772138717482 ) ) ;
#16341 = CIRCLE ( 'NONE', #17106, 10.00000000000000888 ) ;
#16342 = ORIENTED_EDGE ( 'NONE', *, *, #409, .F. ) ;
#16343 = CARTESIAN_POINT ( 'NONE',  ( 791.0478386215596629, -405.8272453906067199, 306.7653713866226326 ) ) ;
#16344 = CARTESIAN_POINT ( 'NONE',  ( 815.1787889125755555, -342.8965053807773984, -343.7953271457877804 ) ) ;
#16345 = CARTESIAN_POINT ( 'NONE',  ( 746.8695393053150156, -101.9073299311474727, -327.6429770376306010 ) ) ;
#16346 = CARTESIAN_POINT ( 'NONE',  ( 754.7162404726377645, -38.73633629969877035, 339.4709603349214717 ) ) ;
#16347 = CARTESIAN_POINT ( 'NONE',  ( 763.2262854647970016, -392.6346026584193396, -309.2812353651462445 ) ) ;
#16348 = CARTESIAN_POINT ( 'NONE',  ( 791.7608162188021197, 205.0000000000000568, 350.0000000000000000 ) ) ;
#16349 = CARTESIAN_POINT ( 'NONE',  ( 803.8651313633788504, -437.2601417444135450, 332.4468031744301015 ) ) ;
#16350 = VERTEX_POINT ( 'NONE', #5193 ) ;
#16351 = CARTESIAN_POINT ( 'NONE',  ( 805.0264073115434940, -78.35105083532376113, 339.4763451958999099 ) ) ;
#16352 = EDGE_CURVE ( 'NONE', #23251, #17287, #35553, .T. ) ;
#16353 = CARTESIAN_POINT ( 'NONE',  ( 808.7758568127978833, -124.1692326535054463, -320.0363995740631822 ) ) ;
#16354 = CYLINDRICAL_SURFACE ( 'NONE', #29959, 10.00000000000000888 ) ;
#16355 = CARTESIAN_POINT ( 'NONE',  ( 776.2433038121456548, -276.8965053807776258, 374.8207195650711014 ) ) ;
#16356 = CARTESIAN_POINT ( 'NONE',  ( 788.8264449731201466, -93.18005720387479585, 363.6646147819170665 ) ) ;
#16357 = ORIENTED_EDGE ( 'NONE', *, *, #31257, .T. ) ;
#16358 = CARTESIAN_POINT ( 'NONE',  ( 755.0636971347428243, -268.2709662947833067, 341.7834795799807353 ) ) ;
#16359 = CARTESIAN_POINT ( 'NONE',  ( 745.1769319972822814, -425.8055962898680491, -346.2694204179732083 ) ) ;
#16360 = LINE ( 'NONE', #36706, #10640 ) ;
#16361 = ORIENTED_EDGE ( 'NONE', *, *, #9376, .F. ) ;
#16362 = ORIENTED_EDGE ( 'NONE', *, *, #9750, .T. ) ;
#16363 = CARTESIAN_POINT ( 'NONE',  ( 766.4474001241216001, -379.0999726633341993, -307.3154664389482491 ) ) ;
#16364 = CARTESIAN_POINT ( 'NONE',  ( 797.6776695296629214, -235.5436935675107293, -357.6776695296636603 ) ) ;
#16366 = CARTESIAN_POINT ( 'NONE',  ( 759.8311093483677041, -214.1692326535052189, 310.9282345327691814 ) ) ;
#16365 = CARTESIAN_POINT ( 'NONE',  ( 754.9967657858570647, -337.5436935675102745, 365.0032342141425943 ) ) ;
#16367 = APPLICATION_CONTEXT ( 'automotive_design' ) ;
#16368 = CARTESIAN_POINT ( 'NONE',  ( 783.0745993439762742, -224.1908817542436623, -365.1016975059196739 ) ) ;
#16369 = CARTESIAN_POINT ( 'NONE',  ( 802.1676090361156639, -230.6346026584197659, -327.8955696845344505 ) ) ;
#16370 = VECTOR ( 'NONE', #23181, 1000.000000000000000 ) ;
#16371 = CARTESIAN_POINT ( 'NONE',  ( 765.0180583372156207, -408.9982390220556567, -360.0135310231089534 ) ) ;
#16372 = ORIENTED_EDGE ( 'NONE', *, *, #21570, .T. ) ;
#16373 = CARTESIAN_POINT ( 'NONE',  ( 785.3141322388236176, -213.7255117493289731, 364.4286716492789537 ) ) ;
#16374 = CARTESIAN_POINT ( 'NONE',  ( 758.0580252608178853, -102.4527844766020337, -328.0187753319985404 ) ) ;
#16375 = ORIENTED_EDGE ( 'NONE', *, *, #26602, .F. ) ;
#16376 = CARTESIAN_POINT ( 'NONE',  ( 747.2067596250078623, -363.1800572038739006, 352.2312462859687230 ) ) ;
#16377 = DIRECTION ( 'NONE',  ( -1.000000000000000000, -0.000000000000000000, 0.000000000000000000 ) ) ;
#16378 = FACE_OUTER_BOUND ( 'NONE', #8920, .T. ) ;
#16379 = DIRECTION ( 'NONE',  ( 0.000000000000000000, 0.000000000000000000, -1.000000000000000000 ) ) ;
#16380 = CARTESIAN_POINT ( 'NONE',  ( 793.0897708529556667, -222.5545181178800362, 361.3366627262616362 ) ) ;
#16381 = CARTESIAN_POINT ( 'NONE',  ( 800.2193346964447755, -90.99823902205663728, 355.1360043628815788 ) ) ;
#16382 = VERTEX_POINT ( 'NONE', #38915 ) ;
#16383 = CARTESIAN_POINT ( 'NONE',  ( 804.1009440267234822, -455.4636090269701754, -314.0944755984392600 ) ) ;
#16384 = CARTESIAN_POINT ( 'NONE',  ( 782.4968714119720516, -58.81642084023854267, -305.0891759886411023 ) ) ;
#16385 = CARTESIAN_POINT ( 'NONE',  ( 756.1348686366196716, -257.2601417444141134, 347.5531968255698416 ) ) ;
#16386 = CARTESIAN_POINT ( 'NONE',  ( 803.6646147819161570, -425.9073299311463074, -348.8264449731210561 ) ) ;
#16387 = CARTESIAN_POINT ( 'NONE',  ( 755.3201227861273992, -51.72551174932947049, -345.3687786644892981 ) ) ;
#16388 = CARTESIAN_POINT ( 'NONE',  ( 782.4968714119720516, -442.8164208402372992, 305.0891759886411023 ) ) ;
#16389 = DIRECTION ( 'NONE',  ( 0.000000000000000000, 0.000000000000000000, 1.000000000000000000 ) ) ;
#16390 = CARTESIAN_POINT ( 'NONE',  ( 763.0428371773158460, -299.4636090269707438, -358.7617431975195359 ) ) ;
#16391 = CARTESIAN_POINT ( 'NONE',  ( 782.4968714119720516, -178.8164208402381519, -305.0891759886411023 ) ) ;
#16392 = CARTESIAN_POINT ( 'NONE',  ( 744.7301800767019131, -76.81642084023845030, 337.4774526936615757 ) ) ;
#16393 = CARTESIAN_POINT ( 'NONE',  ( 747.2067596250078623, -147.1800572038746395, 352.2312462859687230 ) ) ;
#16394 = AXIS2_PLACEMENT_3D ( 'NONE', #5037, #19129, #43383 ) ;
#16395 = FACE_OUTER_BOUND ( 'NONE', #18483, .T. ) ;
#16396 = CARTESIAN_POINT ( 'NONE',  ( 800.1688906516307043, -226.1692326535051052, -369.0717654672308186 ) ) ;
#16397 = CARTESIAN_POINT ( 'NONE',  ( 745.7194118038753459, -421.6454272087885329, 348.7631598425976449 ) ) ;
#16398 = CARTESIAN_POINT ( 'NONE',  ( 754.9967657858570647, -265.5436935675106156, -365.0032342141425374 ) ) ;
#16399 = DIRECTION ( 'NONE',  ( 0.000000000000000000, 0.000000000000000000, -1.000000000000000000 ) ) ;
#16400 = CARTESIAN_POINT ( 'NONE',  ( 763.0537975583475827, -384.4527844766011526, 371.0346526505627480 ) ) ;
#16401 = CARTESIAN_POINT ( 'NONE',  ( 745.7998596910086917, -5.361875385693257279, 332.5602148656461168 ) ) ;
#16402 = CARTESIAN_POINT ( 'NONE',  ( 758.0580252608178853, -366.4527844766012095, -328.0187753319985404 ) ) ;
#16403 = CARTESIAN_POINT ( 'NONE',  ( 765.8855110935204493, -22.16923265350575889, 319.0159684113471599 ) ) ;
#16404 = CARTESIAN_POINT ( 'NONE',  ( 748.6759233522253680, -88.37269993606226137, -324.3348316497537098 ) ) ;
#16405 = CARTESIAN_POINT ( 'NONE',  ( 772.3691319403857278, -167.2601417444143976, -315.8894580844506663 ) ) ;
#16406 = CARTESIAN_POINT ( 'NONE',  ( 811.6461892240364477, -172.7146871989598083, 324.1737431748509835 ) ) ;
#16407 = CARTESIAN_POINT ( 'NONE',  ( 781.7834795799800531, 13.18357915976123174, 315.0636971347436202 ) ) ;
#16408 = CARTESIAN_POINT ( 'NONE',  ( 810.1134526219336749, -176.5328690171416213, 357.8822607201570349 ) ) ;
#16409 = VERTEX_POINT ( 'NONE', #7268 ) ;
#16410 = CARTESIAN_POINT ( 'NONE',  ( 805.0264073115434940, -174.3510508353234627, -339.4763451958999099 ) ) ;
#16411 = CARTESIAN_POINT ( 'NONE',  ( 794.9819416627830151, -180.9982390220563389, 319.9864689768909898 ) ) ;
#16412 = CARTESIAN_POINT ( 'NONE',  ( 745.1769319972822814, 6.194403710130517382, -346.2694204179732083 ) ) ;
#16414 = CARTESIAN_POINT ( 'NONE',  ( 778.1981804954715471, -298.2709662947831930, 314.8072714833591021 ) ) ;
#16413 = CARTESIAN_POINT ( 'NONE',  ( 757.8323909638827445, -290.6346026584195101, 352.1044303154654358 ) ) ;
#16415 = CARTESIAN_POINT ( 'NONE',  ( 311.1634899080286232, 260.0000000000000000, -202.7499999999961915 ) ) ;
#16416 = ORIENTED_EDGE ( 'NONE', *, *, #6076, .T. ) ;
#16417 = CARTESIAN_POINT ( 'NONE',  ( 759.2295555964440155, -16.16923265350578021, 353.9708237608231229 ) ) ;
#16418 = CARTESIAN_POINT ( 'NONE',  ( 745.5313806188320314, -279.2817908451526137, -333.7943932421247268 ) ) ;
#16419 = ORIENTED_EDGE ( 'NONE', *, *, #31104, .F. ) ;
#16420 = DIRECTION ( 'NONE',  ( 0.000000000000000000, 0.000000000000000000, 1.000000000000000000 ) ) ;
#16421 = CARTESIAN_POINT ( 'NONE',  ( 787.4397851343537695, -237.7255117493289163, 374.2001403089903988 ) ) ;
#16422 = CARTESIAN_POINT ( 'NONE',  ( 796.1575198192839480, -318.0090635724251911, 359.4546378042384163 ) ) ;
#16423 = CARTESIAN_POINT ( 'NONE',  ( 804.9511171171677688, -413.8055962898681059, 335.8780910478229202 ) ) ;
#16424 = ADVANCED_FACE ( 'NONE', ( #10035 ), #23866, .F. ) ;
#16425 = EDGE_LOOP ( 'NONE', ( #36307, #2552 ) ) ;
#16426 = CARTESIAN_POINT ( 'NONE',  ( 790.9844846989617508, -118.3726999360621619, -317.2208543904092721 ) ) ;
#16427 = CARTESIAN_POINT ( 'NONE',  ( 781.7834795799800531, -130.8164208402383224, -315.0636971347436202 ) ) ;
#16428 = AXIS2_PLACEMENT_3D ( 'NONE', #17938, #3630, #39194 ) ;
#16429 = CARTESIAN_POINT ( 'NONE',  ( 755.5713283507202505, -317.3618753856922581, -334.6858677611754729 ) ) ;
#16430 = VERTEX_POINT ( 'NONE', #24102 ) ;
#16431 = CARTESIAN_POINT ( 'NONE',  ( 762.3223304703356007, -439.5436935675101040, -322.3223304703362828 ) ) ;
#16432 = CARTESIAN_POINT ( 'NONE',  ( 757.2208543904082489, -304.7146871989594388, 350.9844846989624330 ) ) ;
#16433 = CARTESIAN_POINT ( 'NONE',  ( 793.4841229319055174, -454.6421165850785542, 372.0217908949762773 ) ) ;
#16434 = DIRECTION ( 'NONE',  ( 1.000000000000000000, -4.147566128926370535E-16, 0.000000000000000000 ) ) ;
#16435 = CARTESIAN_POINT ( 'NONE',  ( 799.2566176426618085, -120.0090635724258021, 324.0069404352559559 ) ) ;
#16436 = CARTESIAN_POINT ( 'NONE',  ( 785.3687786644884454, 12.63812461430668321, 315.3201227861279676 ) ) ;
#16437 = ORIENTED_EDGE ( 'NONE', *, *, #24177, .T. ) ;
#16438 = CARTESIAN_POINT ( 'NONE',  ( 778.7629533639073998, -344.7363362996978253, -375.0009284576466371 ) ) ;
#16439 = CARTESIAN_POINT ( 'NONE',  ( 752.7379699480933368, -204.0090635724255606, 361.9858362298580232 ) ) ;
#16440 = CARTESIAN_POINT ( 'NONE',  ( 764.8639956371174549, -320.0891481129648355, -319.7806653035542013 ) ) ;
#16441 = DIRECTION ( 'NONE',  ( -1.880165489482579047E-16, -1.000000000000000000, -0.000000000000000000 ) ) ;
#16442 = CARTESIAN_POINT ( 'NONE',  ( 783.0745993439762742, -200.1908817542436907, -365.1016975059196739 ) ) ;
#16443 = EDGE_CURVE ( 'NONE', #41246, #29996, #45373, .T. ) ;
#16444 = CARTESIAN_POINT ( 'NONE',  ( 782.4968714119720516, -58.81642084023854267, 305.0891759886411023 ) ) ;
#16445 = DIRECTION ( 'NONE',  ( 0.000000000000000000, 1.000000000000000000, -0.000000000000000000 ) ) ;
#16446 = CARTESIAN_POINT ( 'NONE',  ( 801.1904061080338124, -380.0891481129647218, -368.3070685750236066 ) ) ;
#16447 = DIRECTION ( 'NONE',  ( 0.000000000000000000, 0.000000000000000000, -1.000000000000000000 ) ) ;
#16448 = CARTESIAN_POINT ( 'NONE',  ( 750.9282345327678740, -328.9181544815160692, 319.8311093483690115 ) ) ;
#16449 = DIRECTION ( 'NONE',  ( 0.000000000000000000, 0.000000000000000000, 1.000000000000000000 ) ) ;
#16450 = CARTESIAN_POINT ( 'NONE',  ( 801.1904061080336987, -284.0891481129650629, 368.3070685750235498 ) ) ;
#16451 = CARTESIAN_POINT ( 'NONE',  ( 749.2812353651451076, -6.452784476602343666, -323.2262854647983090 ) ) ;
#16452 = EDGE_CURVE ( 'NONE', #42952, #5266, #26721, .T. ) ;
#16453 = CARTESIAN_POINT ( 'NONE',  ( 774.6858677611749044, -249.7255117493288594, -315.5713283507209894 ) ) ;
#16454 = CARTESIAN_POINT ( 'NONE',  ( -784.4999999999993179, -512.9681489794448908, -339.9999999999999432 ) ) ;
#16455 = CARTESIAN_POINT ( 'NONE',  ( 801.9419747391806368, -354.4527844766012095, 351.9812246680014027 ) ) ;
#16456 = CARTESIAN_POINT ( 'NONE',  ( 783.0745993439762742, -104.1908817542440175, 365.1016975059196739 ) ) ;
#16457 = CARTESIAN_POINT ( 'NONE',  ( 761.2382568024794409, -63.62377810805107714, -356.9571628226838129 ) ) ;
#16458 = CARTESIAN_POINT ( 'NONE',  ( 749.8865473780648472, -68.53286901714197654, 322.1177392798429082 ) ) ;
#16459 = CARTESIAN_POINT ( 'NONE',  ( 755.0636971347428243, -364.2709662947830793, 341.7834795799807353 ) ) ;
#16460 = AXIS2_PLACEMENT_3D ( 'NONE', #5121, #40246, #23343 ) ;
#16461 = CARTESIAN_POINT ( 'NONE',  ( 799.9999999999993179, -357.6843811873878280, -0.3380660510726891665 ) ) ;
#16462 = CARTESIAN_POINT ( 'NONE',  ( 989.9999999999992042, 249.9999999999998863, -350.0000000000000000 ) ) ;
#16463 = CARTESIAN_POINT ( 'NONE',  ( 801.9858362298568863, -147.0783235625962959, 312.7379699480935642 ) ) ;
#16464 = CARTESIAN_POINT ( 'NONE',  ( 765.0180583372156207, -432.9982390220555999, 360.0135310231089534 ) ) ;
#16465 = VERTEX_POINT ( 'NONE', #10253 ) ;
#16466 = CARTESIAN_POINT ( 'NONE',  ( 789.9200121543843807, -361.9874144716864635, -317.0176451133914384 ) ) ;
#16468 = CARTESIAN_POINT ( 'NONE',  ( 797.8594530101009923, -181.5436935675108430, 322.1405469898982119 ) ) ;
#16467 = CARTESIAN_POINT ( 'NONE',  ( 771.1735550268778070, -201.1800572038744690, 316.3353852180827630 ) ) ;
#16469 = CARTESIAN_POINT ( 'NONE',  ( 766.5853460496234675, -349.9874144716865771, -372.3518521366060554 ) ) ;
#16470 = CARTESIAN_POINT ( 'NONE',  ( -200.7583438952259201, 394.6698570112193920, -244.9999999999999716 ) ) ;
#16471 = EDGE_CURVE ( 'NONE', #12197, #20750, #35416, .T. ) ;
#16472 = ORIENTED_EDGE ( 'NONE', *, *, #4424, .F. ) ;
#16473 = CARTESIAN_POINT ( 'NONE',  ( 804.6798772138708955, -399.7255117493283478, 334.6312213355107019 ) ) ;
#16474=STYLED_ITEM('',(#45758),#33391);
#16475 = EDGE_CURVE ( 'NONE', #20164, #12460, #33349, .T. ) ;
#16476 = ORIENTED_EDGE ( 'NONE', *, *, #38309, .F. ) ;
#16477 =( LENGTH_UNIT ( ) NAMED_UNIT ( * ) SI_UNIT ( .MILLI., .METRE. ) );
#16478 = CARTESIAN_POINT ( 'NONE',  ( 759.0252816721024374, -216.9982390220562252, -368.0189434323527280 ) ) ;
#16479 = CARTESIAN_POINT ( 'NONE',  ( 772.4837098697145166, -119.3618753856928834, 374.5518280994205611 ) ) ;
#16480 = ORIENTED_EDGE ( 'NONE', *, *, #27744, .T. ) ;
#16481 = CARTESIAN_POINT ( 'NONE',  ( 762.3223304703356007, -199.5436935675108430, -322.3223304703362828 ) ) ;
#16482 = ORIENTED_EDGE ( 'NONE', *, *, #13551, .T. ) ;
#16483 = CARTESIAN_POINT ( 'NONE',  ( 788.8264449731200330, -333.1800572038740142, -363.6646147819171233 ) ) ;
#16484 = CARTESIAN_POINT ( 'NONE',  ( 800.0135310231082713, 9.910851887033969021, -325.0180583372163028 ) ) ;
#16485 = CARTESIAN_POINT ( 'NONE',  ( 763.0537975583475827, -264.4527844766016074, 371.0346526505627480 ) ) ;
#16486 = CARTESIAN_POINT ( 'NONE',  ( 787.6308680596127942, -179.2601417444143692, 364.1105419155492768 ) ) ;
#16488 = DIRECTION ( 'NONE',  ( 1.000000000000000000, -0.000000000000000000, -0.000000000000000000 ) ) ;
#16487 = CYLINDRICAL_SURFACE ( 'NONE', #18874, 10.00000000000000888 ) ;
#16489 = CARTESIAN_POINT ( 'NONE',  ( 787.4999999999992042, -462.9681489794447202, 270.0000000000000568 ) ) ;
#16490 = ORIENTED_EDGE ( 'NONE', *, *, #31148, .F. ) ;
#16491 = CARTESIAN_POINT ( 'NONE',  ( 790.9844846989617508, -454.3726999360611103, -317.2208543904092721 ) ) ;
#16492 = CARTESIAN_POINT ( 'NONE',  ( -879.9999999999992042, 240.0000000000000568, -244.9999999999999716 ) ) ;
#16493 = DIRECTION ( 'NONE',  ( -0.000000000000000000, -0.000000000000000000, 1.000000000000000000 ) ) ;
#16494 = AXIS2_PLACEMENT_3D ( 'NONE', #5936, #30657, #44756 ) ;
#16495 = VERTEX_POINT ( 'NONE', #13958 ) ;
#16496 = CARTESIAN_POINT ( 'NONE',  ( 791.0478386215596629, -237.8272453906072599, -306.7653713866226326 ) ) ;
#16497 = CIRCLE ( 'NONE', #15739, 10.00000000000000888 ) ;
#16498 = CARTESIAN_POINT ( 'NONE',  ( 791.0478386215596629, -93.82724539060770041, 306.7653713866226326 ) ) ;
#16500 = CARTESIAN_POINT ( 'NONE',  ( 797.8594530101008786, -181.5436935675108145, -322.1405469898980982 ) ) ;
#16499 = CARTESIAN_POINT ( 'NONE',  ( 999.9999999999992042, 249.9999999999998863, 200.9999999999999432 ) ) ;
#16501 = EDGE_CURVE ( 'NONE', #18880, #7001, #41679, .T. ) ;
#16502 = CARTESIAN_POINT ( 'NONE',  ( 780.5290396650775619, -372.3510508353228374, -365.2837595273619513 ) ) ;
#16503 = CARTESIAN_POINT ( 'NONE',  ( 810.4231160770870019, -240.5545181178798941, -321.9338519418446936 ) ) ;
#16504 = DIRECTION ( 'NONE',  ( 0.000000000000000000, -1.000000000000000000, 0.000000000000000000 ) ) ;
#16505 = CARTESIAN_POINT ( 'NONE',  ( -784.4999999999993179, -512.9681489794448908, -327.9999999999999432 ) ) ;
#16506 = CARTESIAN_POINT ( 'NONE',  ( 805.2837595273609850, -74.73633629969866377, -340.5290396650784714 ) ) ;
#16507 = CARTESIAN_POINT ( 'NONE',  ( 754.7162404726377645, -422.7363362996975980, 339.4709603349214717 ) ) ;
#16508 = EDGE_CURVE ( 'NONE', #14904, #24881, #24552, .T. ) ;
#16509 = DIRECTION ( 'NONE',  ( -0.000000000000000000, 0.000000000000000000, -1.000000000000000000 ) ) ;
#16510 = CARTESIAN_POINT ( 'NONE',  ( 804.1601925771018387, -439.4419599262316751, -346.5483106153029098 ) ) ;
#16511 = CARTESIAN_POINT ( 'NONE',  ( 763.2262854647970016, -272.6346026584196807, -309.2812353651462445 ) ) ;
#16512 = DIRECTION ( 'NONE',  ( -1.000000000000000000, 0.000000000000000000, 0.000000000000000000 ) ) ;
#16513 = FACE_OUTER_BOUND ( 'NONE', #480, .T. ) ;
#16514 = CARTESIAN_POINT ( 'NONE',  ( 797.6776695296629214, -43.54369356751131903, -357.6776695296636603 ) ) ;
#16515 = VECTOR ( 'NONE', #39353, 1000.000000000000114 ) ;
#16516 = CARTESIAN_POINT ( 'NONE',  ( 813.5763878283155464, -219.8272453906073167, 351.1614460488615350 ) ) ;
#16517 = CARTESIAN_POINT ( 'NONE',  ( 754.0944755984390895, -159.6237781080508285, -364.1009440267246760 ) ) ;
#16518 = CARTESIAN_POINT ( 'NONE',  ( 810.7187646348534145, -186.4527844766017779, 356.7737145352016341 ) ) ;
#16519 = CARTESIAN_POINT ( 'NONE',  ( 813.1304606946830518, -401.9073299311463643, -352.3570229623690580 ) ) ;
#16520 = EDGE_CURVE ( 'NONE', #19442, #30216, #3094, .T. ) ;
#16521 = EDGE_CURVE ( 'NONE', #27562, #2204, #2874, .T. ) ;
#16522 = CYLINDRICAL_SURFACE ( 'NONE', #20237, 2.749999999999863665 ) ;
#16523 = CARTESIAN_POINT ( 'NONE',  ( 759.7806653035534055, -270.9982390220561115, 324.8639956371180801 ) ) ;
#16524 = CARTESIAN_POINT ( 'NONE',  ( 769.9779781133707957, -43.09997266333511590, 316.7813123517150871 ) ) ;
#16525 = CARTESIAN_POINT ( 'NONE',  ( 804.4286716492782716, -425.3618753856919170, -345.3141322388244703 ) ) ;
#16526 = CARTESIAN_POINT ( 'NONE',  ( 799.9999999999993179, -512.9681489794448908, -339.9999999999999432 ) ) ;
#16527 = DIRECTION ( 'NONE',  ( -1.000000000000000000, -0.000000000000000000, -0.000000000000000000 ) ) ;
#16529 = CARTESIAN_POINT ( 'NONE',  ( 762.1405469898971887, -337.5436935675102177, 357.8594530101015607 ) ) ;
#16528 = CARTESIAN_POINT ( 'NONE',  ( 800.7704444035546203, -76.16923265350557415, 326.0291762391768771 ) ) ;
#16530 = ORIENTED_EDGE ( 'NONE', *, *, #21305, .T. ) ;
#16531 = CARTESIAN_POINT ( 'NONE',  ( 790.8726784830453198, -250.7146871989595809, -362.5472867521010585 ) ) ;
#16532 = VECTOR ( 'NONE', #14718, 1000.000000000000000 ) ;
#16533 = CARTESIAN_POINT ( 'NONE',  ( 759.9864689768902508, -122.0891481129656171, -354.9819416627836404 ) ) ;
#16534 = CARTESIAN_POINT ( 'NONE',  ( 781.8018195045266339, -70.27096629478397460, 365.1927285166406705 ) ) ;
#16535 = CARTESIAN_POINT ( 'NONE',  ( 756.1443688327750579, -261.6237781080504305, -314.3581564841659315 ) ) ;
#16536 = LINE ( 'NONE', #19530, #5417 ) ;
#16537 = CARTESIAN_POINT ( 'NONE',  ( 761.9338519418445230, -374.5328690171410813, 370.4231160770881957 ) ) ;
#16538 = ORIENTED_EDGE ( 'NONE', *, *, #17293, .F. ) ;
#16539 = CARTESIAN_POINT ( 'NONE',  ( 755.5713283507202505, -293.3618753856923718, 334.6858677611754729 ) ) ;
#16540 = CARTESIAN_POINT ( 'NONE',  ( 792.2269492836462632, -443.1233509495419298, 372.8191558162650949 ) ) ;
#16541 = ADVANCED_FACE ( 'NONE', ( #17183, #38667 ), #37983, .T. ) ;
#16542 = CARTESIAN_POINT ( 'NONE',  ( 797.6776695296629214, -163.5436935675109567, -357.6776695296636603 ) ) ;
#16543 = CARTESIAN_POINT ( 'NONE',  ( 755.5713283507202505, -389.3618753856919739, 334.6858677611754729 ) ) ;
#16544 = CARTESIAN_POINT ( 'NONE',  ( 767.6429770376289525, -129.1800572038746111, -306.8695393053162093 ) ) ;
#16545 = CARTESIAN_POINT ( 'NONE',  ( 774.6858677611749044, -105.7255117493293000, -315.5713283507209894 ) ) ;
#16546 = EDGE_LOOP ( 'NONE', ( #38154, #31190, #37488, #26988, #45575, #31587 ) ) ;
#16547 = CARTESIAN_POINT ( 'NONE',  ( 775.8780910478218402, -33.28179084515333130, -364.9511171171680530 ) ) ;
#16548 = CARTESIAN_POINT ( 'NONE',  ( 800.9840315886518738, -340.9181544815160123, -354.1144889064786412 ) ) ;
#16549 = AXIS2_PLACEMENT_3D ( 'NONE', #452, #39733, #39497 ) ;
#16551 = CARTESIAN_POINT ( 'NONE',  ( 766.0291762391763086, -418.9181544815157849, 360.7704444035551319 ) ) ;
#16550 = CARTESIAN_POINT ( 'NONE',  ( 791.9812246680005501, -92.63460265842026331, 361.9419747391813189 ) ) ;
#16552 = CARTESIAN_POINT ( 'NONE',  ( 754.9735926884551418, -90.35105083532373271, 340.5236548041000333 ) ) ;
#16555 = CARTESIAN_POINT ( 'NONE',  ( 776.2433038121456548, -348.8965053807774552, 374.8207195650711014 ) ) ;
#16554 = CARTESIAN_POINT ( 'NONE',  ( -598.8365100919716042, 256.5000000000001705, -202.7499999999898819 ) ) ;
#16553 = DIRECTION ( 'NONE',  ( 0.000000000000000000, -1.000000000000000000, 0.000000000000000000 ) ) ;
#16556 = CIRCLE ( 'NONE', #25412, 50.00000000000004263 ) ;
#16557 = CARTESIAN_POINT ( 'NONE',  ( 772.4468031744293057, -369.8272453906068904, -363.8651313633793620 ) ) ;
#16558 = CARTESIAN_POINT ( 'NONE',  ( 785.3141322388236176, -333.7255117493286320, -364.4286716492789537 ) ) ;
#16559 = CARTESIAN_POINT ( 'NONE',  ( 781.2370466360911223, -140.7363362996984506, -304.9990715423533629 ) ) ;
#16560 = CIRCLE ( 'NONE', #28342, 30.00000000000002842 ) ;
#16561 = CARTESIAN_POINT ( 'NONE',  ( 810.4231160770870019, -0.5545181178807169209, 321.9338519418446936 ) ) ;
#16563 = CARTESIAN_POINT ( 'NONE',  ( 355.8971257818259915, 290.0000000000001137, -320.0000000000000568 ) ) ;
#16562 = DIRECTION ( 'NONE',  ( 0.000000000000000000, 0.000000000000000000, 1.000000000000000000 ) ) ;
#16564 = ADVANCED_FACE ( 'NONE', ( #31271 ), #16965, .T. ) ;
#16565 = CARTESIAN_POINT ( 'NONE',  ( 779.4709603349208464, -264.3510508353232353, -314.7162404726379918 ) ) ;
#16566 = CARTESIAN_POINT ( 'NONE',  ( 788.6739635108323228, -103.6454272087894850, -373.9316612368139090 ) ) ;
#16567 = DIRECTION ( 'NONE',  ( -1.000000000000000000, -0.000000000000000000, -0.000000000000000000 ) ) ;
#16568 = CARTESIAN_POINT ( 'NONE',  ( 779.9999999999992042, -452.9681489794448339, -339.9999999999999432 ) ) ;
#16569 = CARTESIAN_POINT ( 'NONE',  ( 766.0291762391763086, -322.9181544815161260, 360.7704444035551319 ) ) ;
#16570 = EDGE_CURVE ( 'NONE', #38643, #11526, #88, .T. ) ;
#16571 = CIRCLE ( 'NONE', #15088, 19.99999999999990763 ) ;
#16572 = ORIENTED_EDGE ( 'NONE', *, *, #36240, .T. ) ;
#16573 = CARTESIAN_POINT ( 'NONE',  ( 797.8822607201568644, -294.5545181178797520, 370.1134526219340160 ) ) ;
#16574 = AXIS2_PLACEMENT_3D ( 'NONE', #21055, #38387, #10662 ) ;
#16575 = CARTESIAN_POINT ( 'NONE',  ( 745.7998596910086917, -173.3618753856927128, -332.5602148656461168 ) ) ;
#16576 = DIRECTION ( 'NONE',  ( -1.000000000000000000, 0.000000000000000000, -0.000000000000000000 ) ) ;
#16577 = CARTESIAN_POINT ( 'NONE',  ( 788.6739635108323228, -103.6454272087894850, 373.9316612368139090 ) ) ;
#16578 = CARTESIAN_POINT ( 'NONE',  ( 745.7998596910086917, -317.3618753856922581, -332.5602148656461168 ) ) ;
#16579 = EDGE_CURVE ( 'NONE', #38546, #30501, #33382, .T. ) ;
#16580 = CARTESIAN_POINT ( 'NONE',  ( 779.9999999999992042, -452.9681489794448339, 329.9999999999999432 ) ) ;
#16581 = CARTESIAN_POINT ( 'NONE',  ( 999.9999999999992042, -590.0000000000001137, 350.0000000000000000 ) ) ;
#16582 = CARTESIAN_POINT ( 'NONE',  ( 800.0135310231082713, -134.0891481129655745, 325.0180583372163028 ) ) ;
#16583 = VERTEX_POINT ( 'NONE', #28032 ) ;
#16584 = CARTESIAN_POINT ( 'NONE',  ( 776.2046728542105711, -428.1908817542430938, 304.8212110874238761 ) ) ;
#16585 = CARTESIAN_POINT ( 'NONE',  ( 749.8865473780648472, -380.5328690171409676, -322.1177392798429082 ) ) ;
#16586 = CARTESIAN_POINT ( 'NONE',  ( 814.9108240113580450, -112.2709662947838325, -337.5031285880265273 ) ) ;
#16587 = AXIS2_PLACEMENT_3D ( 'NONE', #42668, #39678, #7562 ) ;
#16588 = CARTESIAN_POINT ( 'NONE',  ( 766.0291762391763086, -34.91815448151697154, 360.7704444035551319 ) ) ;
#16589 = CARTESIAN_POINT ( 'NONE',  ( 805.0032342141412300, -373.5436935675101040, -314.9967657858571783 ) ) ;
#16590 = DIRECTION ( 'NONE',  ( -1.000000000000000000, -0.000000000000000000, -0.000000000000000000 ) ) ;
#16591 = CARTESIAN_POINT ( 'NONE',  ( 783.7566961878529810, 23.10349461922137237, 305.1792804349288417 ) ) ;
#16592 = ORIENTED_EDGE ( 'NONE', *, *, #24578, .T. ) ;
#16593 = AXIS2_PLACEMENT_3D ( 'NONE', #44011, #21935, #1971 ) ;
#16594 = CARTESIAN_POINT ( 'NONE',  ( 811.6461892240364477, -148.7146871989598935, -324.1737431748509835 ) ) ;
#16595 = DIRECTION ( 'NONE',  ( 0.000000000000000000, 0.000000000000000000, 1.000000000000000000 ) ) ;
#16596 = CARTESIAN_POINT ( 'NONE',  ( 805.9055244015594326, -291.6237781080503169, 315.8990559732753240 ) ) ;
#16597 = CARTESIAN_POINT ( 'NONE',  ( 765.0180583372156207, -96.99823902205660886, 360.0135310231089534 ) ) ;
#16598 = ORIENTED_EDGE ( 'NONE', *, *, #42492, .T. ) ;
#16599 = CARTESIAN_POINT ( 'NONE',  ( 756.3353852180819104, -269.9073299311468190, 331.1735550268788302 ) ) ;
#16600 = AXIS2_PLACEMENT_3D ( 'NONE', #33554, #40942, #16227 ) ;
#16601 = CARTESIAN_POINT ( 'NONE',  ( 792.3570229623688874, 2.819942796124898177, -373.1304606946836202 ) ) ;
#16602 = CARTESIAN_POINT ( 'NONE',  ( 999.5857864376259840, -600.0000000000001137, -360.0000000000000000 ) ) ;
#16603 = VERTEX_POINT ( 'NONE', #42126 ) ;
#16604 = CARTESIAN_POINT ( 'NONE',  ( 745.7194118038753459, -397.6454272087885329, -348.7631598425976449 ) ) ;
#16605 = AXIS2_PLACEMENT_3D ( 'NONE', #39083, #32378, #25189 ) ;
#16607 = CARTESIAN_POINT ( 'NONE',  ( 813.2346286133761168, -269.2601417444139997, 328.9521613784389160 ) ) ;
#16606 = CARTESIAN_POINT ( 'NONE',  ( 747.2067596250078623, -339.1800572038740142, 352.2312462859687230 ) ) ;
#16608 = CARTESIAN_POINT ( 'NONE',  ( 769.9779781133707957, -235.0999726633344835, -316.7813123517150871 ) ) ;
#16609 = CARTESIAN_POINT ( 'NONE',  ( 800.2193346964447755, -210.9982390220561967, -355.1360043628815788 ) ) ;
#16610 = CARTESIAN_POINT ( 'NONE',  ( 803.4237431249931660, -423.1800572038737300, -331.2633955100225194 ) ) ;
#16611 = CARTESIAN_POINT ( 'NONE',  ( 758.0580252608178853, -222.4527844766016642, 328.0187753319985404 ) ) ;
#16612 = ORIENTED_EDGE ( 'NONE', *, *, #9654, .F. ) ;
#16613 = CARTESIAN_POINT ( 'NONE',  ( 812.7932403749906598, -351.1800572038740142, 327.7687537140311633 ) ) ;
#16614 = CIRCLE ( 'NONE', #27684, 30.00000000000002842 ) ;
#16615 = CARTESIAN_POINT ( 'NONE',  ( 791.0733055594794223, 17.05262341476191068, -312.1184307474205184 ) ) ;
#16616 = CARTESIAN_POINT ( 'NONE',  ( 794.4892657455289964, 16.45630643248850689, 314.6207049315058271 ) ) ;
#16617 = DIRECTION ( 'NONE',  ( 0.000000000000000000, 0.000000000000000000, -1.000000000000000000 ) ) ;
#16618 = VECTOR ( 'NONE', #28751, 1000.000000000000000 ) ;
#16619 = CARTESIAN_POINT ( 'NONE',  ( 769.9779781133707957, -211.0999726633346540, 316.7813123517150871 ) ) ;
#16620 = CARTESIAN_POINT ( 'NONE',  ( 788.7366044899766848, -83.90732993114754379, 316.5762568750059813 ) ) ;
#16621 = ORIENTED_EDGE ( 'NONE', *, *, #33179, .T. ) ;
#16622 = CARTESIAN_POINT ( 'NONE',  ( 811.3240766477731540, -460.3726999360611103, -355.6651683502462902 ) ) ;
#16623 = CARTESIAN_POINT ( 'NONE',  ( 751.6929314249750860, -78.99823902205665149, -318.8095938919659034 ) ) ;
#16624 = CARTESIAN_POINT ( 'NONE',  ( 776.9566956441375396, -252.8965053807777394, 364.8461984189686405 ) ) ;
#16625 = CARTESIAN_POINT ( 'NONE',  ( 759.7806653035534055, -414.9982390220555430, -324.8639956371180801 ) ) ;
#16626 = CARTESIAN_POINT ( 'NONE',  ( 771.1735550268780344, -33.18005720387498769, -316.3353852180828198 ) ) ;
#16627 = CARTESIAN_POINT ( 'NONE',  ( 786.2694204179717872, -21.28179084515337749, 305.1769319972829067 ) ) ;
#16628 = CARTESIAN_POINT ( 'NONE',  ( -78.83651009197140525, 260.0000000000000568, -199.9999999999936051 ) ) ;
#16629 = CARTESIAN_POINT ( 'NONE',  ( 766.9102291470427417, -282.5545181178798657, -318.6633372737382501 ) ) ;
#16630 = CARTESIAN_POINT ( 'NONE',  ( 782.5225473063381969, -190.2709662947835909, -375.2698199232970637 ) ) ;
#16631 = CARTESIAN_POINT ( 'NONE',  ( 751.9810565676468741, -98.08914811296568814, 360.9747183278973921 ) ) ;
#16632 = CARTESIAN_POINT ( 'NONE',  ( 782.4968714119720516, -154.8164208402382371, 305.0891759886411023 ) ) ;
#16633 = DIRECTION ( 'NONE',  ( 0.000000000000000000, 0.000000000000000000, 1.000000000000000000 ) ) ;
#16634 = CIRCLE ( 'NONE', #3352, 2.749999999999835687 ) ;
#16635 = CARTESIAN_POINT ( 'NONE',  ( 998.9999999999992042, 249.9999999999998863, -360.0000000000000000 ) ) ;
#16636 = CARTESIAN_POINT ( 'NONE',  ( 815.0009284576459549, -246.3510508353232638, -338.7629533639073429 ) ) ;
#16637 = CARTESIAN_POINT ( 'NONE',  ( 778.7629533639073998, -416.7363362996975980, 375.0009284576466371 ) ) ;
#16638 = CARTESIAN_POINT ( 'NONE',  ( 801.1904061080336987, -284.0891481129650629, -368.3070685750235498 ) ) ;
#16639 = CARTESIAN_POINT ( 'NONE',  ( -786.4999999999993179, -513.1383975375929367, -369.9999999999999432 ) ) ;
#16640 = CARTESIAN_POINT ( 'NONE',  ( 772.4837098697144029, -383.3618753856921444, 374.5518280994205611 ) ) ;
#16641 = CARTESIAN_POINT ( 'NONE',  ( 749.2812353651451076, -6.452784476602343666, 323.2262854647983090 ) ) ;
#16642 = CARTESIAN_POINT ( 'NONE',  ( 781.7834795799800531, -346.8164208402376971, -315.0636971347436202 ) ) ;
#16643 = CARTESIAN_POINT ( 'NONE',  ( 800.7704444035546203, -28.16923265350574468, 326.0291762391768771 ) ) ;
#16644 = CARTESIAN_POINT ( 'NONE',  ( 785.3141322388236176, -189.7255117493290300, -364.4286716492789537 ) ) ;
#16645 = CARTESIAN_POINT ( 'NONE',  ( 813.2346286133761168, -53.26014174441475291, -328.9521613784389160 ) ) ;
#16646 = CARTESIAN_POINT ( 'NONE',  ( 770.0799878456142551, -157.9874144716871456, -362.9823548866085616 ) ) ;
#16647 = CARTESIAN_POINT ( 'NONE',  ( 744.8212110874229666, -162.8965053807780521, 336.2046728542121627 ) ) ;
#16648 = CARTESIAN_POINT ( 'NONE',  ( 797.6776695296629214, 4.456306432488530866, 357.6776695296636603 ) ) ;
#16649 = AXIS2_PLACEMENT_3D ( 'NONE', #31469, #29546, #24759 ) ;
#16650 = ORIENTED_EDGE ( 'NONE', *, *, #39938, .T. ) ;
#16651 = CARTESIAN_POINT ( 'NONE',  ( 755.5713283507202505, -53.36187538569310362, -334.6858677611754729 ) ) ;
#16652 = CARTESIAN_POINT ( 'NONE',  ( 802.7791456095903868, -172.7146871989598083, -329.0155153010375102 ) ) ;
#16653 = CARTESIAN_POINT ( 'NONE',  ( 801.9419747391806368, -162.4527844766018632, 351.9812246680014027 ) ) ;
#16654 = AXIS2_PLACEMENT_3D ( 'NONE', #18608, #43312, #10763 ) ;
#16655 = CARTESIAN_POINT ( 'NONE',  ( 761.9338519418445230, -14.53286901714214707, -370.4231160770881957 ) ) ;
#16657 = CARTESIAN_POINT ( 'NONE',  ( 803.4237431249931660, -303.1800572038740711, 331.2633955100225194 ) ) ;
#16656 = CARTESIAN_POINT ( 'NONE',  ( 800.2193346964447755, -282.9982390220558841, 355.1360043628815788 ) ) ;
#16658 = PLANE ( 'NONE',  #22729 ) ;
#16659 = VERTEX_POINT ( 'NONE', #24797 ) ;
#16660 = CARTESIAN_POINT ( 'NONE',  ( 766.7756240680305382, -14.53286901714214707, 361.5560724626415663 ) ) ;
#16661 = CARTESIAN_POINT ( 'NONE',  ( 764.1737431748507561, -274.3726999360617356, -371.6461892240376415 ) ) ;
#16662 = PRODUCT_CONTEXT ( 'NONE', #20748, 'mechanical' ) ;
#16663 = CARTESIAN_POINT ( 'NONE',  ( 792.3570229623691148, -213.1800572038743837, 373.1304606946836770 ) ) ;
#16664 = CARTESIAN_POINT ( 'NONE',  ( 783.0745993439762742, -320.1908817542434349, 365.1016975059196739 ) ) ;
#16665 = CARTESIAN_POINT ( 'NONE',  ( 765.8855110935204493, -430.1692326535043094, 319.0159684113471599 ) ) ;
#16666 = ORIENTED_EDGE ( 'NONE', *, *, #16214, .T. ) ;
#16667 = CARTESIAN_POINT ( 'NONE',  ( 804.6971507214547046, -99.28179084515313946, -344.0799538623459739 ) ) ;
#16668 = CARTESIAN_POINT ( 'NONE',  ( 778.1981804954714335, -130.2709662947837899, -314.8072714833589885 ) ) ;
#16669 = CARTESIAN_POINT ( 'NONE',  ( 755.0636971347428243, -316.2709662947832499, -341.7834795799807353 ) ) ;
#16670 = VERTEX_POINT ( 'NONE', #35196 ) ;
#16671 = CARTESIAN_POINT ( 'NONE',  ( 795.1360043628807261, -428.0891481129644944, -360.2193346964456282 ) ) ;
#16672 = CIRCLE ( 'NONE', #38104, 4.999999999999982236 ) ;
#16673 = CARTESIAN_POINT ( 'NONE',  ( 755.8398074228967971, -283.4419599262321867, 333.4516893846970333 ) ) ;
#16674 = DIRECTION ( 'NONE',  ( 0.000000000000000000, -0.6594541114781790059, -0.7517448203044204691 ) ) ;
#16675 = CIRCLE ( 'NONE', #29951, 19.99999999999990763 ) ;
#16676 = LINE ( 'NONE', #27292, #30758 ) ;
#16677 = CARTESIAN_POINT ( 'NONE',  ( 796.9571628226829034, -119.4636090269712554, 321.2382568024804641 ) ) ;
#16678 = ORIENTED_EDGE ( 'NONE', *, *, #41635, .T. ) ;
#16679 = CARTESIAN_POINT ( 'NONE',  ( 815.3608509340175488, -338.7363362996978822, -341.2497674668889545 ) ) ;
#16680 = EDGE_CURVE ( 'NONE', #17388, #2565, #44917, .T. ) ;
#16681 = CIRCLE ( 'NONE', #21858, 10.00000000000000888 ) ;
#16682 = CARTESIAN_POINT ( 'NONE',  ( 759.7806653035534055, -318.9982390220557704, -324.8639956371180801 ) ) ;
#16683 = LINE ( 'NONE', #41853, #31836 ) ;
#16684 = CARTESIAN_POINT ( 'NONE',  ( 801.5560724626406000, -192.5545181178801215, -326.7756240680316182 ) ) ;
#16685 = AXIS2_PLACEMENT_3D ( 'NONE', #29353, #15027, #11568 ) ;
#16686 = CARTESIAN_POINT ( 'NONE',  ( 804.7487373415286811, -43.54369356751131903, 364.7487373415288516 ) ) ;
#16687 = CARTESIAN_POINT ( 'NONE',  ( 927.9999999999992042, 154.9999999999998863, 360.0000000000000000 ) ) ;
#16688 = CARTESIAN_POINT ( 'NONE',  ( 749.2812353651451076, -390.4527844766011526, -323.2262854647983090 ) ) ;
#16689 = CARTESIAN_POINT ( 'NONE',  ( 779.9999999999992042, 166.4563064324884465, 339.9999999999999432 ) ) ;
#16690 = CARTESIAN_POINT ( 'NONE',  ( 746.4236121716829757, -327.8272453906069472, 328.8385539511384650 ) ) ;
#16691 = LINE ( 'NONE', #41401, #29412 ) ;
#16692 = CARTESIAN_POINT ( 'NONE',  ( 767.7687537140311633, -287.9073299311468759, 372.7932403749916830 ) ) ;
#16693 = CARTESIAN_POINT ( 'NONE',  ( 814.2001403089898304, -17.36187538569322086, -347.4397851343538264 ) ) ;
#16694 = CARTESIAN_POINT ( 'NONE',  ( 791.9812246680005501, -260.6346026584197375, -361.9419747391813189 ) ) ;
#16695 = PLANE ( 'NONE',  #42409 ) ;
#16696 = MANIFOLD_SOLID_BREP ( 'Boss-Extrude23', #32822 ) ;
#16697 = CARTESIAN_POINT ( 'NONE',  ( 800.0135310231082713, -398.0891481129647218, 325.0180583372163028 ) ) ;
#16698 = CARTESIAN_POINT ( 'NONE',  ( 805.2837595273609850, -170.7363362996983938, 340.5290396650784714 ) ) ;
#16699 = CARTESIAN_POINT ( 'NONE',  ( 776.9566956441375396, -36.89650538077844288, -364.8461984189686405 ) ) ;
#16700 = CARTESIAN_POINT ( 'NONE',  ( 815.1787889125755555, -78.89650538077832209, 343.7953271457877804 ) ) ;
#16701 = CARTESIAN_POINT ( 'NONE',  ( 800.0135310231082713, -374.0891481129647786, 325.0180583372163028 ) ) ;
#16702 = CARTESIAN_POINT ( 'NONE',  ( 959.5497976682736407, 239.9999999999998863, -209.9999999999999716 ) ) ;
#16703 = CARTESIAN_POINT ( 'NONE',  ( 764.8639956371174549, -440.0891481129644944, 319.7806653035542013 ) ) ;
#16704 = VERTEX_POINT ( 'NONE', #11636 ) ;
#16705 = CARTESIAN_POINT ( 'NONE',  ( 797.8594530101008786, -61.54369356751124087, -322.1405469898980982 ) ) ;
#16706 = AXIS2_PLACEMENT_3D ( 'NONE', #21550, #7260, #33475 ) ;
#16707 = CARTESIAN_POINT ( 'NONE',  ( 757.2208543904082489, -352.7146871989593251, -350.9844846989624330 ) ) ;
#16709 = CARTESIAN_POINT ( 'NONE',  ( 788.7366044899766848, -179.9073299311472454, 316.5762568750059813 ) ) ;
#16708 = CARTESIAN_POINT ( 'NONE',  ( 756.3353852180819104, -197.9073299311472169, 331.1735550268788302 ) ) ;
#16710 = CARTESIAN_POINT ( 'NONE',  ( 744.8212110874229666, -378.8965053807772847, -336.2046728542121627 ) ) ;
#16711 = PLANE ( 'NONE',  #15339 ) ;
#16712 = EDGE_LOOP ( 'NONE', ( #3014, #32456, #32513, #1607 ) ) ;
#16713 = CARTESIAN_POINT ( 'NONE',  ( 759.7806653035534055, -390.9982390220557136, 324.8639956371180801 ) ) ;
#16714 = ORIENTED_EDGE ( 'NONE', *, *, #45007, .T. ) ;
#16715 = DIRECTION ( 'NONE',  ( -1.000000000000000000, 4.147566128926370535E-16, -0.000000000000000000 ) ) ;
#16716 = CIRCLE ( 'NONE', #28523, 10.00000000000000888 ) ;
#16717 = CARTESIAN_POINT ( 'NONE',  ( 782.5225473063381969, -214.2709662947834488, -375.2698199232970637 ) ) ;
#16718 = CARTESIAN_POINT ( 'NONE',  ( 747.2067596250078623, -123.1800572038747106, 352.2312462859687230 ) ) ;
#16719 = ORIENTED_EDGE ( 'NONE', *, *, #6040, .F. ) ;
#16720 = CARTESIAN_POINT ( 'NONE',  ( 802.1676090361155502, -206.6346026584198796, -327.8955696845344505 ) ) ;
#16721 = VERTEX_POINT ( 'NONE', #29415 ) ;
#16722 = CARTESIAN_POINT ( 'NONE',  ( 804.9363028652555840, -328.2709662947831362, -338.2165204200192079 ) ) ;
#16723 = CARTESIAN_POINT ( 'NONE',  ( 804.6971507214547046, -459.2817908451519884, -344.0799538623459739 ) ) ;
#16724 = CARTESIAN_POINT ( 'NONE',  ( 755.0488828828309806, -185.8055962898689302, 344.1219089521771934 ) ) ;
#16726 = CARTESIAN_POINT ( 'NONE',  ( 767.9999999999992042, 205.0000000000000568, 350.0000000000000000 ) ) ;
#16725 = CARTESIAN_POINT ( 'NONE',  ( 809.7763221938408833, -453.1000272243879863, 336.1997354883953903 ) ) ;
#16727 = EDGE_CURVE ( 'NONE', #6488, #12356, #41447, .T. ) ;
#16728 = DIRECTION ( 'NONE',  ( -0.000000000000000000, 1.000000000000000000, -0.000000000000000000 ) ) ;
#16729 = ORIENTED_EDGE ( 'NONE', *, *, #21338, .F. ) ;
#16730 = CARTESIAN_POINT ( 'NONE',  ( 761.4292242960306112, -449.4636090269702322, -323.2154366446414429 ) ) ;
#16731 = DIRECTION ( 'NONE',  ( 0.000000000000000000, -1.000000000000000000, 0.000000000000000000 ) ) ;
#16732 = DIRECTION ( 'NONE',  ( 0.000000000000000000, -1.000000000000000000, 1.110223024625155554E-15 ) ) ;
#16733 = EDGE_LOOP ( 'NONE', ( #1145, #35864, #35603, #4955 ) ) ;
#16734 = CARTESIAN_POINT ( 'NONE',  ( 755.8990559732751535, -251.4636090269709143, -365.9055244015606831 ) ) ;
#16735 = CARTESIAN_POINT ( 'NONE',  ( 745.1792804349281596, -86.19088175424408860, 343.7566961878542884 ) ) ;
#16737 = CARTESIAN_POINT ( 'NONE',  ( 762.3223304703356007, -223.5436935675107577, -322.3223304703362828 ) ) ;
#16736 = DIRECTION ( 'NONE',  ( -0.000000000000000000, 1.000000000000000000, -0.000000000000000000 ) ) ;
#16738 = CARTESIAN_POINT ( 'NONE',  ( 799.4546378042377910, -369.0783235625956422, -356.1575198192848006 ) ) ;
#16739 = CARTESIAN_POINT ( 'NONE',  ( 797.8822607201568644, -246.5545181178799510, -370.1134526219340160 ) ) ;
#16740 = CARTESIAN_POINT ( 'NONE',  ( 911.9999999999993179, 219.9999999999998863, -360.0000000000000000 ) ) ;
#16741 = CARTESIAN_POINT ( 'NONE',  ( 939.9999999999992042, 240.0000000000000568, 201.9999999999999716 ) ) ;
#16742 = CARTESIAN_POINT ( 'NONE',  ( 754.7162404726377645, -86.73633629969862113, -339.4709603349214717 ) ) ;
#16743 = AXIS2_PLACEMENT_3D ( 'NONE', #29730, #43808, #40385 ) ;
#16744 = CARTESIAN_POINT ( 'NONE',  ( 769.9779781133707957, -427.0999726633338582, 316.7813123517150871 ) ) ;
#16745 = AXIS2_PLACEMENT_3D ( 'NONE', #27186, #41276, #44045 ) ;
#16746 = FACE_OUTER_BOUND ( 'NONE', #44254, .T. ) ;
#16747 = CARTESIAN_POINT ( 'NONE',  ( 782.5225473063383106, -286.2709662947833067, -375.2698199232970637 ) ) ;
#16748 = CARTESIAN_POINT ( 'NONE',  ( 939.9999999999993179, -600.0000000000001137, -360.0000000000000000 ) ) ;
#16749 = PLANE ( 'NONE',  #38659 ) ;
#16750 = CARTESIAN_POINT ( 'NONE',  ( 756.5762568750052424, -51.18005720387493085, -348.7366044899774238 ) ) ;
#16751 = VECTOR ( 'NONE', #10188, 1000.000000000000000 ) ;
#16752 = CARTESIAN_POINT ( 'NONE',  ( 752.7379699480933368, -204.0090635724255606, 361.9858362298580232 ) ) ;
#16753 = CARTESIAN_POINT ( 'NONE',  ( 813.9316612368132837, -175.4419599262325562, -348.6739635108323228 ) ) ;
#16754 = CARTESIAN_POINT ( 'NONE',  ( 744.7301800767019131, -196.8164208402380950, 337.4774526936615757 ) ) ;
#16755 = CARTESIAN_POINT ( 'NONE',  ( 796.7737145352015204, -404.6346026584193396, -370.7187646348536987 ) ) ;
#16756 = VECTOR ( 'NONE', #18615, 1000.000000000000000 ) ;
#16757 = CARTESIAN_POINT ( 'NONE',  ( 799.9999999999993179, -462.9681489794448339, 370.0000000000000568 ) ) ;
#16758 = CARTESIAN_POINT ( 'NONE',  ( 765.0180583372156207, -288.9982390220559978, 360.0135310231089534 ) ) ;
#16759 = CARTESIAN_POINT ( 'NONE',  ( 783.0745993439762742, -56.19088175424417386, 365.1016975059196739 ) ) ;
#16760 = CARTESIAN_POINT ( 'NONE',  ( 759.9864689768902508, -434.0891481129646081, -354.9819416627836404 ) ) ;
#16761 = PLANE ( 'NONE',  #27655 ) ;
#16762 = PLANE ( 'NONE',  #12200 ) ;
#16764 = CARTESIAN_POINT ( 'NONE',  ( 762.1405469898971887, -313.5436935675102745, 357.8594530101015607 ) ) ;
#16763 = CARTESIAN_POINT ( 'NONE',  ( 779.4709603349208464, -72.35105083532378956, 314.7162404726379918 ) ) ;
#16765 = ORIENTED_EDGE ( 'NONE', *, *, #13105, .T. ) ;
#16766 = CARTESIAN_POINT ( 'NONE',  ( 784.0799538623451781, -275.8055962898685038, -364.6971507214555572 ) ) ;
#16767 = CARTESIAN_POINT ( 'NONE',  ( 754.8072714833581358, -124.8164208402383508, -338.1981804954720587 ) ) ;
#16768 = CARTESIAN_POINT ( 'NONE',  ( 759.7806653035534055, -54.99823902205672255, 324.8639956371180801 ) ) ;
#16769 = CARTESIAN_POINT ( 'NONE',  ( 810.1134526219336749, -248.5328690171414223, -357.8822607201570349 ) ) ;
#16770 = CARTESIAN_POINT ( 'NONE',  ( 914.9999999999992042, 99.99999999999984368, -350.0000000000000000 ) ) ;
#16771 = CARTESIAN_POINT ( 'NONE',  ( 746.7653713866222915, -377.2601417444137724, 351.0478386215610271 ) ) ;
#16772 = ORIENTED_EDGE ( 'NONE', *, *, #29199, .T. ) ;
#16773 = AXIS2_PLACEMENT_3D ( 'NONE', #13051, #2187, #26889 ) ;
#16774 = CARTESIAN_POINT ( 'NONE',  ( 805.1927285166397041, -280.8164208402378677, 341.8018195045277707 ) ) ;
#16775 = CARTESIAN_POINT ( 'NONE',  ( 772.4837098697144029, 0.6381246143067236254, 374.5518280994205611 ) ) ;
#16776 = CARTESIAN_POINT ( 'NONE',  ( 795.9930595647434757, -27.07832356259665474, -320.7433823573372820 ) ) ;
#16777 = CARTESIAN_POINT ( 'NONE',  ( 758.0580252608178853, -174.4527844766018063, -328.0187753319985404 ) ) ;
#16778 = CARTESIAN_POINT ( 'NONE',  ( 762.1405469898971887, -385.5436935675102745, 357.8594530101015607 ) ) ;
#16779 = EDGE_CURVE ( 'NONE', #45456, #2619, #8171, .T. ) ;
#16780 = CARTESIAN_POINT ( 'NONE',  ( 813.1304606946830518, -113.9073299311474301, -352.3570229623690580 ) ) ;
#16781 = CARTESIAN_POINT ( 'NONE',  ( 771.1735550268780344, -105.1800572038747390, -316.3353852180828198 ) ) ;
#16782 = VERTEX_POINT ( 'NONE', #18113 ) ;
#16783 = CARTESIAN_POINT ( 'NONE',  ( 786.5483106153019435, -55.64542720878963422, -364.1601925771022366 ) ) ;
#16784 = AXIS2_PLACEMENT_3D ( 'NONE', #8194, #7514, #7981 ) ;
#16785 = CARTESIAN_POINT ( 'NONE',  ( 801.5560724626406000, -360.5545181178796383, -326.7756240680316182 ) ) ;
#16787 = CARTESIAN_POINT ( 'NONE',  ( 799.2566176426618085, -408.0090635724249069, 324.0069404352559559 ) ) ;
#16786 = CARTESIAN_POINT ( 'NONE',  ( 754.8072714833581358, -76.81642084023845030, 338.1981804954720587 ) ) ;
#16790 = CARTESIAN_POINT ( 'NONE',  ( 793.4146539503750546, -361.9874144716864635, 307.6481478633938877 ) ) ;
#16789 = PLANE ( 'NONE',  #44657 ) ;
#16788 = CARTESIAN_POINT ( 'NONE',  ( 804.7487373415286811, -451.5436935675099903, 364.7487373415288516 ) ) ;
#16791 = EDGE_CURVE ( 'NONE', #13142, #15014, #1658, .T. ) ;
#16792 = CARTESIAN_POINT ( 'NONE',  ( 773.7943932421234194, -119.8055962898690865, 305.5313806188329409 ) ) ;
#16793 = CARTESIAN_POINT ( 'NONE',  ( 766.9102291470427417, -354.5545181178796383, -318.6633372737382501 ) ) ;
#16794 = CARTESIAN_POINT ( 'NONE',  ( 778.1981804954714335, -370.2709662947831362, -314.8072714833589885 ) ) ;
#16795 = CARTESIAN_POINT ( 'NONE',  ( 810.4231160770870019, -120.5545181178803205, -321.9338519418446936 ) ) ;
#16796 = CARTESIAN_POINT ( 'NONE',  ( 755.8990559732751535, -11.46360902697159290, 365.9055244015606831 ) ) ;
#16798 = CARTESIAN_POINT ( 'NONE',  ( 181.1634899080285948, 260.0000000000000000, -193.8809999999953959 ) ) ;
#16797 = DIRECTION ( 'NONE',  ( -0.000000000000000000, 1.000000000000000000, -0.000000000000000000 ) ) ;
#16799 = CARTESIAN_POINT ( 'NONE',  ( 755.8990559732751535, -155.4636090269711417, -365.9055244015606831 ) ) ;
#16800 = DIRECTION ( 'NONE',  ( -0.000000000000000000, -0.000000000000000000, 1.000000000000000000 ) ) ;
#16801 = CARTESIAN_POINT ( 'NONE',  ( 914.9999999999992042, 99.99999999999984368, 360.0000000000000000 ) ) ;
#16802 = CARTESIAN_POINT ( 'NONE',  ( 804.1105419155481968, -339.8272453906069472, 347.6308680596136469 ) ) ;
#16803 = ORIENTED_EDGE ( 'NONE', *, *, #23804, .F. ) ;
#16804 = CARTESIAN_POINT ( 'NONE',  ( 812.3518521366052028, -313.0999726633342561, 326.5853460496235243 ) ) ;
#16805 = CARTESIAN_POINT ( 'NONE',  ( 796.9462024416508257, -156.4527844766018916, -308.9653473494370246 ) ) ;
#16806 = ADVANCED_FACE ( 'NONE', ( #39599, #21790 ), #42814, .F. ) ;
#16807 = DIRECTION ( 'NONE',  ( 1.000000000000000000, -0.000000000000000000, -0.000000000000000000 ) ) ;
#16808 = CARTESIAN_POINT ( 'NONE',  ( 802.2119215644370342, -126.0090635724257737, 367.5423716828165084 ) ) ;
#16809 = EDGE_CURVE ( 'NONE', #1277, #15686, #22458, .T. ) ;
#16810 = CARTESIAN_POINT ( 'NONE',  ( 792.2312462859673587, -299.9073299311468759, -307.2067596250082602 ) ) ;
#16811 = CARTESIAN_POINT ( 'NONE',  ( 779.9999999999992042, 16.45630643248849267, -339.9999999999999432 ) ) ;
#16812 = CARTESIAN_POINT ( 'NONE',  ( 701.1634899080286232, 259.9999999999999432, -199.9999999999990337 ) ) ;
#16813 = ADVANCED_FACE ( 'NONE', ( #32650 ), #11853, .F. ) ;
#16814 = CARTESIAN_POINT ( 'NONE',  ( 804.6798772138708955, -135.7255117493291152, 334.6312213355107019 ) ) ;
#16815 = ORIENTED_EDGE ( 'NONE', *, *, #33150, .T. ) ;
#16816 = CARTESIAN_POINT ( 'NONE',  ( 746.4236121716829757, -423.8272453906067199, 328.8385539511384650 ) ) ;
#16817 = CARTESIAN_POINT ( 'NONE',  ( 814.8230680027162407, -365.8055962898682765, -333.7305795820267917 ) ) ;
#16818 = VECTOR ( 'NONE', #34236, 1000.000000000000114 ) ;
#16819 = CARTESIAN_POINT ( 'NONE',  ( 745.7998596910086917, -125.3618753856928834, -332.5602148656461168 ) ) ;
#16820 = CARTESIAN_POINT ( 'NONE',  ( 757.0176451133909268, -61.09997266333506616, 349.9200121543848354 ) ) ;
#16821 = CARTESIAN_POINT ( 'NONE',  ( 763.0537975583475827, -384.4527844766011526, -371.0346526505627480 ) ) ;
#16822 = DIRECTION ( 'NONE',  ( -1.000000000000000000, -0.000000000000000000, -0.000000000000000000 ) ) ;
#16823 = CARTESIAN_POINT ( 'NONE',  ( 789.6640940660590786, -442.9180389616178672, 363.1300863558843162 ) ) ;
#16824 = ORIENTED_EDGE ( 'NONE', *, *, #13339, .F. ) ;
#16825 = CARTESIAN_POINT ( 'NONE',  ( 783.7566961878529810, -144.8965053807781089, -305.1792804349288417 ) ) ;
#16826 = CARTESIAN_POINT ( 'NONE',  ( 799.9999999999993179, 205.0000000000000568, 339.9999999999999432 ) ) ;
#16827 = CARTESIAN_POINT ( 'NONE',  ( 747.3154664389472828, -283.9874144716867477, 326.4474001241230781 ) ) ;
#16828 = CARTESIAN_POINT ( 'NONE',  ( 755.5713283507202505, -77.36187538569302546, 334.6858677611754729 ) ) ;
#16829 = EDGE_LOOP ( 'NONE', ( #14407, #23160, #15345, #1921 ) ) ;
#16830 = ADVANCED_FACE ( 'NONE', ( #35884, #32193 ), #7954, .T. ) ;
#16831 = CARTESIAN_POINT ( 'NONE',  ( 759.2295555964440155, -16.16923265350578021, -353.9708237608231229 ) ) ;
#16832 = CARTESIAN_POINT ( 'NONE',  ( 803.6646147819161570, -257.9073299311469896, 348.8264449731210561 ) ) ;
#16833 = EDGE_CURVE ( 'NONE', #14734, #5955, #15331, .T. ) ;
#16834 = CARTESIAN_POINT ( 'NONE',  ( 808.0189434323515343, -14.08914811296595460, -319.0252816721025511 ) ) ;
#16835 = LINE ( 'NONE', #34127, #23910 ) ;
#16836 = VERTEX_POINT ( 'NONE', #31944 ) ;
#16837 = ORIENTED_EDGE ( 'NONE', *, *, #35586, .T. ) ;
#16838 = CARTESIAN_POINT ( 'NONE',  ( 800.2193346964447755, -186.9982390220563104, -355.1360043628815788 ) ) ;
#16839 = CARTESIAN_POINT ( 'NONE',  ( 748.6759233522253680, -400.3726999360612808, -324.3348316497537098 ) ) ;
#16840 = CARTESIAN_POINT ( 'NONE',  ( 801.9419747391806368, -258.4527844766016074, -351.9812246680014027 ) ) ;
#16842 = CARTESIAN_POINT ( 'NONE',  ( 759.8311093483677041, -262.1692326535049347, 310.9282345327691814 ) ) ;
#16841 = CARTESIAN_POINT ( 'NONE',  ( 745.0891759886404770, -364.2709662947830793, 342.4968714119734159 ) ) ;
#16843 = CARTESIAN_POINT ( 'NONE',  ( 755.3028492785439312, -255.2817908451526705, -335.9200461376539693 ) ) ;
#16844 = CARTESIAN_POINT ( 'NONE',  ( 756.3353852180819104, -221.9073299311470464, -331.1735550268788302 ) ) ;
#16845 = CARTESIAN_POINT ( 'NONE',  ( 800.2193346964446619, -402.9982390220555999, -355.1360043628816925 ) ) ;
#16846 = CARTESIAN_POINT ( 'NONE',  ( 759.9864689768902508, -242.0891481129652618, 354.9819416627836404 ) ) ;
#16847 = EDGE_LOOP ( 'NONE', ( #23409, #9083, #4343, #5870 ) ) ;
#16848 = VECTOR ( 'NONE', #4539, 1000.000000000000000 ) ;
#16849 = CARTESIAN_POINT ( 'NONE',  ( 796.9462024416508257, -348.4527844766012663, 308.9653473494370246 ) ) ;
#16850 = DIRECTION ( 'NONE',  ( 1.880165489482579047E-16, 1.000000000000000000, 0.000000000000000000 ) ) ;
#16851 = CARTESIAN_POINT ( 'NONE',  ( 745.7194118038753459, -61.64542720878961291, -348.7631598425976449 ) ) ;
#16852 = CARTESIAN_POINT ( 'NONE',  ( 789.5497161195852414, 16.45630643248838609, 314.2297168413928148 ) ) ;
#16853 = CARTESIAN_POINT ( 'NONE',  ( 879.9999999999992042, 239.9999999999998863, -219.9999999999999716 ) ) ;
#16854 = CARTESIAN_POINT ( 'NONE',  ( 790.9844846989617508, -238.3726999360617640, 317.2208543904092721 ) ) ;
#16855 = CARTESIAN_POINT ( 'NONE',  ( 785.3687786644884454, -131.3618753856928834, 315.3201227861279676 ) ) ;
#16856 = ORIENTED_EDGE ( 'NONE', *, *, #38277, .T. ) ;
#16857 = CARTESIAN_POINT ( 'NONE',  ( 796.9571628226829034, -23.46360902697155026, -321.2382568024804641 ) ) ;
#16858 = CARTESIAN_POINT ( 'NONE',  ( 813.1304606946831655, -65.90732993114760063, -352.3570229623691716 ) ) ;
#16859 = CARTESIAN_POINT ( 'NONE',  ( 775.9200461376533440, -287.8055962898685038, 315.3028492785443291 ) ) ;
#16860 = CARTESIAN_POINT ( 'NONE',  ( 759.7806653035534055, -438.9982390220553157, -324.8639956371180801 ) ) ;
#16861 = CARTESIAN_POINT ( 'NONE',  ( 764.8639956371174549, -32.08914811296589420, -319.7806653035542581 ) ) ;
#16862 = CARTESIAN_POINT ( 'NONE',  ( 801.1904061080336987, -452.0891481129646650, 368.3070685750235498 ) ) ;
#16863 = CARTESIAN_POINT ( 'NONE',  ( 744.7301800767019131, -196.8164208402380950, -337.4774526936615757 ) ) ;
#16864 = CARTESIAN_POINT ( 'NONE',  ( 759.0252816721024374, -72.99823902205667991, 368.0189434323527280 ) ) ;
#16865 = CARTESIAN_POINT ( 'NONE',  ( 796.7737145352015204, -188.6346026584199365, 370.7187646348536987 ) ) ;
#16866 = LINE ( 'NONE', #34157, #15131 ) ;
#16867 = DIRECTION ( 'NONE',  ( 1.000000000000000000, 0.000000000000000000, 0.000000000000000000 ) ) ;
#16868 = CARTESIAN_POINT ( 'NONE',  ( 759.8311093483677041, -262.1692326535049347, -310.9282345327691814 ) ) ;
#16869 = CARTESIAN_POINT ( 'NONE',  ( 799.9636004259356241, -406.9181544815157849, 311.2241431872006956 ) ) ;
#16870 = CARTESIAN_POINT ( 'NONE',  ( 808.0189434323515343, -278.0891481129651197, -319.0252816721025511 ) ) ;
#16871 = CYLINDRICAL_SURFACE ( 'NONE', #12481, 10.00000000000000888 ) ;
#16872 = CARTESIAN_POINT ( 'NONE',  ( 787.4397851343537695, -381.7255117493284615, 374.2001403089903988 ) ) ;
#16873 = CARTESIAN_POINT ( 'NONE',  ( 808.3070685750232087, -18.99823902205684689, 361.1904061080339829 ) ) ;
#16874 = CARTESIAN_POINT ( 'NONE',  ( 800.0135310231082713, -350.0891481129648923, -325.0180583372163028 ) ) ;
#16875 = CARTESIAN_POINT ( 'NONE',  ( 804.1601925771018387, -31.44195992623299674, 346.5483106153029098 ) ) ;
#16876 = CARTESIAN_POINT ( 'NONE',  ( 771.2368401574024119, -61.44195992623291147, -374.2805881961240857 ) ) ;
#16877 = CARTESIAN_POINT ( 'NONE',  ( 754.8983024940795303, -162.8965053807780521, -336.9254006560228163 ) ) ;
#16878 = CARTESIAN_POINT ( 'NONE',  ( 745.1769319972822814, -161.8055962898689870, 346.2694204179732083 ) ) ;
#16879 = CARTESIAN_POINT ( 'NONE',  ( 879.9999999999990905, 479.9999999999998863, 199.9999999999999716 ) ) ;
#16880 = CARTESIAN_POINT ( 'NONE',  ( 754.0944755984390895, -183.6237781080507148, 364.1009440267246760 ) ) ;
#16881 = EDGE_LOOP ( 'NONE', ( #5694, #20625 ) ) ;
#16882 = CARTESIAN_POINT ( 'NONE',  ( 756.3353852180819104, -77.90732993114757221, -331.1735550268788302 ) ) ;
#16883 = CARTESIAN_POINT ( 'NONE',  ( 786.6156483768007774, -169.4419599262325562, -315.5913626894246136 ) ) ;
#16884 = CARTESIAN_POINT ( 'NONE',  ( 767.8955696845333705, -168.4527844766018347, 362.1676090361162323 ) ) ;
#16885 = CARTESIAN_POINT ( 'NONE',  ( 759.8311093483677041, 1.830767346494167391, -310.9282345327691814 ) ) ;
#16887 = CARTESIAN_POINT ( 'NONE',  ( 759.7806653035535192, -294.9982390220559978, 324.8639956371181370 ) ) ;
#16886 = CARTESIAN_POINT ( 'NONE',  ( 764.8639956371174549, -296.0891481129650629, 319.7806653035542013 ) ) ;
#16888 = DIRECTION ( 'NONE',  ( 1.000000000000000000, 2.313994520913686024E-32, -2.750100768424433609E-32 ) ) ;
#16889 = ORIENTED_EDGE ( 'NONE', *, *, #45565, .T. ) ;
#16890 = CARTESIAN_POINT ( 'NONE',  ( 796.7845633553578182, -9.623778108051251223, 358.5707757039688204 ) ) ;
#16891 = CARTESIAN_POINT ( 'NONE',  ( 814.8207195650702488, -314.1908817542433781, -336.2433038121456548 ) ) ;
#16892 = CARTESIAN_POINT ( 'NONE',  ( 745.7998596910086917, -245.3618753856925139, 332.5602148656461168 ) ) ;
#16893 = CARTESIAN_POINT ( 'NONE',  ( 769.9779781133707957, -331.0999726633342561, 316.7813123517150871 ) ) ;
#16894 = CARTESIAN_POINT ( 'NONE',  ( 796.7845633553578182, -441.6237781080499190, 358.5707757039688204 ) ) ;
#16895 = CARTESIAN_POINT ( 'NONE',  ( 769.9779781133707957, -163.0999726633347677, -316.7813123517150871 ) ) ;
#16896 = CARTESIAN_POINT ( 'NONE',  ( 767.8955696845333705, -120.4527844766019484, -362.1676090361162323 ) ) ;
#16897 = CARTESIAN_POINT ( 'NONE',  ( 800.0135310231082713, -326.0891481129649492, -325.0180583372163028 ) ) ;
#16898 = ORIENTED_EDGE ( 'NONE', *, *, #13433, .T. ) ;
#16899 = CARTESIAN_POINT ( 'NONE',  ( 803.6646147819161570, -425.9073299311463074, -348.8264449731210561 ) ) ;
#16900 = CARTESIAN_POINT ( 'NONE',  ( 754.8983024940795303, -306.8965053807775689, 336.9254006560228163 ) ) ;
#16901 = LINE ( 'NONE', #3676, #21882 ) ;
#16902 = CARTESIAN_POINT ( 'NONE',  ( 8.295132257852746908E-14, 200.0000000000001421, 339.9999999999999432 ) ) ;
#16903 = CARTESIAN_POINT ( 'NONE',  ( 755.5913626894240451, -133.6454272087893571, 346.6156483768012890 ) ) ;
#16904 = CARTESIAN_POINT ( 'NONE',  ( 801.9419747391806368, 5.547215523397618142, 351.9812246680014027 ) ) ;
#16905 = ORIENTED_EDGE ( 'NONE', *, *, #2061, .T. ) ;
#16906 = CARTESIAN_POINT ( 'NONE',  ( 795.8262568251477660, -334.3726999360615082, -308.3538107759623585 ) ) ;
#16907 = CARTESIAN_POINT ( 'NONE',  ( 754.7162404726377645, -230.7363362996981664, 339.4709603349214717 ) ) ;
#16908 = CARTESIAN_POINT ( 'NONE',  ( 795.8262568251477660, -238.3726999360617640, 308.3538107759623585 ) ) ;
#16909 = VECTOR ( 'NONE', #3002, 1000.000000000000000 ) ;
#16910 = CARTESIAN_POINT ( 'NONE',  ( 781.8018195045266339, -310.2709662947832499, -365.1927285166406705 ) ) ;
#16911 = CARTESIAN_POINT ( 'NONE',  ( 181.1634899080285948, 256.5000000000000000, -206.1189999999954239 ) ) ;
#16912 = CARTESIAN_POINT ( 'NONE',  ( 754.7162404726377645, -182.7363362996983369, -339.4709603349214717 ) ) ;
#16913 = CARTESIAN_POINT ( 'NONE',  ( 772.5602148656447525, -57.72551174932945628, 305.7998596910095443 ) ) ;
#16914 = CARTESIAN_POINT ( 'NONE',  ( 809.4284809582966318, -452.9681489794448339, 335.2276976236387895 ) ) ;
#16915 = CARTESIAN_POINT ( 'NONE',  ( 777.5031285880264704, -382.8164208402374697, -374.9108240113588408 ) ) ;
#16916 = DIRECTION ( 'NONE',  ( 0.000000000000000000, 0.000000000000000000, -1.000000000000000000 ) ) ;
#16917 = CARTESIAN_POINT ( 'NONE',  ( 809.0717654672305343, -316.9181544815160692, 360.1688906516309885 ) ) ;
#16918 = CARTESIAN_POINT ( 'NONE',  ( 311.1634899080286232, 240.0000000000000000, -199.9999999999963336 ) ) ;
#16919 = CARTESIAN_POINT ( 'NONE',  ( 808.0189434323515343, -278.0891481129651197, 319.0252816721025511 ) ) ;
#16920 = CARTESIAN_POINT ( 'NONE',  ( 814.9108240113580450, -16.27096629478413092, -337.5031285880265273 ) ) ;
#16921 = CARTESIAN_POINT ( 'NONE',  ( 755.3201227861273992, -243.7255117493287742, -345.3687786644892981 ) ) ;
#16922 = CARTESIAN_POINT ( 'NONE',  ( -28.63011601220122415, -563.3203001761230553, -342.3463313526983143 ) ) ;
#16923 = CARTESIAN_POINT ( 'NONE',  ( 774.6858677611749044, -393.7255117493283478, 315.5713283507209894 ) ) ;
#16924 = CARTESIAN_POINT ( 'NONE',  ( 775.8780910478218402, -153.2817908451529831, 364.9511171171680530 ) ) ;
#16925 = CARTESIAN_POINT ( 'NONE',  ( 799.9636004259356241, -46.91815448151694312, -311.2241431872006956 ) ) ;
#16926 = CARTESIAN_POINT ( 'NONE',  ( 758.6633372737375112, -44.53286901714205470, -326.9102291470432533 ) ) ;
#16927 = CARTESIAN_POINT ( 'NONE',  ( 811.6461892240364477, -52.71468719896020616, 324.1737431748509835 ) ) ;
#16928 = CARTESIAN_POINT ( 'NONE',  ( 771.1735550268780344, -369.1800572038739006, 316.3353852180828198 ) ) ;
#16929 = LINE ( 'NONE', #16461, #23977 ) ;
#16930 = FACE_OUTER_BOUND ( 'NONE', #36707, .T. ) ;
#16931 = CARTESIAN_POINT ( 'NONE',  ( 747.3154664389472828, -139.9874144716872024, 326.4474001241230781 ) ) ;
#16932 = CARTESIAN_POINT ( 'NONE',  ( 756.3353852180819104, -413.9073299311465348, 331.1735550268788302 ) ) ;
#16933 = VERTEX_POINT ( 'NONE', #18790 ) ;
#16934 = CARTESIAN_POINT ( 'NONE',  ( 774.6312213355099630, -71.36187538569302546, -364.6798772138717482 ) ) ;
#16935 = CARTESIAN_POINT ( 'NONE',  ( 765.8855110935204493, -358.1692326535047641, -319.0159684113471599 ) ) ;
#16937 = CARTESIAN_POINT ( 'NONE',  ( 800.2193346964446619, -186.9982390220563104, 355.1360043628816925 ) ) ;
#16936 = CARTESIAN_POINT ( 'NONE',  ( 764.8639956371174549, -176.0891481129653755, 319.7806653035542013 ) ) ;
#16938 = CARTESIAN_POINT ( 'NONE',  ( 754.0944755984390895, -351.6237781080502032, -364.1009440267246760 ) ) ;
#16939 = CYLINDRICAL_SURFACE ( 'NONE', #25619, 1.000000000000000888 ) ;
#16940 = ORIENTED_EDGE ( 'NONE', *, *, #8086, .F. ) ;
#16941 = CARTESIAN_POINT ( 'NONE',  ( 804.9363028652555840, -400.2709662947828519, 338.2165204200192079 ) ) ;
#16942 = AXIS2_PLACEMENT_3D ( 'NONE', #24321, #6089, #41666 ) ;
#16943 = VERTEX_POINT ( 'NONE', #14419 ) ;
#16944 = CARTESIAN_POINT ( 'NONE',  ( 813.1304606946830518, -233.9073299311470180, -352.3570229623690580 ) ) ;
#16945 = CARTESIAN_POINT ( 'NONE',  ( 746.8695393053151292, -125.9073299311474159, 327.6429770376306578 ) ) ;
#16946 = ORIENTED_EDGE ( 'NONE', *, *, #15877, .F. ) ;
#16947 = CARTESIAN_POINT ( 'NONE',  ( 797.8594530101009923, -205.5436935675108145, -322.1405469898982119 ) ) ;
#16948 = ORIENTED_EDGE ( 'NONE', *, *, #18978, .T. ) ;
#16949 = CARTESIAN_POINT ( 'NONE',  ( 758.0580252608178853, -342.4527844766013231, -328.0187753319985404 ) ) ;
#16950 = CARTESIAN_POINT ( 'NONE',  ( 795.1360043628807261, 3.910851887033985896, -360.2193346964456282 ) ) ;
#16951 = CARTESIAN_POINT ( 'NONE',  ( 804.1601925771018387, -199.4419599262324709, 346.5483106153029098 ) ) ;
#16952 = CARTESIAN_POINT ( 'NONE',  ( -786.4999999999993179, -563.3203001761230553, -342.3463313526983143 ) ) ;
#16953 = DIRECTION ( 'NONE',  ( -1.880165489482579047E-16, -1.000000000000000000, -0.000000000000000000 ) ) ;
#16954 = VERTEX_POINT ( 'NONE', #993 ) ;
#16955 = CARTESIAN_POINT ( 'NONE',  ( 793.9708237608222134, -454.9181544815156713, -319.2295555964448681 ) ) ;
#16956 = DIRECTION ( 'NONE',  ( -1.000000000000000000, -0.000000000000000000, -0.000000000000000000 ) ) ;
#16957 = DIRECTION ( 'NONE',  ( -1.000000000000000000, -0.000000000000000000, -0.000000000000000000 ) ) ;
#16958 = EDGE_LOOP ( 'NONE', ( #38904, #16245 ) ) ;
#16959 = CARTESIAN_POINT ( 'NONE',  ( 781.2370466360911223, -236.7363362996981380, -304.9990715423533629 ) ) ;
#16960 = CARTESIAN_POINT ( 'NONE',  ( 781.2370466360911223, -140.7363362996984506, 304.9990715423533629 ) ) ;
#16962 = CARTESIAN_POINT ( 'NONE',  ( 785.3687786644884454, -227.3618753856925707, -315.3201227861279676 ) ) ;
#16961 = CARTESIAN_POINT ( 'NONE',  ( 799.9999999999993179, -512.9681489794448908, 309.9999999999998863 ) ) ;
#16963 = CARTESIAN_POINT ( 'NONE',  ( 775.9200461376533440, -383.8055962898682765, -315.3028492785443291 ) ) ;
#16964 = CARTESIAN_POINT ( 'NONE',  ( 809.0717654672305343, -244.9181544815162681, -360.1688906516309885 ) ) ;
#16965 = CYLINDRICAL_SURFACE ( 'NONE', #35583, 10.00000000000000888 ) ;
#16966 = DIRECTION ( 'NONE',  ( 1.000000000000000000, -1.892425610156518354E-16, 0.000000000000000000 ) ) ;
#16967 = CARTESIAN_POINT ( 'NONE',  ( 759.0159684113467620, -64.91815448151686496, -325.8855110935213020 ) ) ;
#16968 = CARTESIAN_POINT ( 'NONE',  ( 804.6971507214547046, -435.2817908451521021, 344.0799538623459739 ) ) ;
#16969 = CARTESIAN_POINT ( 'NONE',  ( 788.6739635108323228, -367.6454272087886466, 373.9316612368139090 ) ) ;
#16970 = CARTESIAN_POINT ( 'NONE',  ( -789.9999999999992042, 205.0000000000000568, -339.9999999999999432 ) ) ;
#16971 = CARTESIAN_POINT ( 'NONE',  ( 789.9200121543843807, -433.9874144716862361, -317.0176451133914384 ) ) ;
#16972 = CARTESIAN_POINT ( 'NONE',  ( 747.2067596250078623, -291.1800572038741848, -352.2312462859687230 ) ) ;
#16973 = CARTESIAN_POINT ( 'NONE',  ( -338.8365100919713200, 240.0000000000001421, -199.9999999999917861 ) ) ;
#16974 = CARTESIAN_POINT ( 'NONE',  ( 788.7366044899766848, 12.09267006885214180, 316.5762568750059813 ) ) ;
#16975 = CARTESIAN_POINT ( 'NONE',  ( 774.6312213355099630, -71.36187538569302546, -364.6798772138717482 ) ) ;
#16976 = CARTESIAN_POINT ( 'NONE',  ( 752.7379699480933368, -228.0090635724254753, 361.9858362298580232 ) ) ;
#16977 = CARTESIAN_POINT ( 'NONE',  ( 768.8385539511368734, -167.2601417444143976, -306.4236121716840557 ) ) ;
#16978 = CARTESIAN_POINT ( 'NONE',  ( 754.9967657858570647, -193.5436935675108714, 365.0032342141425374 ) ) ;
#16979 = CARTESIAN_POINT ( 'NONE',  ( 748.9653473494363425, -410.6346026584191122, -356.9462024416521331 ) ) ;
#16980 = CARTESIAN_POINT ( 'NONE',  ( 799.9999999999993179, -462.9681489794448339, -370.0000000000000568 ) ) ;
#16981 = CARTESIAN_POINT ( 'NONE',  ( 797.8594530101008786, -301.5436935675105588, 322.1405469898980982 ) ) ;
#16982 = CARTESIAN_POINT ( 'NONE',  ( 758.4439275373578084, -60.55451811788051941, 353.2243759319684386 ) ) ;
#16983 = CARTESIAN_POINT ( 'NONE',  ( 771.2633955100217236, -431.9073299311464211, -363.4237431249939618 ) ) ;
#16984 = FACE_OUTER_BOUND ( 'NONE', #24536, .T. ) ;
#16985 = PLANE ( 'NONE',  #30623 ) ;
#16987 = CARTESIAN_POINT ( 'NONE',  ( 800.2193346964447755, -330.9982390220558273, 355.1360043628815788 ) ) ;
#16986 = CARTESIAN_POINT ( 'NONE',  ( 765.8855110935204493, -118.1692326535054463, 319.0159684113471599 ) ) ;
#16988 = EDGE_LOOP ( 'NONE', ( #22738, #43009 ) ) ;
#16989 = EDGE_CURVE ( 'NONE', #28289, #5691, #779, .T. ) ;
#16990 = CARTESIAN_POINT ( 'NONE',  ( 756.1348686366196716, -257.2601417444141134, -347.5531968255698416 ) ) ;
#16991 = CARTESIAN_POINT ( 'NONE',  ( 797.8594530101008786, -85.54369356751118403, 322.1405469898980982 ) ) ;
#16992 = CARTESIAN_POINT ( 'NONE',  ( 768.8385539511368734, -263.2601417444141134, -306.4236121716840557 ) ) ;
#16993 = CARTESIAN_POINT ( 'NONE',  ( 999.9999999999992042, 248.9999999999998863, -360.0000000000000000 ) ) ;
#16994 = CARTESIAN_POINT ( 'NONE',  ( 800.1688906516307043, -370.1692326535045936, 369.0717654672308186 ) ) ;
#16995 = ORIENTED_EDGE ( 'NONE', *, *, #20200, .F. ) ;
#16996 = CARTESIAN_POINT ( 'NONE',  ( 757.8323909638827445, -290.6346026584195101, 352.1044303154654358 ) ) ;
#16997 = CARTESIAN_POINT ( 'NONE',  ( 796.7845633553578182, -57.62377810805111267, -358.5707757039688204 ) ) ;
#16998 = CARTESIAN_POINT ( 'NONE',  ( 759.9864689768902508, -170.0891481129654608, -354.9819416627836404 ) ) ;
#16999 = CARTESIAN_POINT ( 'NONE',  ( 804.6798772138708955, -423.7255117493281205, 334.6312213355107019 ) ) ;
#17000 = CARTESIAN_POINT ( 'NONE',  ( 747.2067596250078623, -99.18005720387478164, -352.2312462859687230 ) ) ;
#17001 = CARTESIAN_POINT ( 'NONE',  ( 771.2633955100217236, -119.9073299311474443, -363.4237431249939618 ) ) ;
#17002 = VERTEX_POINT ( 'NONE', #43035 ) ;
#17003 = CARTESIAN_POINT ( 'NONE',  ( 755.5913626894240451, -37.64542720878968396, -346.6156483768012890 ) ) ;
#17004 = CARTESIAN_POINT ( 'NONE',  ( 760.7433823573367135, -372.0090635724250205, -355.9930595647440441 ) ) ;
#17006 = CARTESIAN_POINT ( 'NONE',  ( 755.3028492785439312, -423.2817908451521589, 335.9200461376539693 ) ) ;
#17005 = CARTESIAN_POINT ( 'NONE',  ( 797.6776695296629214, -139.5436935675110135, 357.6776695296636603 ) ) ;
#17009 = CARTESIAN_POINT ( 'NONE',  ( 795.6651683502461765, -370.7146871989592114, 371.3240766477733814 ) ) ;
#17008 = PLANE ( 'NONE',  #7046 ) ;
#17007 = DIRECTION ( 'NONE',  ( -1.000000000000000000, -0.000000000000000000, -0.000000000000000000 ) ) ;
#17010 = EDGE_CURVE ( 'NONE', #42674, #29342, #20752, .T. ) ;
#17011 = CARTESIAN_POINT ( 'NONE',  ( 772.4468031744293057, -345.8272453906069472, -363.8651313633793620 ) ) ;
#17012 = CARTESIAN_POINT ( 'NONE',  ( 800.0135310231082713, -350.0891481129648923, -325.0180583372163028 ) ) ;
#17013 = CARTESIAN_POINT ( 'NONE',  ( 764.1737431748507561, -130.3726999360621619, -371.6461892240376415 ) ) ;
#17014 = CARTESIAN_POINT ( 'NONE',  ( 792.2312462859673587, -443.9073299311464780, 307.2067596250082602 ) ) ;
#17016 = CARTESIAN_POINT ( 'NONE',  ( -468.8365100919714337, 260.0000000000001705, -199.9999999999908766 ) ) ;
#17015 = DIRECTION ( 'NONE',  ( -0.000000000000000000, -0.000000000000000000, 1.000000000000000000 ) ) ;
#17017 = CARTESIAN_POINT ( 'NONE',  ( 755.8398074228967971, -307.4419599262320730, -333.4516893846970333 ) ) ;
#17018 = CARTESIAN_POINT ( 'NONE',  ( 762.1177392798416577, -162.5545181178802352, -309.8865473780659272 ) ) ;
#17019 = DIRECTION ( 'NONE',  ( 1.000000000000000000, 4.625929269271485914E-16, 0.000000000000000000 ) ) ;
#17020 = DIRECTION ( 'NONE',  ( 0.000000000000000000, -1.000000000000000000, 0.000000000000000000 ) ) ;
#17021 = CARTESIAN_POINT ( 'NONE',  ( 779.4763451958990572, -320.7363362996979390, 365.0264073115438919 ) ) ;
#17022 = CARTESIAN_POINT ( 'NONE',  ( 814.2805881961230625, -289.6454272087889308, 331.2368401574024119 ) ) ;
#17023 = CARTESIAN_POINT ( 'NONE',  ( 810.7187646348534145, -162.4527844766018632, -356.7737145352016341 ) ) ;
#17024 = FACE_OUTER_BOUND ( 'NONE', #6699, .T. ) ;
#17025 = CARTESIAN_POINT ( 'NONE',  ( 814.4686193811664907, -99.28179084515313946, 346.2056067578752732 ) ) ;
#17026 = CARTESIAN_POINT ( 'NONE',  ( 763.0537975583475827, -312.4527844766012663, -371.0346526505627480 ) ) ;
#17027 = EDGE_CURVE ( 'NONE', #30441, #19176, #39137, .T. ) ;
#17028 = CARTESIAN_POINT ( 'NONE',  ( -598.8365100919716042, 240.0000000000001705, -199.9999999999899671 ) ) ;
#17029 = PRODUCT_DEFINITION_SHAPE ( 'NONE', 'NONE',  #45732 ) ;
#17030 = CARTESIAN_POINT ( 'NONE',  ( 879.9999999999992042, 99.99999999999984368, 360.0000000000000000 ) ) ;
#17031 = CARTESIAN_POINT ( 'NONE',  ( 755.0636971347428243, -196.2709662947835909, 341.7834795799807353 ) ) ;
#17032 = VERTEX_POINT ( 'NONE', #36331 ) ;
#17033 = CARTESIAN_POINT ( 'NONE',  ( 814.4686193811664907, -435.2817908451521021, 346.2056067578752732 ) ) ;
#17034 = CARTESIAN_POINT ( 'NONE',  ( 793.4146539503750546, -385.9874144716864066, -307.6481478633938877 ) ) ;
#17035 = CARTESIAN_POINT ( 'NONE',  ( 811.0346526505616112, -134.6346026584201070, -323.0537975583477532 ) ) ;
#17036 = CARTESIAN_POINT ( 'NONE',  ( 786.5483106153019435, -55.64542720878963422, 364.1601925771022366 ) ) ;
#17037 = CARTESIAN_POINT ( 'NONE',  ( 813.1304606946830518, -401.9073299311463643, -352.3570229623690580 ) ) ;
#17038 = CARTESIAN_POINT ( 'NONE',  ( 927.9999999999992042, 154.9999999999998863, -360.0000000000000000 ) ) ;
#17039 = CARTESIAN_POINT ( 'NONE',  ( 804.1601925771018387, -415.4419599262318457, 346.5483106153029098 ) ) ;
#17040 = ORIENTED_EDGE ( 'NONE', *, *, #23904, .F. ) ;
#17041 = EDGE_CURVE ( 'NONE', #38829, #44752, #23676, .T. ) ;
#17042 = CARTESIAN_POINT ( 'NONE',  ( 746.7653713866222915, -161.2601417444143976, -351.0478386215610271 ) ) ;
#17043 = CARTESIAN_POINT ( 'NONE',  ( 791.1614460488616487, -275.2601417444140566, 373.5763878283158874 ) ) ;
#17044 = CARTESIAN_POINT ( 'NONE',  ( 804.6798772138710092, -111.7255117493292857, 334.6312213355106451 ) ) ;
#17045 = ORIENTED_EDGE ( 'NONE', *, *, #23279, .F. ) ;
#17046 = CARTESIAN_POINT ( 'NONE',  ( 797.6776695296629214, -259.5436935675106156, 357.6776695296636603 ) ) ;
#17047 = CARTESIAN_POINT ( 'NONE',  ( 746.8695393053150156, -5.907329931147798696, -327.6429770376306010 ) ) ;
#17048 = CARTESIAN_POINT ( 'NONE',  ( 789.9999999999992042, 205.0000000000000568, -319.9999999999999432 ) ) ;
#17049 = EDGE_CURVE ( 'NONE', #24181, #16933, #11899, .T. ) ;
#17050 = ORIENTED_EDGE ( 'NONE', *, *, #21115, .F. ) ;
#17051 = ORIENTED_EDGE ( 'NONE', *, *, #30056, .T. ) ;
#17052 = CARTESIAN_POINT ( 'NONE',  ( 805.1927285166397041, -184.8164208402380950, -341.8018195045277707 ) ) ;
#17053 = CARTESIAN_POINT ( 'NONE',  ( 810.4231160770870019, -408.5545181178794110, -321.9338519418446936 ) ) ;
#17054 = ADVANCED_FACE ( 'NONE', ( #43935, #9055, #2127 ), #23121, .T. ) ;
#17055 = CARTESIAN_POINT ( 'NONE',  ( 800.0135310231082713, -38.08914811296587999, 325.0180583372163028 ) ) ;
#17056 = CARTESIAN_POINT ( 'NONE',  ( 781.8018195045266339, -262.2709662947831930, -365.1927285166406705 ) ) ;
#17058 = CARTESIAN_POINT ( 'NONE',  ( 749.8865473780648472, -236.5328690171414792, 322.1177392798429082 ) ) ;
#17057 = CARTESIAN_POINT ( 'NONE',  ( 782.4968714119720516, -370.8164208402375834, 305.0891759886411023 ) ) ;
#17059 = EDGE_CURVE ( 'NONE', #22826, #37323, #15547, .T. ) ;
#17060 = CARTESIAN_POINT ( 'NONE',  ( 804.1105419155481968, -267.8272453906071746, -347.6308680596136469 ) ) ;
#17061 = CARTESIAN_POINT ( 'NONE',  ( 774.6858677611749044, -249.7255117493288594, -315.5713283507209894 ) ) ;
#17062 = CARTESIAN_POINT ( 'NONE',  ( 762.3223304703356007, -415.5436935675102177, -322.3223304703362828 ) ) ;
#17063 = CARTESIAN_POINT ( 'NONE',  ( 791.9812246680005501, -68.63460265842033436, -361.9419747391813189 ) ) ;
#17064 = CARTESIAN_POINT ( 'NONE',  ( 804.9363028652555840, -232.2709662947834488, 338.2165204200192079 ) ) ;
#17065 = VERTEX_POINT ( 'NONE', #33542 ) ;
#17066 = CARTESIAN_POINT ( 'NONE',  ( 745.0891759886404770, -364.2709662947830793, 342.4968714119734159 ) ) ;
#17067 = CARTESIAN_POINT ( 'NONE',  ( 989.9999999999992042, 239.9999999999998863, 360.0000000000000000 ) ) ;
#17068 = CARTESIAN_POINT ( 'NONE',  ( 744.6391490659812007, -62.73633629969871350, -338.7502325331110455 ) ) ;
#17069 = CARTESIAN_POINT ( 'NONE',  ( 773.4999999999993179, -365.3551492539851893, -28.13243251470704109 ) ) ;
#17070 = DIRECTION ( 'NONE',  ( 0.000000000000000000, 0.000000000000000000, 1.000000000000000000 ) ) ;
#17071 = CARTESIAN_POINT ( 'NONE',  ( 802.9823548866075953, -241.0999726633345119, 330.0799878456151077 ) ) ;
#17072 = CARTESIAN_POINT ( 'NONE',  ( 781.7834795799800531, -106.8164208402383935, 315.0636971347436202 ) ) ;
#17073 = EDGE_LOOP ( 'NONE', ( #10813, #31702, #33636, #11574 ) ) ;
#17074 = CARTESIAN_POINT ( 'NONE',  ( 798.5707757039680246, -5.463609026971610660, -356.7845633553585003 ) ) ;
#17075 = CARTESIAN_POINT ( 'NONE',  ( 808.0189434323515343, -86.08914811296573077, -319.0252816721025511 ) ) ;
#17076 = CARTESIAN_POINT ( 'NONE',  ( 757.2208543904082489, -280.7146871989594956, 350.9844846989624330 ) ) ;
#17077 = CARTESIAN_POINT ( 'NONE',  ( 804.9363028652555840, -448.2709662947827951, -338.2165204200192079 ) ) ;
#17078 = CARTESIAN_POINT ( 'NONE',  ( 801.9419747391806368, -42.45278447660223264, -351.9812246680014027 ) ) ;
#17079 = EDGE_CURVE ( 'NONE', #15790, #8154, #39213, .T. ) ;
#17080 = CARTESIAN_POINT ( 'NONE',  ( 778.7629533639073998, -8.736336299698871599, 375.0009284576466371 ) ) ;
#17081 = CARTESIAN_POINT ( 'NONE',  ( 745.0891759886404770, -196.2709662947835909, -342.4968714119734159 ) ) ;
#17082 = ADVANCED_FACE ( 'NONE', ( #15763 ), #1891, .F. ) ;
#17083 = CARTESIAN_POINT ( 'NONE',  ( 745.4481719005789273, -171.7255117493291152, 347.5162901302853129 ) ) ;
#17084 = CARTESIAN_POINT ( 'NONE',  ( 756.3353852180819104, -77.90732993114757221, 331.1735550268788302 ) ) ;
#17085 = DIRECTION ( 'NONE',  ( -1.880165489482579047E-16, -1.000000000000000000, -0.000000000000000000 ) ) ;
#17086 = CARTESIAN_POINT ( 'NONE',  ( 919.9999999999993179, 219.9999999999998863, -359.9749999999999659 ) ) ;
#17087 = CARTESIAN_POINT ( 'NONE',  ( 751.2241431872005251, -256.1692326535049915, -359.9636004259367610 ) ) ;
#17088 = CARTESIAN_POINT ( 'NONE',  ( 804.1009440267234822, -431.4636090269702322, 314.0944755984392600 ) ) ;
#17089 = CARTESIAN_POINT ( 'NONE',  ( 787.5162901302840055, -275.3618753856923149, -305.4481719005792684 ) ) ;
#17090 = DIRECTION ( 'NONE',  ( -0.000000000000000000, 1.000000000000000000, -0.000000000000000000 ) ) ;
#17091 = CARTESIAN_POINT ( 'NONE',  ( 751.9810565676468741, -410.0891481129647218, 360.9747183278973921 ) ) ;
#17092 = CARTESIAN_POINT ( 'NONE',  ( 815.2698199232962679, -16.81642084023867412, 342.5225473063383674 ) ) ;
#17093 = CARTESIAN_POINT ( 'NONE',  ( 815.0009284576459549, -30.35105083532391390, -338.7629533639073429 ) ) ;
#17094 = CARTESIAN_POINT ( 'NONE',  ( 800.2193346964447755, -378.9982390220555999, -355.1360043628815788 ) ) ;
#17095 = EDGE_CURVE ( 'NONE', #11542, #15632, #19683, .T. ) ;
#17096 = CARTESIAN_POINT ( 'NONE',  ( 784.0799538623451781, -35.80559628986934229, 364.6971507214555572 ) ) ;
#17097 = CARTESIAN_POINT ( 'NONE',  ( 800.1688906516307043, -58.16923265350564520, -369.0717654672308186 ) ) ;
#17098 = CARTESIAN_POINT ( 'NONE',  ( 776.9566956441375396, -156.8965053807780805, -364.8461984189686405 ) ) ;
#17099 = CARTESIAN_POINT ( 'NONE',  ( 813.2346286133761168, -173.2601417444143692, 328.9521613784389160 ) ) ;
#17100 = CARTESIAN_POINT ( 'NONE',  ( 791.9812246680005501, -20.63460265842048003, 361.9419747391813189 ) ) ;
#17101 = EDGE_LOOP ( 'NONE', ( #22617, #3655, #19664, #13588 ) ) ;
#17102 = CARTESIAN_POINT ( 'NONE',  ( 765.0180583372156207, -72.99823902205667991, -360.0135310231089534 ) ) ;
#17103 = CARTESIAN_POINT ( 'NONE',  ( 761.2382568024794409, -159.6237781080508285, -356.9571628226838129 ) ) ;
#17104 = CARTESIAN_POINT ( 'NONE',  ( 781.7834795799800531, -154.8164208402382371, 315.0636971347436202 ) ) ;
#17105 = CARTESIAN_POINT ( 'NONE',  ( 761.9338519418445230, 9.467130982857780097, -370.4231160770881957 ) ) ;
#17106 = AXIS2_PLACEMENT_3D ( 'NONE', #24497, #13902, #3511 ) ;
#17107 = DIRECTION ( 'NONE',  ( -0.000000000000000000, 1.000000000000000000, -0.000000000000000000 ) ) ;
#17108 = VERTEX_POINT ( 'NONE', #36999 ) ;
#17109 = CARTESIAN_POINT ( 'NONE',  ( 803.8651313633788504, -29.26014174441482751, 332.4468031744301015 ) ) ;
#17110 = CARTESIAN_POINT ( 'NONE',  ( 814.4686193811664907, -315.2817908451525000, -346.2056067578752732 ) ) ;
#17111 = EDGE_CURVE ( 'NONE', #15260, #40820, #824, .T. ) ;
#17112 = CARTESIAN_POINT ( 'NONE',  ( 792.3570229623691148, -261.1800572038742416, 373.1304606946836770 ) ) ;
#17113 = CARTESIAN_POINT ( 'NONE',  ( 790.9844846989617508, -334.3726999360615082, 317.2208543904092721 ) ) ;
#17114 = CARTESIAN_POINT ( 'NONE',  ( 798.0661480581538854, 21.46713098285774279, 309.5768839229118043 ) ) ;
#17115 = CARTESIAN_POINT ( 'NONE',  ( 805.2837595273609850, -146.7363362996984506, -340.5290396650784714 ) ) ;
#17116 = CARTESIAN_POINT ( 'NONE',  ( 800.2193346964447755, -138.9982390220563957, -355.1360043628815788 ) ) ;
#17117 = CARTESIAN_POINT ( 'NONE',  ( 765.0180583372156207, -312.9982390220559409, -360.0135310231089534 ) ) ;
#17118 = VERTEX_POINT ( 'NONE', #43706 ) ;
#17119 = CARTESIAN_POINT ( 'NONE',  ( 759.2295555964440155, -352.1692326535046504, 353.9708237608231229 ) ) ;
#17120 = DIRECTION ( 'NONE',  ( -0.000000000000000000, 0.6755902076156502511, 0.7372773368101330771 ) ) ;
#17121 = CARTESIAN_POINT ( 'NONE',  ( 804.6971507214547046, -123.2817908451530542, 344.0799538623459739 ) ) ;
#17122 = CARTESIAN_POINT ( 'NONE',  ( 767.8955696845333705, -0.4527844766023628176, 362.1676090361162323 ) ) ;
#17123 = VERTEX_POINT ( 'NONE', #40699 ) ;
#17124 = CARTESIAN_POINT ( 'NONE',  ( 793.5525998758768083, -391.0999726633340288, -372.6845335610516941 ) ) ;
#17125 = FACE_OUTER_BOUND ( 'NONE', #41293, .T. ) ;
#17126 = CARTESIAN_POINT ( 'NONE',  ( 814.4686193811664907, -219.2817908451527558, 346.2056067578752732 ) ) ;
#17127 = CARTESIAN_POINT ( 'NONE',  ( 802.7791456095903868, -172.7146871989598083, 329.0155153010375102 ) ) ;
#17128 = CARTESIAN_POINT ( 'NONE',  ( 759.7806653035534055, -342.9982390220557136, -324.8639956371180801 ) ) ;
#17129 = EDGE_CURVE ( 'NONE', #39820, #1382, #6715, .T. ) ;
#17130 = LINE ( 'NONE', #17595, #3825 ) ;
#17131 = CARTESIAN_POINT ( 'NONE',  ( 798.5707757039680246, -221.4636090269709428, -356.7845633553585003 ) ) ;
#17132 = EDGE_CURVE ( 'NONE', #26042, #34191, #44386, .T. ) ;
#17133 = CARTESIAN_POINT ( 'NONE',  ( 815.2698199232961542, -64.81642084023852135, 342.5225473063383106 ) ) ;
#17134 = AXIS2_PLACEMENT_3D ( 'NONE', #19280, #29906, #43991 ) ;
#17135 = CARTESIAN_POINT ( 'NONE',  ( 807.6521310549275086, -452.9681489794448339, 339.7933401739554711 ) ) ;
#17136 = CARTESIAN_POINT ( 'NONE',  ( 749.2812353651451076, -414.4527844766010389, -323.2262854647983090 ) ) ;
#17137 = FACE_OUTER_BOUND ( 'NONE', #22598, .T. ) ;
#17138 = CARTESIAN_POINT ( 'NONE',  ( 809.0717654672305343, -340.9181544815160123, 360.1688906516309885 ) ) ;
#17139 = CARTESIAN_POINT ( 'NONE',  ( 786.4999999999993179, -512.9681489794448908, -339.9999999999999432 ) ) ;
#17140 = CARTESIAN_POINT ( 'NONE',  ( 808.0189434323515343, -38.08914811296587999, -319.0252816721025511 ) ) ;
#17141 = CARTESIAN_POINT ( 'NONE',  ( 795.1360043628807261, -260.0891481129650060, -360.2193346964456282 ) ) ;
#17142 = DIRECTION ( 'NONE',  ( 0.000000000000000000, 0.000000000000000000, 1.000000000000000000 ) ) ;
#17143 = CARTESIAN_POINT ( 'NONE',  ( 788.8264449731200330, -405.1800572038737300, 363.6646147819171233 ) ) ;
#17144 = CARTESIAN_POINT ( 'NONE',  ( 796.9571628226829034, -143.4636090269711701, 321.2382568024804641 ) ) ;
#17145 = CARTESIAN_POINT ( 'NONE',  ( 786.2694204179717872, -45.28179084515329578, -305.1769319972829067 ) ) ;
#17146 = CARTESIAN_POINT ( 'NONE',  ( 764.0069404352550464, -63.07832356259653750, -359.2566176426627180 ) ) ;
#17147 = CARTESIAN_POINT ( 'NONE',  ( 748.3538107759620743, -64.71468719896019195, 355.8262568251490165 ) ) ;
#17148 = CARTESIAN_POINT ( 'NONE',  ( 758.0580252608178853, -366.4527844766012095, 328.0187753319985404 ) ) ;
#17149 = CARTESIAN_POINT ( 'NONE',  ( 799.9999999999993179, -462.9681489794448339, -309.9999999999998863 ) ) ;
#17150 = CARTESIAN_POINT ( 'NONE',  ( 751.2241431872005251, -136.1692326535053894, 359.9636004259367610 ) ) ;
#17151 = CARTESIAN_POINT ( 'NONE',  ( 755.3201227861273992, -435.7255117493282341, 345.3687786644892981 ) ) ;
#17152 = VERTEX_POINT ( 'NONE', #23364 ) ;
#17153 = CARTESIAN_POINT ( 'NONE',  ( 778.1981804954714335, -58.27096629478398171, -314.8072714833589885 ) ) ;
#17154 = CARTESIAN_POINT ( 'NONE',  ( 760.5453621957607311, -381.0783235625954717, -323.8424801807151425 ) ) ;
#17156 = CARTESIAN_POINT ( 'NONE',  ( 754.8072714833583632, -196.8164208402380950, 338.1981804954721156 ) ) ;
#17155 = CARTESIAN_POINT ( 'NONE',  ( 804.9363028652555840, -184.2709662947835909, 338.2165204200192079 ) ) ;
#17157 = VECTOR ( 'NONE', #36440, 1000.000000000000000 ) ;
#17158 = CARTESIAN_POINT ( 'NONE',  ( 766.5853460496234675, -373.9874144716864066, -372.3518521366060554 ) ) ;
#17159 = LINE ( 'NONE', #45341, #38211 ) ;
#17160 = ORIENTED_EDGE ( 'NONE', *, *, #41564, .F. ) ;
#17161 = CARTESIAN_POINT ( 'NONE',  ( 755.3201227861273992, -387.7255117493283478, 345.3687786644892981 ) ) ;
#17162 = ORIENTED_EDGE ( 'NONE', *, *, #24972, .T. ) ;
#17163 = CARTESIAN_POINT ( 'NONE',  ( 754.9967657858570647, -217.5436935675107293, -365.0032342141425374 ) ) ;
#17164 = CARTESIAN_POINT ( 'NONE',  ( 810.7187646348534145, -138.4527844766019200, 356.7737145352016341 ) ) ;
#17165 = ORIENTED_EDGE ( 'NONE', *, *, #28572, .T. ) ;
#17166 = AXIS2_PLACEMENT_3D ( 'NONE', #7710, #315, #32879 ) ;
#17167 = CARTESIAN_POINT ( 'NONE',  ( 764.3348316497523456, -190.7146871989597798, 308.6759233522265617 ) ) ;
#17168 = CARTESIAN_POINT ( 'NONE',  ( 755.5713283507202505, -197.3618753856926560, -334.6858677611754729 ) ) ;
#17169 = ORIENTED_EDGE ( 'NONE', *, *, #34208, .F. ) ;
#17170 = CARTESIAN_POINT ( 'NONE',  ( 767.8955696845333705, -0.4527844766023628176, -362.1676090361162323 ) ) ;
#17171 = CARTESIAN_POINT ( 'NONE',  ( 789.9200121543843807, -241.9874144716869182, 317.0176451133914384 ) ) ;
#17172 = CARTESIAN_POINT ( 'NONE',  ( 773.4999999999993179, -494.6608068873671300, -357.6536686473015720 ) ) ;
#17173 = LINE ( 'NONE', #41896, #6616 ) ;
#17174 = VERTEX_POINT ( 'NONE', #19016 ) ;
#17175 = CARTESIAN_POINT ( 'NONE',  ( 788.8264449731200330, 2.819942796124898177, -363.6646147819171233 ) ) ;
#17176 = DIRECTION ( 'NONE',  ( 1.000000000000000000, -0.000000000000000000, -0.000000000000000000 ) ) ;
#17177 = ORIENTED_EDGE ( 'NONE', *, *, #8086, .T. ) ;
#17178 = CARTESIAN_POINT ( 'NONE',  ( 788.6739635108323228, -271.6454272087889876, -373.9316612368139090 ) ) ;
#17179 = CARTESIAN_POINT ( 'NONE',  ( 752.7379699480933368, -132.0090635724257595, 361.9858362298580232 ) ) ;
#17181 = CARTESIAN_POINT ( 'NONE',  ( 804.4286716492782716, -209.3618753856926276, -345.3141322388244703 ) ) ;
#17180 = FACE_OUTER_BOUND ( 'NONE', #29062, .T. ) ;
#17182 = CARTESIAN_POINT ( 'NONE',  ( 772.3691319403857278, -383.2601417444137155, -315.8894580844506663 ) ) ;
#17183 = FACE_OUTER_BOUND ( 'NONE', #19730, .T. ) ;
#17184 = DIRECTION ( 'NONE',  ( 1.000000000000000000, 0.000000000000000000, 0.000000000000000000 ) ) ;
#17185 = CARTESIAN_POINT ( 'NONE',  ( 801.5560724626406000, -96.55451811788039151, -326.7756240680316182 ) ) ;
#17186 = CARTESIAN_POINT ( 'NONE',  ( 815.3608509340175488, -386.7363362996977116, 341.2497674668889545 ) ) ;
#17187 = VECTOR ( 'NONE', #33831, 1000.000000000000114 ) ;
#17188 = LINE ( 'NONE', #31046, #454 ) ;
#17189 = CARTESIAN_POINT ( 'NONE',  ( 798.0661480581538854, 21.46713098285774279, -309.5768839229118043 ) ) ;
#17190 = CARTESIAN_POINT ( 'NONE',  ( 796.9462024416508257, -324.4527844766013231, -308.9653473494370246 ) ) ;
#17191 = CARTESIAN_POINT ( 'NONE',  ( -769.9999999999992042, 205.0000000000000568, -319.9999999999999432 ) ) ;
#17192 = CARTESIAN_POINT ( 'NONE',  ( 755.5713283507202505, -77.36187538569302546, -334.6858677611754729 ) ) ;
#17193 = CARTESIAN_POINT ( 'NONE',  ( 807.2620300519052989, -216.0090635724255037, 318.0141637701419768 ) ) ;
#17194 = CARTESIAN_POINT ( 'NONE',  ( 812.6845335610512393, -151.9874144716871740, -353.5525998758768651 ) ) ;
#17195 = CARTESIAN_POINT ( 'NONE',  ( 746.8695393053150156, -197.9073299311472169, 327.6429770376306010 ) ) ;
#17196 = CARTESIAN_POINT ( 'NONE',  ( 814.5518280994195948, -423.7255117493281205, -332.4837098697145734 ) ) ;
#17197 = CARTESIAN_POINT ( 'NONE',  ( -338.8365100919713200, 240.0000000000001137, -202.7499999999916724 ) ) ;
#17198 = CARTESIAN_POINT ( 'NONE',  ( 768.0187753319979720, -296.6346026584195670, 318.0580252608186242 ) ) ;
#17199 = CARTESIAN_POINT ( 'NONE',  ( 779.4763451958990572, -56.73633629969872771, 365.0264073115438919 ) ) ;
#17200 = CARTESIAN_POINT ( 'NONE',  ( 778.1981804954714335, -418.2709662947827383, -314.8072714833589885 ) ) ;
#17201 = ADVANCED_BREP_SHAPE_REPRESENTATION ( '', ( #2862, #26858 ), #9809 ) ;
#17202 = DIRECTION ( 'NONE',  ( 1.000000000000000000, -0.000000000000000000, -0.000000000000000000 ) ) ;
#17203 = CARTESIAN_POINT ( 'NONE',  ( 786.4999999999993179, -365.3551492539851893, -28.13243251470704109 ) ) ;
#17205 = CARTESIAN_POINT ( 'NONE',  ( 778.2165204200184689, -310.8164208402377540, 364.9363028652563230 ) ) ;
#17204 = CARTESIAN_POINT ( 'NONE',  ( 760.5453621957607311, -117.0783235625963528, 323.8424801807151425 ) ) ;
#17206 = VERTEX_POINT ( 'NONE', #27076 ) ;
#17207 = CARTESIAN_POINT ( 'NONE',  ( 804.9511171171677688, -245.8055962898686460, -335.8780910478229202 ) ) ;
#17208 = CARTESIAN_POINT ( 'NONE',  ( 774.6858677611749044, -81.72551174932937101, 315.5713283507209894 ) ) ;
#17209 = CARTESIAN_POINT ( 'NONE',  ( 766.5853460496234675, -253.9874144716868329, -372.3518521366060554 ) ) ;
#17210 = CYLINDRICAL_SURFACE ( 'NONE', #1991, 9.999999999999980460 ) ;
#17211 = CARTESIAN_POINT ( 'NONE',  ( 805.9055244015594326, -411.6237781080499758, 315.8990559732753240 ) ) ;
#17212 = ORIENTED_EDGE ( 'NONE', *, *, #689, .T. ) ;
#17213 = CARTESIAN_POINT ( 'NONE',  ( 800.2193346964447755, -282.9982390220558841, 355.1360043628815788 ) ) ;
#17214 = CARTESIAN_POINT ( 'NONE',  ( 793.2243759319678702, -50.53286901714203339, -318.4439275373583200 ) ) ;
#17215 = CARTESIAN_POINT ( 'NONE',  ( 778.2165204200184689, -166.8164208402382087, -364.9363028652563230 ) ) ;
#17216 = CARTESIAN_POINT ( 'NONE',  ( 771.2633955100217236, -191.9073299311471885, -363.4237431249939618 ) ) ;
#17217 = CARTESIAN_POINT ( 'NONE',  ( 804.4286716492782716, -425.3618753856919170, 345.3141322388244703 ) ) ;
#17218 = CARTESIAN_POINT ( 'NONE',  ( 758.8095938919642549, -128.0891481129655176, -311.6929314249763365 ) ) ;
#17219 = MANIFOLD_SOLID_BREP ( 'Fillet2', #4038 ) ;
#17220 = AXIS2_PLACEMENT_3D ( 'NONE', #7900, #34962, #17184 ) ;
#17221 = CARTESIAN_POINT ( 'NONE',  ( 794.9819416627830151, -108.9982390220565804, -319.9864689768909898 ) ) ;
#17222 = CARTESIAN_POINT ( 'NONE',  ( 780.5236548040995785, -44.73633629969875614, -314.9735926884559944 ) ) ;
#17223 = CIRCLE ( 'NONE', #21646, 24.99999999999991118 ) ;
#17224 = CARTESIAN_POINT ( 'NONE',  ( 766.9102291470427417, -378.5545181178795247, -318.6633372737382501 ) ) ;
#17226 = CARTESIAN_POINT ( 'NONE',  ( 772.4468031744293057, -441.8272453906066630, 363.8651313633793620 ) ) ;
#17225 = CARTESIAN_POINT ( 'NONE',  ( 781.7834795799800531, -130.8164208402383224, 315.0636971347436202 ) ) ;
#17227 = CARTESIAN_POINT ( 'NONE',  ( 760.5453621957607311, -93.07832356259645223, 323.8424801807151425 ) ) ;
#17230 = CARTESIAN_POINT ( 'NONE',  ( 812.6845335610512393, -343.9874144716865771, 353.5525998758768651 ) ) ;
#17229 = CARTESIAN_POINT ( 'NONE',  ( 791.7608162188021197, 240.0000000000000853, -320.0000000000000000 ) ) ;
#17228 = DIRECTION ( 'NONE',  ( -0.000000000000000000, -0.000000000000000000, 1.000000000000000000 ) ) ;
#17231 = VERTEX_POINT ( 'NONE', #26157 ) ;
#17232 = CARTESIAN_POINT ( 'NONE',  ( 755.8894580844503253, -351.8272453906068336, -332.3691319403863531 ) ) ;
#17233 = CARTESIAN_POINT ( 'NONE',  ( 794.9819416627830151, -348.9982390220558273, -319.9864689768909898 ) ) ;
#17234 = CARTESIAN_POINT ( 'NONE',  ( 747.6481478633932056, -133.0999726633348246, -353.4146539503763620 ) ) ;
#17235 = CARTESIAN_POINT ( 'NONE',  ( 762.1177392798416577, -42.55451811788057626, 309.8865473780659272 ) ) ;
#17236 = COLOUR_RGB ( '',0.7921568627450980005, 0.8196078431372548767, 0.9333333333333333481 ) ;
#17238 = FACE_OUTER_BOUND ( 'NONE', #10946, .T. ) ;
#17237 = CARTESIAN_POINT ( 'NONE',  ( -773.4999999999993179, -365.3551492539851893, -18.13243251470705886 ) ) ;
#17239 = CARTESIAN_POINT ( 'NONE',  ( 790.8726784830453198, -298.7146871989593251, -362.5472867521010585 ) ) ;
#17240 = CARTESIAN_POINT ( 'NONE',  ( 792.1044303154645831, -444.4527844766009821, -317.8323909638837677 ) ) ;
#17241 = CARTESIAN_POINT ( 'NONE',  ( 768.9521613784389729, -153.8272453906075157, -373.2346286133773106 ) ) ;
#17242 = FACE_OUTER_BOUND ( 'NONE', #19051, .T. ) ;
#17243 = CARTESIAN_POINT ( 'NONE',  ( 447.2824899080285945, 256.4999999999999432, -199.9999999999972431 ) ) ;
#17244 = CARTESIAN_POINT ( 'NONE',  ( 787.5531968255692163, -381.8272453906068336, 316.1348686366205811 ) ) ;
#17245 = CARTESIAN_POINT ( 'NONE',  ( 809.0717654672305343, -292.9181544815162397, 360.1688906516309885 ) ) ;
#17246 = EDGE_CURVE ( 'NONE', #38502, #31293, #22690, .T. ) ;
#17247 = CARTESIAN_POINT ( 'NONE',  ( 792.2312462859673587, -179.9073299311472454, -307.2067596250082602 ) ) ;
#17248 = DIRECTION ( 'NONE',  ( 1.000000000000000000, 0.000000000000000000, 0.000000000000000000 ) ) ;
#17249 = CARTESIAN_POINT ( 'NONE',  ( 778.7629533639073998, -104.7363362996985785, 375.0009284576466371 ) ) ;
#17250 = CARTESIAN_POINT ( 'NONE',  ( 815.2698199232961542, -304.8164208402376403, -342.5225473063383106 ) ) ;
#17251 = CARTESIAN_POINT ( 'NONE',  ( -786.4999999999993179, 26.27639943461424110, 900.0000000000004547 ) ) ;
#17252 = PLANE ( 'NONE',  #13909 ) ;
#17253 = CARTESIAN_POINT ( 'NONE',  ( 804.9363028652555840, -184.2709662947835909, 338.2165204200192079 ) ) ;
#17254 = AXIS2_PLACEMENT_3D ( 'NONE', #2651, #34969, #24339 ) ;
#17255 = ORIENTED_EDGE ( 'NONE', *, *, #21883, .F. ) ;
#17256 = CARTESIAN_POINT ( 'NONE',  ( 791.0478386215596629, -429.8272453906067199, 306.7653713866226326 ) ) ;
#17257 = CARTESIAN_POINT ( 'NONE',  ( 759.8311093483677041, -382.1692326535045936, -310.9282345327691814 ) ) ;
#17258 = CARTESIAN_POINT ( 'NONE',  ( 746.8695393053150156, -125.9073299311474159, -327.6429770376306010 ) ) ;
#17259 = CARTESIAN_POINT ( 'NONE',  ( 772.5602148656447525, -393.7255117493283478, -305.7998596910095443 ) ) ;
#17260 = LINE ( 'NONE', #27652, #26166 ) ;
#17261 = CARTESIAN_POINT ( 'NONE',  ( 788.7631598425961101, -1.441959926233096656, 305.7194118038759143 ) ) ;
#17262 = VERTEX_POINT ( 'NONE', #5354 ) ;
#17263 = CARTESIAN_POINT ( 'NONE',  ( 803.8556311672234642, -153.6237781080508000, -365.6418435158340117 ) ) ;
#17264 = FACE_BOUND ( 'NONE', #19260, .T. ) ;
#17265 = CARTESIAN_POINT ( 'NONE',  ( 798.0661480581538854, -314.5328690171411949, 309.5768839229118043 ) ) ;
#17266 = CARTESIAN_POINT ( 'NONE',  ( 800.0135310231082713, -110.0891481129656597, 325.0180583372163028 ) ) ;
#17267 = ORIENTED_EDGE ( 'NONE', *, *, #39387, .T. ) ;
#17268 = AXIS2_PLACEMENT_3D ( 'NONE', #29850, #40032, #36785 ) ;
#17269 = CARTESIAN_POINT ( 'NONE',  ( 792.1044303154645831, -300.4527844766012663, 317.8323909638837677 ) ) ;
#17270 = CARTESIAN_POINT ( 'NONE',  ( 787.4397851343537695, -21.72551174932956641, -374.2001403089903988 ) ) ;
#17271 = CARTESIAN_POINT ( 'NONE',  ( 790.6613096012131336, -448.0786441114948389, 367.3906422790598185 ) ) ;
#17272 = ORIENTED_EDGE ( 'NONE', *, *, #7810, .F. ) ;
#17273 = CARTESIAN_POINT ( 'NONE',  ( 754.3581564841646241, -425.4636090269703459, -316.1443688327762516 ) ) ;
#17274 = ORIENTED_EDGE ( 'NONE', *, *, #45466, .T. ) ;
#17275 = CARTESIAN_POINT ( 'NONE',  ( 771.1735550268778070, -33.18005720387498769, 316.3353852180827630 ) ) ;
#17276 = CARTESIAN_POINT ( 'NONE',  ( 768.0187753319979720, -272.6346026584196807, -318.0580252608186242 ) ) ;
#17278 = CARTESIAN_POINT ( 'NONE',  ( 813.9316612368132837, -247.4419599262323004, 348.6739635108323228 ) ) ;
#17277 = CARTESIAN_POINT ( 'NONE',  ( 777.4774526936600978, -370.2709662947830793, 304.7301800767028226 ) ) ;
#17279 = EDGE_CURVE ( 'NONE', #35219, #1648, #17130, .T. ) ;
#17280 = AXIS2_PLACEMENT_3D ( 'NONE', #35188, #10245, #3564 ) ;
#17281 = CARTESIAN_POINT ( 'NONE',  ( 804.8461984189677878, -242.1908817542435770, -336.9566956441385628 ) ) ;
#17282 = CARTESIAN_POINT ( 'NONE',  ( 758.0580252608178853, -270.4527844766014937, -328.0187753319985404 ) ) ;
#17283 = CARTESIAN_POINT ( 'NONE',  ( 804.6798772138710092, -447.7255117493281205, -334.6312213355106451 ) ) ;
#17284 = CARTESIAN_POINT ( 'NONE',  ( 804.9363028652555840, -88.27096629478390355, -338.2165204200192079 ) ) ;
#17285 = AXIS2_PLACEMENT_3D ( 'NONE', #27518, #34688, #3517 ) ;
#17286 = CARTESIAN_POINT ( 'NONE',  ( 778.2165204200184689, -238.8164208402379813, 364.9363028652563230 ) ) ;
#17287 = VERTEX_POINT ( 'NONE', #27976 ) ;
#17288 = CARTESIAN_POINT ( 'NONE',  ( 748.9653473494363425, -386.6346026584191691, 356.9462024416521331 ) ) ;
#17289 = DIRECTION ( 'NONE',  ( 1.000000000000000000, -1.880165489482579047E-16, 0.000000000000000000 ) ) ;
#17290 = CARTESIAN_POINT ( 'NONE',  ( 799.9636004259356241, -46.91815448151694312, -311.2241431872006956 ) ) ;
#17291 = CARTESIAN_POINT ( 'NONE',  ( 914.9999999999992042, 74.99999999999984368, 350.0000000000000000 ) ) ;
#17292 = CARTESIAN_POINT ( 'NONE',  ( 927.9999999999992042, 154.9999999999998863, -350.0000000000000000 ) ) ;
#17293 = EDGE_CURVE ( 'NONE', #45518, #9555, #20361, .T. ) ;
#17294 = CARTESIAN_POINT ( 'NONE',  ( 755.1538015810308480, -230.1908817542436338, 343.0433043558613804 ) ) ;
#17295 = CARTESIAN_POINT ( 'NONE',  ( 804.6798772138708955, -111.7255117493293000, 334.6312213355107019 ) ) ;
#17296 = EDGE_LOOP ( 'NONE', ( #32673, #8166, #11722, #4712 ) ) ;
#17297 = CARTESIAN_POINT ( 'NONE',  ( 776.9254006560222479, 3.809118245755632959, -314.8983024940802125 ) ) ;
#17298 = CARTESIAN_POINT ( 'NONE',  ( 808.3070685750232087, -66.99823902205670834, -361.1904061080339829 ) ) ;
#17299 = CARTESIAN_POINT ( 'NONE',  ( 766.7756240680305382, -302.5328690171411949, 361.5560724626415663 ) ) ;
#17300 = CARTESIAN_POINT ( 'NONE',  ( 794.9819416627830151, -444.9982390220554862, -319.9864689768909898 ) ) ;
#17301 = VECTOR ( 'NONE', #8098, 1000.000000000000000 ) ;
#17302 = CARTESIAN_POINT ( 'NONE',  ( 762.1177392798416577, -18.55451811788065797, 309.8865473780659272 ) ) ;
#17303 = CARTESIAN_POINT ( 'NONE',  ( 813.1304606946830518, -209.9073299311470748, -352.3570229623690580 ) ) ;
#17304 = AXIS2_PLACEMENT_3D ( 'NONE', #7102, #17949, #22973 ) ;
#17305 = CARTESIAN_POINT ( 'NONE',  ( 812.7932403749906598, -183.1800572038744974, 327.7687537140311633 ) ) ;
#17306 = CARTESIAN_POINT ( 'NONE',  ( 785.3141322388236176, -93.72551174932934259, 364.4286716492789537 ) ) ;
#17307 = CARTESIAN_POINT ( 'NONE',  ( 789.9999999999992042, 240.0000000000000568, -319.9999999999999432 ) ) ;
#17308 = DIRECTION ( 'NONE',  ( -0.000000000000000000, -0.000000000000000000, 1.000000000000000000 ) ) ;
#17309 = CARTESIAN_POINT ( 'NONE',  ( 798.0661480581538854, -266.5328690171413655, -309.5768839229118043 ) ) ;
#17310 = CARTESIAN_POINT ( 'NONE',  ( 755.8990559732751535, -419.4636090269702891, 365.9055244015606831 ) ) ;
#17311 = CARTESIAN_POINT ( 'NONE',  ( 754.9967657858570647, -289.5436935675103882, -365.0032342141425374 ) ) ;
#17312 = CARTESIAN_POINT ( 'NONE',  ( 769.9999999999992042, 205.0000000000000568, -329.9999999999999432 ) ) ;
#17313 = CARTESIAN_POINT ( 'NONE',  ( 769.1273215169530886, -358.7146871989592114, 317.4527132478988847 ) ) ;
#17314 = CARTESIAN_POINT ( 'NONE',  ( 814.2001403089898304, -65.36187538569306810, 347.4397851343538264 ) ) ;
#17315 = CARTESIAN_POINT ( 'NONE',  ( 795.1360043628807261, -404.0891481129646081, -360.2193346964456282 ) ) ;
#17316 = CARTESIAN_POINT ( 'NONE',  ( 793.2243759319678702, -2.532869017142183932, 318.4439275373583200 ) ) ;
#17317 = COLOUR_RGB ( '',0.7921568627450980005, 0.8196078431372548767, 0.9333333333333333481 ) ;
#17318 = CARTESIAN_POINT ( 'NONE',  ( 803.8556311672234642, -33.62377810805116951, -365.6418435158340117 ) ) ;
#17319 = CARTESIAN_POINT ( 'NONE',  ( 793.2243759319678702, -194.5328690171415644, -318.4439275373583200 ) ) ;
#17320 = CARTESIAN_POINT ( 'NONE',  ( 813.9316612368132837, -175.4419599262325562, 348.6739635108323228 ) ) ;
#17321 = CARTESIAN_POINT ( 'NONE',  ( 756.3353852180820240, -5.907329931147799584, 331.1735550268787733 ) ) ;
#17322 = VECTOR ( 'NONE', #25928, 1000.000000000000000 ) ;
#17323 = ORIENTED_EDGE ( 'NONE', *, *, #25106, .F. ) ;
#17324 = CARTESIAN_POINT ( 'NONE',  ( 802.1676090361156639, -86.63460265842023489, -327.8955696845344505 ) ) ;
#17325 = CARTESIAN_POINT ( 'NONE',  ( 804.9511171171677688, -197.8055962898688733, -335.8780910478229202 ) ) ;
#17326 = UNCERTAINTY_MEASURE_WITH_UNIT (LENGTH_MEASURE( 1.000000000000000082E-05 ), #40357, 'distance_accuracy_value', 'NONE');
#17327 = CARTESIAN_POINT ( 'NONE',  ( 803.6646147819161570, -185.9073299311472454, 348.8264449731210561 ) ) ;
#17328 = CARTESIAN_POINT ( 'NONE',  ( 747.3154664389472828, -43.98741447168752217, -326.4474001241230781 ) ) ;
#17329 = CARTESIAN_POINT ( 'NONE',  ( 778.1981804954715471, -346.2709662947830225, 314.8072714833591021 ) ) ;
#17330 = PLANE ( 'NONE',  #30818 ) ;
#17331 = ORIENTED_EDGE ( 'NONE', *, *, #36744, .T. ) ;
#17332 = CARTESIAN_POINT ( 'NONE',  ( 784.0799538623451781, -35.80559628986934229, 364.6971507214555572 ) ) ;
#17333 = CARTESIAN_POINT ( 'NONE',  ( 815.3608509340175488, -290.7363362996980527, -341.2497674668889545 ) ) ;
#17334 = VECTOR ( 'NONE', #3169, 1000.000000000000000 ) ;
#17335 = EDGE_CURVE ( 'NONE', #3566, #34365, #24276, .T. ) ;
#17336 = CARTESIAN_POINT ( 'NONE',  ( 755.2512626584698410, -271.5436935675106156, 315.2512626584710915 ) ) ;
#17337 = EDGE_CURVE ( 'NONE', #2204, #42341, #14911, .T. ) ;
#17338 = CARTESIAN_POINT ( 'NONE',  ( 755.1538015810308480, -350.1908817542433212, 343.0433043558613804 ) ) ;
#17339 = AXIS2_PLACEMENT_3D ( 'NONE', #6506, #26655, #27971 ) ;
#17340 = CARTESIAN_POINT ( 'NONE',  ( 783.0433043558608688, -432.8965053807771142, 315.1538015810313027 ) ) ;
#17341 = CARTESIAN_POINT ( 'NONE',  ( 800.9840315886518738, -148.9181544815166092, -354.1144889064786412 ) ) ;
#17342 = CARTESIAN_POINT ( 'NONE',  ( 774.6312213355099630, -143.3618753856927697, -364.6798772138717482 ) ) ;
#17343 = CARTESIAN_POINT ( 'NONE',  ( 794.9819416627830151, -348.9982390220558273, -319.9864689768909898 ) ) ;
#17344 = ORIENTED_EDGE ( 'NONE', *, *, #32332, .T. ) ;
#17345 = CARTESIAN_POINT ( 'NONE',  ( 772.5602148656447525, -249.7255117493288594, 305.7998596910095443 ) ) ;
#17346 = CARTESIAN_POINT ( 'NONE',  ( 802.7791456095903868, -340.7146871989592114, 329.0155153010375102 ) ) ;
#17347 = EDGE_CURVE ( 'NONE', #2958, #33261, #44860, .T. ) ;
#17348 = DIRECTION ( 'NONE',  ( -0.000000000000000000, 1.000000000000000000, -0.000000000000000000 ) ) ;
#17349 = EDGE_CURVE ( 'NONE', #22842, #23907, #20031, .T. ) ;
#17350 = CIRCLE ( 'NONE', #9961, 8.025000000000003908 ) ;
#17351 = CARTESIAN_POINT ( 'NONE',  ( 754.7162404726377645, -134.7363362996984790, 339.4709603349214717 ) ) ;
#17352 = CARTESIAN_POINT ( 'NONE',  ( 797.6776695296629214, -19.54369356751139364, 357.6776695296636603 ) ) ;
#17353 = ORIENTED_EDGE ( 'NONE', *, *, #4112, .F. ) ;
#17354 = CARTESIAN_POINT ( 'NONE',  ( 750.9282345327678740, -376.9181544815159555, -319.8311093483690115 ) ) ;
#17355 = VECTOR ( 'NONE', #21440, 1000.000000000000000 ) ;
#17356 = CARTESIAN_POINT ( 'NONE',  ( 51.16348990802859475, 260.0000000000000568, -197.2499999999946851 ) ) ;
#17357 = CARTESIAN_POINT ( 'NONE',  ( 766.0291762391763086, -226.9181544815163534, 360.7704444035551319 ) ) ;
#17358 = CARTESIAN_POINT ( 'NONE',  ( 745.1792804349281596, -230.1908817542436338, 343.7566961878542884 ) ) ;
#17359 = CARTESIAN_POINT ( 'NONE',  ( 759.2295555964440155, -184.1692326535052757, 353.9708237608231229 ) ) ;
#17360 = AXIS2_PLACEMENT_3D ( 'NONE', #2996, #20310, #31164 ) ;
#17361 = CARTESIAN_POINT ( 'NONE',  ( 755.0636971347428243, -316.2709662947832499, -341.7834795799807353 ) ) ;
#17362 = CARTESIAN_POINT ( 'NONE',  ( 802.5472867521000353, -220.3726999360618208, -350.8726784830461156 ) ) ;
#17363 = CARTESIAN_POINT ( 'NONE',  ( 796.9462024416508257, -12.45278447660232146, 308.9653473494370246 ) ) ;
#17364 = CARTESIAN_POINT ( 'NONE',  ( 749.2812353651451076, -78.45278447660211896, 323.2262854647983090 ) ) ;
#17365 = CARTESIAN_POINT ( 'NONE',  ( 796.9142768083648889, -452.9681489794446634, 358.6301678913937963 ) ) ;
#17366 = CARTESIAN_POINT ( 'NONE',  ( 792.3570229623691148, -429.1800572038737300, -373.1304606946836770 ) ) ;
#17367 = DIRECTION ( 'NONE',  ( 1.000000000000000000, 0.000000000000000000, 0.000000000000000000 ) ) ;
#17368 = EDGE_CURVE ( 'NONE', #29782, #30209, #31214, .T. ) ;
#17369 = VECTOR ( 'NONE', #43287, 1000.000000000000000 ) ;
#17370 = CARTESIAN_POINT ( 'NONE',  ( 788.6739635108323228, -367.6454272087886466, 373.9316612368139090 ) ) ;
#17371 = EDGE_CURVE ( 'NONE', #34451, #1374, #16341, .T. ) ;
#17372 = LINE ( 'NONE', #18060, #6546 ) ;
#17373 = CARTESIAN_POINT ( 'NONE',  ( 813.1304606946830518, -281.9073299311468759, 352.3570229623690580 ) ) ;
#17374 = CARTESIAN_POINT ( 'NONE',  ( 805.0032342141412300, -37.54369356751132614, -314.9967657858571783 ) ) ;
#17375 = CARTESIAN_POINT ( 'NONE',  ( 755.3201227861273992, -291.7255117493285752, -345.3687786644892981 ) ) ;
#17376 = VECTOR ( 'NONE', #42145, 1000.000000000000000 ) ;
#17377 = CARTESIAN_POINT ( 'NONE',  ( -775.4999999999993179, -513.1383975375929367, -367.9999999999999432 ) ) ;
#17378 = CARTESIAN_POINT ( 'NONE',  ( 804.6798772138708955, -399.7255117493283478, 334.6312213355107019 ) ) ;
#17379 = CARTESIAN_POINT ( 'NONE',  ( 801.5560724626406000, -144.5545181178802636, 326.7756240680316182 ) ) ;
#17380 = CARTESIAN_POINT ( 'NONE',  ( 797.8822607201568644, -30.55451811788062244, -370.1134526219340160 ) ) ;
#17381 = CARTESIAN_POINT ( 'NONE',  ( 763.2154366446407039, -93.62377810805098477, -321.4292242960311228 ) ) ;
#17382 = CARTESIAN_POINT ( 'NONE',  ( 813.2346286133761168, -77.26014174441466764, 328.9521613784389160 ) ) ;
#17383 = CARTESIAN_POINT ( 'NONE',  ( 755.3201227861273992, -411.7255117493282910, 345.3687786644892981 ) ) ;
#17384 = CARTESIAN_POINT ( 'NONE',  ( 805.0032342141413437, 10.45630643248851044, 314.9967657858572352 ) ) ;
#17385 = PLANE ( 'NONE',  #16649 ) ;
#17386 = CARTESIAN_POINT ( 'NONE',  ( 778.7502325331095108, -144.3510508353235764, 304.6391490659818828 ) ) ;
#17387 = CARTESIAN_POINT ( 'NONE',  ( 774.6312213355099630, -431.3618753856918033, 364.6798772138717482 ) ) ;
#17388 = VERTEX_POINT ( 'NONE', #16911 ) ;
#17389 = CARTESIAN_POINT ( 'NONE',  ( 757.8323909638827445, -50.63460265842036989, -352.1044303154654358 ) ) ;
#17390 = CARTESIAN_POINT ( 'NONE',  ( 776.9566956441375396, -372.8965053807773415, -364.8461984189686405 ) ) ;
#17392 = CARTESIAN_POINT ( 'NONE',  ( 756.5762568750052424, -219.1800572038744122, 348.7366044899774238 ) ) ;
#17391 = CARTESIAN_POINT ( 'NONE',  ( 759.9864689768902508, -242.0891481129652618, 354.9819416627836404 ) ) ;
#17393 = ORIENTED_EDGE ( 'NONE', *, *, #35409, .T. ) ;
#17394 = CARTESIAN_POINT ( 'NONE',  ( 786.2056067578752163, -395.8055962898682765, -374.4686193811670023 ) ) ;
#17396 = EDGE_CURVE ( 'NONE', #2677, #22833, #38382, .T. ) ;
#17395 = DIRECTION ( 'NONE',  ( 0.000000000000000000, 0.000000000000000000, 1.000000000000000000 ) ) ;
#17397 = VERTEX_POINT ( 'NONE', #42071 ) ;
#17398 = CARTESIAN_POINT ( 'NONE',  ( 755.0636971347428243, -388.2709662947829656, 341.7834795799807353 ) ) ;
#17399 = AXIS2_PLACEMENT_3D ( 'NONE', #15146, #14918, #36374 ) ;
#17400 = EDGE_CURVE ( 'NONE', #13608, #19936, #16683, .T. ) ;
#17401 = VERTEX_POINT ( 'NONE', #41393 ) ;
#17402 = CARTESIAN_POINT ( 'NONE',  ( 796.9462024416508257, -252.4527844766015789, -308.9653473494370246 ) ) ;
#17403 = ADVANCED_FACE ( 'NONE', ( #45088 ), #13443, .F. ) ;
#17404 = EDGE_LOOP ( 'NONE', ( #30452, #30057 ) ) ;
#17405 = CARTESIAN_POINT ( 'NONE',  ( 756.1443688327750579, -189.6237781080507148, 314.3581564841659315 ) ) ;
#17406 = VECTOR ( 'NONE', #15385, 1000.000000000000000 ) ;
#17407 = CARTESIAN_POINT ( 'NONE',  ( 759.7806653035535192, -198.9982390220562536, -324.8639956371181370 ) ) ;
#17408 = ORIENTED_EDGE ( 'NONE', *, *, #13648, .F. ) ;
#17409 = CARTESIAN_POINT ( 'NONE',  ( 794.9819416627830151, -372.9982390220557704, -319.9864689768909898 ) ) ;
#17410 = CARTESIAN_POINT ( 'NONE',  ( 791.9812246680005501, -20.63460265842048003, -361.9419747391813189 ) ) ;
#17411 =( GEOMETRIC_REPRESENTATION_CONTEXT ( 3 ) GLOBAL_UNCERTAINTY_ASSIGNED_CONTEXT ( ( #32911 ) ) GLOBAL_UNIT_ASSIGNED_CONTEXT ( ( #37939, #45108, #9993 ) ) REPRESENTATION_CONTEXT ( 'NONE', 'WORKASPACE' ) );
#17412 =( BOUNDED_CURVE ( )  B_SPLINE_CURVE ( 3, ( #9113, #27135, #2404, #37055 ),
 .UNSPECIFIED., .F., .T. ) 
 B_SPLINE_CURVE_WITH_KNOTS ( ( 4, 4 ),
 ( 1.570796326794896558, 3.141592653589793116 ),
 .UNSPECIFIED. ) 
 CURVE ( )  GEOMETRIC_REPRESENTATION_ITEM ( )  RATIONAL_B_SPLINE_CURVE ( ( 1.000000000000000000, 0.8047378541243649375, 0.8047378541243649375, 1.000000000000000000 ) ) 
 REPRESENTATION_ITEM ( '' )  );
#17413 = CARTESIAN_POINT ( 'NONE',  ( 805.1016975059191054, -222.8965053807778531, 343.0745993439771837 ) ) ;
#17414 = DIRECTION ( 'NONE',  ( 0.000000000000000000, 0.000000000000000000, 1.000000000000000000 ) ) ;
#17415 = DIRECTION ( 'NONE',  ( 0.000000000000000000, 0.000000000000000000, 1.000000000000000000 ) ) ;
#17416 = CIRCLE ( 'NONE', #43222, 10.00000000000006395 ) ;
#17417 = PRODUCT_DEFINITION_SHAPE ( 'NONE', 'NONE',  #44518 ) ;
#17418 = ORIENTED_EDGE ( 'NONE', *, *, #36127, .T. ) ;
#17419 = CARTESIAN_POINT ( 'NONE',  ( 787.5531968255692163, -453.8272453906066630, -316.1348686366205811 ) ) ;
#17420 = DIRECTION ( 'NONE',  ( -0.000000000000000000, 1.000000000000000000, -0.000000000000000000 ) ) ;
#17421 = LINE ( 'NONE', #31499, #23344 ) ;
#17422 = ORIENTED_EDGE ( 'NONE', *, *, #1848, .F. ) ;
#17423 = CARTESIAN_POINT ( 'NONE',  ( 813.5763878283155464, -267.8272453906071746, -351.1614460488615350 ) ) ;
#17424 = CARTESIAN_POINT ( 'NONE',  ( 744.6391490659812007, -134.7363362996984790, 338.7502325331110455 ) ) ;
#17426 = CARTESIAN_POINT ( 'NONE',  ( 795.1360043628807261, -236.0891481129651766, -360.2193346964456282 ) ) ;
#17425 = FACE_OUTER_BOUND ( 'NONE', #5011, .T. ) ;
#17427 = CARTESIAN_POINT ( 'NONE',  ( 773.3843516231979720, -397.4419599262317320, -364.4086373105754433 ) ) ;
#17428 = CARTESIAN_POINT ( 'NONE',  ( -338.8365100919713200, 260.0000000000001137, -202.7499999999916724 ) ) ;
#17429 = PLANE ( 'NONE',  #6900 ) ;
#17430 = CARTESIAN_POINT ( 'NONE',  ( 783.0745993439762742, -128.1908817542439465, -365.1016975059196739 ) ) ;
#17431 = CARTESIAN_POINT ( 'NONE',  ( 766.4474001241216001, -379.0999726633341993, 307.3154664389482491 ) ) ;
#17432 = CARTESIAN_POINT ( 'NONE',  ( -775.4999999999993179, -512.9681489794448908, -352.0000000000000000 ) ) ;
#17433 = CARTESIAN_POINT ( 'NONE',  ( 747.3154664389472828, 4.012585528312341054, -326.4474001241230781 ) ) ;
#17434 = CARTESIAN_POINT ( 'NONE',  ( 767.7687537140311633, -311.9073299311468759, -372.7932403749916830 ) ) ;
#17435 = DIRECTION ( 'NONE',  ( 1.000000000000000000, 0.000000000000000000, 0.000000000000000000 ) ) ;
#17436 = CARTESIAN_POINT ( 'NONE',  ( 794.9819416627830151, 11.00176097794305541, 319.9864689768909898 ) ) ;
#17437 = CARTESIAN_POINT ( 'NONE',  ( 794.9819416627830151, -84.99823902205663728, -319.9864689768909898 ) ) ;
#17438 = CARTESIAN_POINT ( 'NONE',  ( 745.1792804349281596, -254.1908817542435770, 343.7566961878542884 ) ) ;
#17439 = CARTESIAN_POINT ( 'NONE',  ( 747.3154664389472828, -187.9874144716870603, -326.4474001241230781 ) ) ;
#17440 = CARTESIAN_POINT ( 'NONE',  ( 792.3570229623688874, -189.1800572038744122, 373.1304606946836202 ) ) ;
#17441 = CARTESIAN_POINT ( 'NONE',  ( 767.6429770376289525, -441.1800572038735027, -306.8695393053162093 ) ) ;
#17442 = VECTOR ( 'NONE', #21391, 1000.000000000000000 ) ;
#17443 = CARTESIAN_POINT ( 'NONE',  ( 919.9999999999993179, 154.9999999999998863, 350.0000000000000000 ) ) ;
#17444 = CARTESIAN_POINT ( 'NONE',  ( 778.1981804954714335, -274.2709662947833067, 314.8072714833589885 ) ) ;
#17445 = CARTESIAN_POINT ( 'NONE',  ( 761.4292242960306112, -89.46360902697134065, 323.2154366446414429 ) ) ;
#17446 = CARTESIAN_POINT ( 'NONE',  ( 768.0187753319979720, -416.6346026584192259, -318.0580252608186242 ) ) ;
#17447 = DIRECTION ( 'NONE',  ( -0.000000000000000000, 1.000000000000000000, 0.000000000000000000 ) ) ;
#17448 = DIRECTION ( 'NONE',  ( 0.000000000000000000, -1.000000000000000000, -1.056348263647623421E-15 ) ) ;
#17450 = CARTESIAN_POINT ( 'NONE',  ( 771.2633955100217236, -311.9073299311468759, 363.4237431249939618 ) ) ;
#17449 = CARTESIAN_POINT ( 'NONE',  ( 759.2295555964440155, -112.1692326535054889, 353.9708237608231229 ) ) ;
#17451 = VERTEX_POINT ( 'NONE', #41614 ) ;
#17452 = AXIS2_PLACEMENT_3D ( 'NONE', #18952, #29114, #43426 ) ;
#17453 = CARTESIAN_POINT ( 'NONE',  ( 804.9511171171677688, -269.8055962898686175, -335.8780910478229202 ) ) ;
#17454 = CARTESIAN_POINT ( 'NONE',  ( 778.1981804954714335, -82.27096629478388934, 314.8072714833589885 ) ) ;
#17455 = CARTESIAN_POINT ( 'NONE',  ( 758.0141637701419768, -303.0783235625957559, -367.2620300519063790 ) ) ;
#17456 = LINE ( 'NONE', #16770, #31964 ) ;
#17457 = CARTESIAN_POINT ( 'NONE',  ( 751.2241431872005251, -400.1692326535045936, 359.9636004259367610 ) ) ;
#17458 = EDGE_LOOP ( 'NONE', ( #2330, #4045 ) ) ;
#17459 = CARTESIAN_POINT ( 'NONE',  ( 778.1981804954714335, -298.2709662947830793, 314.8072714833589885 ) ) ;
#17460 = CARTESIAN_POINT ( 'NONE',  ( 772.3691319403857278, -47.26014174441477422, -315.8894580844506663 ) ) ;
#17461 = CARTESIAN_POINT ( 'NONE',  ( 757.8323909638827445, -170.6346026584199649, -352.1044303154654358 ) ) ;
#17462 = CARTESIAN_POINT ( 'NONE',  ( 804.4286716492782716, -209.3618753856926276, -345.3141322388244703 ) ) ;
#17463 = CARTESIAN_POINT ( 'NONE',  ( 781.7834795799800531, -394.8164208402374697, 315.0636971347436202 ) ) ;
#17464 = CARTESIAN_POINT ( 'NONE',  ( 763.0537975583475827, -96.45278447660203369, -371.0346526505627480 ) ) ;
#17465 = MANIFOLD_SOLID_BREP ( 'Fillet1', #37218 ) ;
#17466 = CARTESIAN_POINT ( 'NONE',  ( 755.5713283507202505, -101.3618753856929544, -334.6858677611754729 ) ) ;
#17467 = ORIENTED_EDGE ( 'NONE', *, *, #36014, .F. ) ;
#17468 = CIRCLE ( 'NONE', #15973, 10.00000000000000888 ) ;
#17469 = CARTESIAN_POINT ( 'NONE',  ( 755.5913626894240451, -373.6454272087887034, -346.6156483768012890 ) ) ;
#17471 = CARTESIAN_POINT ( 'NONE',  ( 804.1105419155481968, -435.8272453906066062, 347.6308680596136469 ) ) ;
#17470 = CARTESIAN_POINT ( 'NONE',  ( 794.9819416627830151, -132.9982390220564810, 319.9864689768909898 ) ) ;
#17472 = CARTESIAN_POINT ( 'NONE',  ( 790.8726784830453198, -130.7146871989599504, 362.5472867521010585 ) ) ;
#17473 = VECTOR ( 'NONE', #21107, 1000.000000000000114 ) ;
#17476 = CARTESIAN_POINT ( 'NONE',  ( 744.8212110874229666, -402.8965053807773415, 336.2046728542121627 ) ) ;
#17475 = CARTESIAN_POINT ( 'NONE',  ( 799.9999999999993179, 205.0000000000000568, -339.9999999999999432 ) ) ;
#17474 = CARTESIAN_POINT ( 'NONE',  ( 829.9999999999992042, 529.9999999999997726, -320.0000000000000000 ) ) ;
#17477 = VERTEX_POINT ( 'NONE', #38605 ) ;
#17478 = CARTESIAN_POINT ( 'NONE',  ( 759.0159684113467620, -352.9181544815159555, -325.8855110935213020 ) ) ;
#17479 = CARTESIAN_POINT ( 'NONE',  ( 791.9812246680005501, -356.6346026584193964, -361.9419747391813189 ) ) ;
#17480 = VECTOR ( 'NONE', #11748, 1000.000000000000000 ) ;
#17481 = CARTESIAN_POINT ( 'NONE',  ( 783.7953271457878373, -176.1908817542438328, -375.1787889125761239 ) ) ;
#17482 = CARTESIAN_POINT ( 'NONE',  ( 788.6739635108323228, -31.64542720878970883, 373.9316612368139090 ) ) ;
#17483 = VECTOR ( 'NONE', #42742, 1000.000000000000000 ) ;
#17485 = CARTESIAN_POINT ( 'NONE',  ( 911.9999999999993179, 219.9999999999998863, -350.0000000000000000 ) ) ;
#17484 = FACE_OUTER_BOUND ( 'NONE', #3662, .T. ) ;
#17486 = CARTESIAN_POINT ( 'NONE',  ( 786.6156483768007774, -289.4419599262321299, -315.5913626894246136 ) ) ;
#17487 = LINE ( 'NONE', #28557, #45401 ) ;
#17488 = CARTESIAN_POINT ( 'NONE',  ( 752.7379699480933368, -156.0090635724256742, -361.9858362298580232 ) ) ;
#17489 = CARTESIAN_POINT ( 'NONE',  ( -786.4999999999993179, -513.1383975375929367, -369.9999999999999432 ) ) ;
#17490 = DIRECTION ( 'NONE',  ( -1.000000000000000000, -0.000000000000000000, -0.000000000000000000 ) ) ;
#17491 = CIRCLE ( 'NONE', #31484, 50.00000000000004263 ) ;
#17492 = CARTESIAN_POINT ( 'NONE',  ( 796.9571628226829034, -383.4636090269704596, 321.2382568024804641 ) ) ;
#17493 = CARTESIAN_POINT ( 'NONE',  ( 799.9636004259356241, -334.9181544815160692, 311.2241431872006956 ) ) ;
#17494 = CARTESIAN_POINT ( 'NONE',  ( 782.5225473063383106, -190.2709662947835625, -375.2698199232970637 ) ) ;
#17495 = LINE ( 'NONE', #41978, #41588 ) ;
#17496 = CARTESIAN_POINT ( 'NONE',  ( 745.5313806188320314, -135.2817908451530116, 333.7943932421247268 ) ) ;
#17497 = CARTESIAN_POINT ( 'NONE',  ( 812.7932403749906598, -351.1800572038740142, -327.7687537140311633 ) ) ;
#17498 = CARTESIAN_POINT ( 'NONE',  ( 928.0249999999991815, 154.9999999999998863, -360.0000000000000000 ) ) ;
#17499 = DIRECTION ( 'NONE',  ( -0.000000000000000000, 1.000000000000000000, -0.000000000000000000 ) ) ;
#17500 = CARTESIAN_POINT ( 'NONE',  ( 778.2165204200184689, -190.8164208402381234, 364.9363028652563230 ) ) ;
#17501 = VERTEX_POINT ( 'NONE', #6962 ) ;
#17502 = CARTESIAN_POINT ( 'NONE',  ( 811.3240766477731540, -412.3726999360612808, 355.6651683502462902 ) ) ;
#17503 = CARTESIAN_POINT ( 'NONE',  ( 812.6845335610512393, -391.9874144716864066, -353.5525998758768651 ) ) ;
#17504 = AXIS2_PLACEMENT_3D ( 'NONE', #17548, #39027, #21920 ) ;
#17505 = CARTESIAN_POINT ( 'NONE',  ( 787.5162901302840055, -107.3618753856928976, -305.4481719005792684 ) ) ;
#17506 = CARTESIAN_POINT ( 'NONE',  ( 782.5225473063381969, -430.2709662947827383, -375.2698199232970637 ) ) ;
#17507 = LINE ( 'NONE', #17038, #34264 ) ;
#17508 = CARTESIAN_POINT ( 'NONE',  ( 781.2497674668890113, 11.64894916467595642, 375.3608509340180603 ) ) ;
#17509 = ORIENTED_EDGE ( 'NONE', *, *, #32525, .T. ) ;
#17510 = CARTESIAN_POINT ( 'NONE',  ( 768.8385539511368734, -167.2601417444143976, -306.4236121716840557 ) ) ;
#17511 = FACE_OUTER_BOUND ( 'NONE', #1599, .T. ) ;
#17512 = CARTESIAN_POINT ( 'NONE',  ( 747.3154664389472828, -307.9874144716866340, 326.4474001241230781 ) ) ;
#17513 = CARTESIAN_POINT ( 'NONE',  ( 788.8264449731201466, -117.1800572038747106, 363.6646147819170665 ) ) ;
#17514 = EDGE_LOOP ( 'NONE', ( #39749, #1941, #45221, #43559 ) ) ;
#17515 = VECTOR ( 'NONE', #41420, 1000.000000000000000 ) ;
#17516 = CARTESIAN_POINT ( 'NONE',  ( 765.0180583372156207, -144.9982390220564525, -360.0135310231089534 ) ) ;
#17517 = CARTESIAN_POINT ( 'NONE',  ( 797.8594530101008786, -301.5436935675105588, 322.1405469898980982 ) ) ;
#17518 = AXIS2_PLACEMENT_3D ( 'NONE', #8005, #39188, #18847 ) ;
#17519 = CARTESIAN_POINT ( 'NONE',  ( 787.5162901302840055, -11.36187538569323863, -305.4481719005792684 ) ) ;
#17520 = EDGE_CURVE ( 'NONE', #35282, #32688, #34801, .T. ) ;
#17521 = CARTESIAN_POINT ( 'NONE',  ( 789.8509095638472672, -449.0441647919901698, 365.1129080010174448 ) ) ;
#17522 = EDGE_LOOP ( 'NONE', ( #12359, #14746, #42525 ) ) ;
#17523 = CARTESIAN_POINT ( 'NONE',  ( 805.6418435158337843, -413.4636090269704027, -363.8556311672236916 ) ) ;
#17524 = ORIENTED_EDGE ( 'NONE', *, *, #6286, .F. ) ;
#17525 = APPLICATION_PROTOCOL_DEFINITION ( 'draft international standard', 'automotive_design', 1998, #4845 ) ;
#17526 = CARTESIAN_POINT ( 'NONE',  ( 804.6798772138708955, -15.72551174932958951, 334.6312213355107019 ) ) ;
#17527 = CARTESIAN_POINT ( 'NONE',  ( 774.6858677611749044, -273.7255117493288026, -315.5713283507209894 ) ) ;
#17529 = CARTESIAN_POINT ( 'NONE',  ( 813.2346286133761168, -245.2601417444141987, 328.9521613784389160 ) ) ;
#17528 = CARTESIAN_POINT ( 'NONE',  ( 804.7487373415286811, -355.5436935675103882, 364.7487373415288516 ) ) ;
#17530 = CARTESIAN_POINT ( 'NONE',  ( 752.4576283171824116, -69.07832356259653750, 317.7880784355627952 ) ) ;
#17531 = CARTESIAN_POINT ( 'NONE',  ( 776.9254006560222479, -260.1908817542435486, -314.8983024940802125 ) ) ;
#17532 = CARTESIAN_POINT ( 'NONE',  ( 804.6798772138708955, -255.7255117493287742, -334.6312213355107019 ) ) ;
#17533 = CARTESIAN_POINT ( 'NONE',  ( 809.6099558218720631, -452.9681489794449476, -335.1781210895659342 ) ) ;
#17534 = CARTESIAN_POINT ( 'NONE',  ( 771.1735550268778070, -129.1800572038746111, -316.3353852180827630 ) ) ;
#17535 = CARTESIAN_POINT ( 'NONE',  ( 792.1044303154645831, -252.4527844766015789, 317.8323909638837677 ) ) ;
#17536 = CARTESIAN_POINT ( 'NONE',  ( 763.0537975583475827, -384.4527844766011526, 371.0346526505627480 ) ) ;
#17537 = CARTESIAN_POINT ( 'NONE',  ( 1820.038553321469863, -589.9999999999998863, 210.0000000000000000 ) ) ;
#17538 = CARTESIAN_POINT ( 'NONE',  ( 804.1009440267234822, -47.46360902697148987, -314.0944755984392600 ) ) ;
#17539 = FACE_OUTER_BOUND ( 'NONE', #20045, .T. ) ;
#17540 = LINE ( 'NONE', #6895, #35649 ) ;
#17541 = CARTESIAN_POINT ( 'NONE',  ( 796.1575198192839480, -246.0090635724253900, 359.4546378042384163 ) ) ;
#17542 = APPLICATION_CONTEXT ( 'automotive_design' ) ;
#17543 = CARTESIAN_POINT ( 'NONE',  ( 771.1735550268778070, -105.1800572038747248, 316.3353852180827630 ) ) ;
#17544 = ORIENTED_EDGE ( 'NONE', *, *, #5098, .F. ) ;
#17545 = CARTESIAN_POINT ( 'NONE',  ( 787.5531968255692163, -21.82724539060792424, -316.1348686366205811 ) ) ;
#17546 = CARTESIAN_POINT ( 'NONE',  ( 815.2698199232962679, -112.8164208402383650, -342.5225473063383674 ) ) ;
#17547 = CARTESIAN_POINT ( 'NONE',  ( 756.1348686366196716, -305.2601417444139429, 347.5531968255698416 ) ) ;
#17548 = CARTESIAN_POINT ( 'NONE',  ( 181.1634899080285948, 240.0000000000000284, -199.9999999999953957 ) ) ;
#17549 = CARTESIAN_POINT ( 'NONE',  ( 764.1737431748507561, -34.37269993606243901, 371.6461892240376415 ) ) ;
#17550 = CARTESIAN_POINT ( 'NONE',  ( 758.8095938919642549, -224.0891481129653187, -311.6929314249763365 ) ) ;
#17551 = CARTESIAN_POINT ( 'NONE',  ( 767.7687537140311633, -191.9073299311471885, 372.7932403749916830 ) ) ;
#17552 = CARTESIAN_POINT ( 'NONE',  ( 768.0187753319979720, -80.63460265842029173, 318.0580252608186242 ) ) ;
#17553 = CARTESIAN_POINT ( 'NONE',  ( 831.1634899080286232, 256.4999999999998863, -202.7499999999998863 ) ) ;
#17554 = CARTESIAN_POINT ( 'NONE',  ( 811.6461892240364477, -268.7146871989595525, -324.1737431748509835 ) ) ;
#17555 = CARTESIAN_POINT ( 'NONE',  ( 780.5236548040995785, 3.263663700301089765, 314.9735926884559944 ) ) ;
#17556 = CARTESIAN_POINT ( 'NONE',  ( 772.4837098697144029, -311.3618753856922581, -374.5518280994205611 ) ) ;
#17557 = CARTESIAN_POINT ( 'NONE',  ( 989.9999999999992042, -418.3138125091626307, -201.9999999999998010 ) ) ;
#17558 = CARTESIAN_POINT ( 'NONE',  ( 756.1348686366196716, -353.2601417444137724, 347.5531968255698416 ) ) ;
#17559 = CARTESIAN_POINT ( 'NONE',  ( 814.9108240113580450, -40.27096629478405987, 337.5031285880265273 ) ) ;
#17560 = CARTESIAN_POINT ( 'NONE',  ( 788.7366044899766848, -371.9073299311465917, -316.5762568750059813 ) ) ;
#17561 = CARTESIAN_POINT ( 'NONE',  ( 755.8398074228967971, -67.44195992623289726, 333.4516893846970333 ) ) ;
#17562 = CARTESIAN_POINT ( 'NONE',  ( 807.5423716828161105, -57.07832356259658013, -362.2119215644372048 ) ) ;
#17563 = CARTESIAN_POINT ( 'NONE',  ( 783.0433043558608688, -192.8965053807779668, -315.1538015810313027 ) ) ;
#17564 = CARTESIAN_POINT ( 'NONE',  ( 758.0141637701419768, -207.0783235625960685, 367.2620300519063790 ) ) ;
#17565 = CARTESIAN_POINT ( 'NONE',  ( 755.5713283507202505, -5.361875385693257279, 334.6858677611754729 ) ) ;
#17566 = ORIENTED_EDGE ( 'NONE', *, *, #39078, .T. ) ;
#17567 = CARTESIAN_POINT ( 'NONE',  ( 769.1273215169530886, -190.7146871989597798, -317.4527132478988847 ) ) ;
#17568 = CARTESIAN_POINT ( 'NONE',  ( 805.1927285166397041, -208.8164208402380666, 341.8018195045277707 ) ) ;
#17569 = EDGE_CURVE ( 'NONE', #32576, #8421, #15621, .T. ) ;
#17570 = CARTESIAN_POINT ( 'NONE',  ( 752.4576283171824116, -45.07832356259660145, -317.7880784355627952 ) ) ;
#17571 = CARTESIAN_POINT ( 'NONE',  ( 764.8639956371174549, -344.0891481129648355, 319.7806653035542581 ) ) ;
#17572 = CARTESIAN_POINT ( 'NONE',  ( 914.9999999999992042, 74.99999999999984368, -350.0000000000000000 ) ) ;
#17573 = ORIENTED_EDGE ( 'NONE', *, *, #25815, .T. ) ;
#17574 = CARTESIAN_POINT ( 'NONE',  ( 796.7845633553578182, -57.62377810805111267, 358.5707757039688204 ) ) ;
#17575 = CARTESIAN_POINT ( 'NONE',  ( 797.8822607201568644, -318.5545181178796952, -370.1134526219340160 ) ) ;
#17576 = AXIS2_PLACEMENT_3D ( 'NONE', #17572, #31643, #234 ) ;
#17577 = CARTESIAN_POINT ( 'NONE',  ( 814.5518280994195948, -255.7255117493287742, 332.4837098697145166 ) ) ;
#17578 = CARTESIAN_POINT ( 'NONE',  ( 776.2433038121456548, -12.89650538077851216, 374.8207195650711014 ) ) ;
#17579 = CARTESIAN_POINT ( 'NONE',  ( 760.7433823573367135, -156.0090635724256742, -355.9930595647440441 ) ) ;
#17580 = CARTESIAN_POINT ( 'NONE',  ( 762.3223304703356007, -151.5436935675109851, -322.3223304703362828 ) ) ;
#17581 = CARTESIAN_POINT ( 'NONE',  ( 759.9864689768902508, -362.0891481129648923, -354.9819416627836404 ) ) ;
#17582 = ORIENTED_EDGE ( 'NONE', *, *, #43051, .T. ) ;
#17583 = CARTESIAN_POINT ( 'NONE',  ( 813.1304606946830518, -305.9073299311467622, 352.3570229623690580 ) ) ;
#17584 = CYLINDRICAL_SURFACE ( 'NONE', #24043, 2.749999999999835687 ) ;
#17585 = CARTESIAN_POINT ( 'NONE',  ( 790.8726784830453198, -322.7146871989593819, 362.5472867521010585 ) ) ;
#17586 = DIRECTION ( 'NONE',  ( 0.000000000000000000, 0.000000000000000000, 1.000000000000000000 ) ) ;
#17587 = CARTESIAN_POINT ( 'NONE',  ( 804.8461984189677878, -146.1908817542438896, 336.9566956441385628 ) ) ;
#17588 = CARTESIAN_POINT ( 'NONE',  ( 762.1405469898971887, -25.54369356751136877, 357.8594530101015607 ) ) ;
#17589 = VERTEX_POINT ( 'NONE', #4426 ) ;
#17590 = CARTESIAN_POINT ( 'NONE',  ( 749.5768839229115201, -372.5545181178796383, -358.0661480581553064 ) ) ;
#17591 = CARTESIAN_POINT ( 'NONE',  ( 989.9999999999992042, 469.9999999999999432, 360.0000000000000000 ) ) ;
#17592 = CARTESIAN_POINT ( 'NONE',  ( 755.8990559732751535, -251.4636090269709143, 365.9055244015606831 ) ) ;
#17593 = CARTESIAN_POINT ( 'NONE',  ( 800.7704444035546203, -172.1692326535052757, 326.0291762391768771 ) ) ;
#17594 = CARTESIAN_POINT ( 'NONE',  ( 805.1927285166397041, -376.8164208402375834, -341.8018195045277707 ) ) ;
#17595 = CARTESIAN_POINT ( 'NONE',  ( 799.9999999999993179, 205.0000000000000568, -319.9999999999999432 ) ) ;
#17596 = CARTESIAN_POINT ( 'NONE',  ( 773.4516893846965786, -211.6454272087891582, -315.8398074228977066 ) ) ;
#17597 = CARTESIAN_POINT ( 'NONE',  ( 755.2512626584698410, -31.54369356751135456, 315.2512626584710915 ) ) ;
#17598 = CARTESIAN_POINT ( 'NONE',  ( 777.5031285880264704, -70.81642084023850714, 374.9108240113588408 ) ) ;
#17599 = CARTESIAN_POINT ( 'NONE',  ( 808.1998602359702772, -452.9681489794448908, 337.6500903519150825 ) ) ;
#17600 = CARTESIAN_POINT ( 'NONE',  ( 777.5031285880264704, -430.8164208402374129, -374.9108240113588408 ) ) ;
#17601 = DIRECTION ( 'NONE',  ( 0.000000000000000000, 0.000000000000000000, -1.000000000000000000 ) ) ;
#17602 = AXIS2_PLACEMENT_3D ( 'NONE', #40345, #9530, #41176 ) ;
#17603 = CARTESIAN_POINT ( 'NONE',  ( 747.6481478633932056, -349.0999726633342561, 353.4146539503763620 ) ) ;
#17604 = DIRECTION ( 'NONE',  ( 0.000000000000000000, -1.000000000000000000, 0.000000000000000000 ) ) ;
#17605 = CARTESIAN_POINT ( 'NONE',  ( 800.9747183278959710, -324.9982390220559409, 311.9810565676471583 ) ) ;
#17606 = CARTESIAN_POINT ( 'NONE',  ( 758.8095938919642549, -56.08914811296580893, -311.6929314249763365 ) ) ;
#17607 = CARTESIAN_POINT ( 'NONE',  ( 762.3223304703356007, -271.5436935675106156, -322.3223304703362828 ) ) ;
#17608 = EDGE_CURVE ( 'NONE', #10339, #25758, #36279, .T. ) ;
#17609 = FACE_OUTER_BOUND ( 'NONE', #1267, .T. ) ;
#17610 = CARTESIAN_POINT ( 'NONE',  ( 781.8018195045266339, -382.2709662947828519, 365.1927285166406705 ) ) ;
#17611 = CARTESIAN_POINT ( 'NONE',  ( 796.9571628226829034, -167.4636090269711133, 321.2382568024804641 ) ) ;
#17612 = CARTESIAN_POINT ( 'NONE',  ( 768.9521613784389729, -33.82724539060788516, -373.2346286133773106 ) ) ;
#17613 = CARTESIAN_POINT ( 'NONE',  ( 804.1601925771018387, -79.44195992623286884, -346.5483106153029098 ) ) ;
#17614 = CARTESIAN_POINT ( 'NONE',  ( 758.0141637701419768, -87.07832356259646645, 367.2620300519063790 ) ) ;
#17615 = CARTESIAN_POINT ( 'NONE',  ( 774.6858677611749044, -393.7255117493283478, 315.5713283507209894 ) ) ;
#17616 = CARTESIAN_POINT ( 'NONE',  ( 813.1304606946831655, 6.092670068852160448, 352.3570229623691716 ) ) ;
#17617 = CARTESIAN_POINT ( 'NONE',  ( 181.1634899080285948, 260.0000000000000000, -199.9999999999953957 ) ) ;
#17618 = CARTESIAN_POINT ( 'NONE',  ( 808.7758568127978833, -148.1692326535053610, 320.0363995740631822 ) ) ;
#17619 = CARTESIAN_POINT ( 'NONE',  ( 765.0180583372156207, -0.9982390220569063999, -360.0135310231089534 ) ) ;
#17621 = ORIENTED_EDGE ( 'NONE', *, *, #21591, .T. ) ;
#17620 = CARTESIAN_POINT ( 'NONE',  ( 784.0799538623451781, -107.8055962898691433, -364.6971507214555572 ) ) ;
#17622 = CARTESIAN_POINT ( 'NONE',  ( 795.1360043628807261, -68.08914811296575920, -360.2193346964456282 ) ) ;
#17623 = ADVANCED_FACE ( 'NONE', ( #7652 ), #28436, .F. ) ;
#17624 = ADVANCED_FACE ( 'NONE', ( #17821 ), #937, .T. ) ;
#17625 = CARTESIAN_POINT ( 'NONE',  ( 798.7617431975189675, -387.6237781080499758, -323.0428371773161871 ) ) ;
#17627 = CARTESIAN_POINT ( 'NONE',  ( 801.9419747391806368, -210.4527844766016926, 351.9812246680014027 ) ) ;
#17626 = CARTESIAN_POINT ( 'NONE',  ( 794.9819416627830151, -228.9982390220561683, 319.9864689768909898 ) ) ;
#17628 = EDGE_LOOP ( 'NONE', ( #42680, #20843, #15409, #29655 ) ) ;
#17629 = CARTESIAN_POINT ( 'NONE',  ( 813.2346286133761168, -389.2601417444136018, -328.9521613784389160 ) ) ;
#17630 = CARTESIAN_POINT ( 'NONE',  ( 787.4397851343537695, 2.274488250670355871, 374.2001403089903988 ) ) ;
#17631 = DIRECTION ( 'NONE',  ( -0.000000000000000000, -0.000000000000000000, 1.000000000000000000 ) ) ;
#17632 = EDGE_LOOP ( 'NONE', ( #21999, #40693, #29995, #38908 ) ) ;
#17633 = CARTESIAN_POINT ( 'NONE',  ( 762.1405469898971887, -433.5436935675099903, 357.8594530101015607 ) ) ;
#17634 = ORIENTED_EDGE ( 'NONE', *, *, #711, .F. ) ;
#17635 =( LENGTH_UNIT ( ) NAMED_UNIT ( * ) SI_UNIT ( .MILLI., .METRE. ) );
#17636 = CARTESIAN_POINT ( 'NONE',  ( 747.2067596250078623, -243.1800572038743269, -352.2312462859687230 ) ) ;
#17637 = CARTESIAN_POINT ( 'NONE',  ( 801.1904061080338124, -140.0891481129655176, 368.3070685750236066 ) ) ;
#17638 = ORIENTED_EDGE ( 'NONE', *, *, #521, .F. ) ;
#17639 = CARTESIAN_POINT ( 'NONE',  ( 746.0683387631852383, -187.4419599262325278, 331.3260364891676204 ) ) ;
#17640 = CARTESIAN_POINT ( 'NONE',  ( 757.8323909638828582, -242.6346026584197659, -352.1044303154654358 ) ) ;
#17641 = ORIENTED_EDGE ( 'NONE', *, *, #33400, .T. ) ;
#17642 = EDGE_CURVE ( 'NONE', #14449, #27904, #25185, .T. ) ;
#17643 = VECTOR ( 'NONE', #25433, 1000.000000000000114 ) ;
#17644 = CARTESIAN_POINT ( 'NONE',  ( 791.9812246680005501, -356.6346026584193964, -361.9419747391813189 ) ) ;
#17645 = CARTESIAN_POINT ( 'NONE',  ( 788.8264449731200330, -21.18005720387502677, -363.6646147819171233 ) ) ;
#17646 = EDGE_CURVE ( 'NONE', #34942, #31246, #260, .T. ) ;
#17647 = CARTESIAN_POINT ( 'NONE',  ( 803.8651313633788504, -221.2601417444142271, 332.4468031744301015 ) ) ;
#17648 = DIRECTION ( 'NONE',  ( 5.551115123125783688E-16, 1.000000000000000000, 0.000000000000000000 ) ) ;
#17649 = DIRECTION ( 'NONE',  ( 0.000000000000000000, 0.000000000000000000, 1.000000000000000000 ) ) ;
#17650 = ORIENTED_EDGE ( 'NONE', *, *, #22976, .F. ) ;
#17651 = CARTESIAN_POINT ( 'NONE',  ( 762.3223304703356007, -31.54369356751135456, -322.3223304703362828 ) ) ;
#17652 = CARTESIAN_POINT ( 'NONE',  ( 701.1634899080286232, 259.9999999999999432, -199.9999999999990337 ) ) ;
#17653 = CARTESIAN_POINT ( 'NONE',  ( 879.9999999999992042, 99.99999999999984368, -360.0000000000000000 ) ) ;
#17654 = ORIENTED_EDGE ( 'NONE', *, *, #34495, .T. ) ;
#17655 = CARTESIAN_POINT ( 'NONE',  ( 815.3608509340175488, -266.7363362996981095, -341.2497674668889545 ) ) ;
#17656 = CARTESIAN_POINT ( 'NONE',  ( 805.6418435158337843, -149.4636090269711417, 363.8556311672236916 ) ) ;
#17658 = CARTESIAN_POINT ( 'NONE',  ( 771.2633955100217236, -239.9073299311470748, -363.4237431249939618 ) ) ;
#17657 = CARTESIAN_POINT ( 'NONE',  ( 311.1634899080286232, 256.5000000000000000, -202.7499999999962483 ) ) ;
#17659 = CARTESIAN_POINT ( 'NONE',  ( 763.2154366446407039, -381.6237781080500326, -321.4292242960311228 ) ) ;
#17660 = SURFACE_STYLE_FILL_AREA ( #6338 ) ;
#17661 = CARTESIAN_POINT ( 'NONE',  ( 779.4763451958990572, -128.7363362996984790, -365.0264073115438919 ) ) ;
#17662 = DIRECTION ( 'NONE',  ( 0.000000000000000000, 0.000000000000000000, 1.000000000000000000 ) ) ;
#17663 = CARTESIAN_POINT ( 'NONE',  ( 751.2241431872005251, 7.830767346494148740, -359.9636004259367610 ) ) ;
#17664 = CARTESIAN_POINT ( 'NONE',  ( 792.2312462859673587, -299.9073299311468759, -307.2067596250082602 ) ) ;
#17665 = FACE_OUTER_BOUND ( 'NONE', #22321, .T. ) ;
#17666 = CARTESIAN_POINT ( 'NONE',  ( 765.0180583372156207, -0.9982390220569063999, 360.0135310231089534 ) ) ;
#17667 = CARTESIAN_POINT ( 'NONE',  ( 795.1360043628807261, -68.08914811296575920, -360.2193346964456282 ) ) ;
#17668 = EDGE_CURVE ( 'NONE', #9428, #32578, #43638, .T. ) ;
#17669 = CARTESIAN_POINT ( 'NONE',  ( 776.2046728542105711, -260.1908817542435486, 304.8212110874238761 ) ) ;
#17670 = CARTESIAN_POINT ( 'NONE',  ( 778.7502325331095108, -216.3510508353233490, -304.6391490659818828 ) ) ;
#17671 = CARTESIAN_POINT ( 'NONE',  ( 787.5162901302840055, -227.3618753856925707, 305.4481719005792684 ) ) ;
#17672 = CARTESIAN_POINT ( 'NONE',  ( 787.5162901302840055, -443.3618753856917465, -305.4481719005792684 ) ) ;
#17673 = CARTESIAN_POINT ( 'NONE',  ( 879.9999999999992042, 239.9999999999998863, -244.9999999999999716 ) ) ;
#17674 = ADVANCED_FACE ( 'NONE', ( #22186 ), #3733, .F. ) ;
#17675 = CARTESIAN_POINT ( 'NONE',  ( 767.8955696845333705, -288.4527844766014937, 362.1676090361162323 ) ) ;
#17676 = CARTESIAN_POINT ( 'NONE',  ( 798.5707757039680246, -77.46360902697138329, 356.7845633553585003 ) ) ;
#17677 = CARTESIAN_POINT ( 'NONE',  ( 788.7366044899766848, -443.9073299311464780, -316.5762568750059813 ) ) ;
#17678 = CIRCLE ( 'NONE', #19151, 30.00000000000008171 ) ;
#17679 = CARTESIAN_POINT ( 'NONE',  ( 355.8971257818259915, 290.0000000000001137, -244.9999999999999716 ) ) ;
#17680 = DIRECTION ( 'NONE',  ( -1.880165489482579047E-16, -1.000000000000000000, -0.000000000000000000 ) ) ;
#17682 = CARTESIAN_POINT ( 'NONE',  ( 764.8639956371174549, -344.0891481129647786, 319.7806653035542013 ) ) ;
#17681 = CARTESIAN_POINT ( 'NONE',  ( 804.1601925771018387, -127.4419599262326983, 346.5483106153029098 ) ) ;
#17683 = ORIENTED_EDGE ( 'NONE', *, *, #17041, .F. ) ;
#17684 = EDGE_CURVE ( 'NONE', #27240, #22001, #11930, .T. ) ;
#17685 = CARTESIAN_POINT ( 'NONE',  ( 796.7845633553578182, -297.6237781080502600, -358.5707757039688204 ) ) ;
#17686 = CARTESIAN_POINT ( 'NONE',  ( 800.2193346964447755, -90.99823902205663728, 355.1360043628815788 ) ) ;
#17687 = CARTESIAN_POINT ( 'NONE',  ( 745.1769319972822814, -305.8055962898684470, -346.2694204179732083 ) ) ;
#17688 = DIRECTION ( 'NONE',  ( 0.000000000000000000, -0.3826834323650838421, -0.9238795325112891810 ) ) ;
#17689 = CARTESIAN_POINT ( 'NONE',  ( 814.8230680027162407, -413.8055962898681059, 333.7305795820267917 ) ) ;
#17690 = ORIENTED_EDGE ( 'NONE', *, *, #15853, .F. ) ;
#17691 = CARTESIAN_POINT ( 'NONE',  ( 794.9819416627830151, -324.9982390220559409, 319.9864689768909898 ) ) ;
#17692 = CARTESIAN_POINT ( 'NONE',  ( 795.9930595647434757, -51.07832356259657303, -320.7433823573372820 ) ) ;
#17693 = CARTESIAN_POINT ( 'NONE',  ( 805.1927285166397041, -160.8164208402382371, -341.8018195045277707 ) ) ;
#17694 = CARTESIAN_POINT ( 'NONE',  ( 791.9812246680005501, -212.6346026584198796, -361.9419747391813189 ) ) ;
#17695 = CARTESIAN_POINT ( 'NONE',  ( 768.0187753319979720, -416.6346026584192259, 318.0580252608186242 ) ) ;
#17696 = CARTESIAN_POINT ( 'NONE',  ( 787.5162901302840055, -131.3618753856928834, -305.4481719005792684 ) ) ;
#17697 = MANIFOLD_SOLID_BREP ( 'Body-Move/Copy1', #30602 ) ;
#17698 = CARTESIAN_POINT ( 'NONE',  ( 785.3687786644885591, -131.3618753856928549, -315.3201227861280813 ) ) ;
#17699 = EDGE_LOOP ( 'NONE', ( #10407, #18497, #1687, #27644 ) ) ;
#17700 = CARTESIAN_POINT ( 'NONE',  ( 802.5472867521000353, -388.3726999360613945, -350.8726784830461156 ) ) ;
#17702 = CARTESIAN_POINT ( 'NONE',  ( 802.9823548866075953, -433.0999726633339151, 330.0799878456151077 ) ) ;
#17701 = CARTESIAN_POINT ( 'NONE',  ( 767.8955696845333705, -120.4527844766019484, 362.1676090361162323 ) ) ;
#17703 = CARTESIAN_POINT ( 'NONE',  ( 789.9200121543843807, -121.9874144716872593, 317.0176451133914384 ) ) ;
#17706 = CARTESIAN_POINT ( 'NONE',  ( 746.0683387631852383, -379.4419599262318457, 331.3260364891676204 ) ) ;
#17705 = DIRECTION ( 'NONE',  ( 0.000000000000000000, 0.000000000000000000, -1.000000000000000000 ) ) ;
#17704 = CARTESIAN_POINT ( 'NONE',  ( 791.7608162188021197, 205.0000000000000568, 329.9999999999999432 ) ) ;
#17707 = VERTEX_POINT ( 'NONE', #14356 ) ;
#17708 = CARTESIAN_POINT ( 'NONE',  ( 799.2566176426618085, -384.0090635724249637, -324.0069404352559559 ) ) ;
#17709 = CARTESIAN_POINT ( 'NONE',  ( 756.5762568750052424, -363.1800572038739006, -348.7366044899774238 ) ) ;
#17710 = CARTESIAN_POINT ( 'NONE',  ( 788.6739635108323228, -175.6454272087892718, -373.9316612368139090 ) ) ;
#17711 = CARTESIAN_POINT ( 'NONE',  ( 802.2119215644370342, -30.00906357242607925, 367.5423716828165084 ) ) ;
#17713 = CARTESIAN_POINT ( 'NONE',  ( 879.9999999999990905, 479.9999999999998863, 210.0000000000000000 ) ) ;
#17712 = CARTESIAN_POINT ( 'NONE',  ( 190.7583438952259485, 394.6698570112193920, -274.9999999999999432 ) ) ;
#17714 = CARTESIAN_POINT ( 'NONE',  ( 755.5713283507202505, -437.3618753856919170, -334.6858677611754729 ) ) ;
#17715 = CARTESIAN_POINT ( 'NONE',  ( 810.4231160770870019, -168.5545181178802352, -321.9338519418446936 ) ) ;
#17716 = CARTESIAN_POINT ( 'NONE',  ( 786.4999999999993179, -513.1383975375929367, -369.9999999999999432 ) ) ;
#17717 = CARTESIAN_POINT ( 'NONE',  ( 1238.921997096861332, 240.0000000000000853, -360.0000000000000000 ) ) ;
#17718 = CARTESIAN_POINT ( 'NONE',  ( 761.4292242960306112, -353.4636090269705733, 323.2154366446414429 ) ) ;
#17719 = CARTESIAN_POINT ( 'NONE',  ( 760.0363995740630116, -322.9181544815161260, 368.7758568127991907 ) ) ;
#17720 = CARTESIAN_POINT ( 'NONE',  ( 751.6929314249750860, -198.9982390220562536, -318.8095938919659034 ) ) ;
#17721 = LINE ( 'NONE', #34343, #33434 ) ;
#17722 = DIRECTION ( 'NONE',  ( 0.000000000000000000, 0.000000000000000000, 1.000000000000000000 ) ) ;
#17723 = EDGE_CURVE ( 'NONE', #32851, #66, #32132, .T. ) ;
#17724 = CARTESIAN_POINT ( 'NONE',  ( 745.1792804349281596, -158.1908817542438612, 343.7566961878542884 ) ) ;
#17725 = CARTESIAN_POINT ( 'NONE',  ( 764.3348316497523456, -94.71468719896007826, -308.6759233522265617 ) ) ;
#17726 = CARTESIAN_POINT ( 'NONE',  ( 808.0189434323515343, -86.08914811296573077, 319.0252816721025511 ) ) ;
#17727 = CARTESIAN_POINT ( 'NONE',  ( 792.3570229623688874, -333.1800572038740142, -373.1304606946836202 ) ) ;
#17728 = FACE_OUTER_BOUND ( 'NONE', #20050, .T. ) ;
#17729 = CARTESIAN_POINT ( 'NONE',  ( 759.9999999999992042, 205.0000000000000568, -339.9999999999999432 ) ) ;
#17730 = CARTESIAN_POINT ( 'NONE',  ( 767.8955696845333705, -192.4527844766016926, 362.1676090361162323 ) ) ;
#17731 = CARTESIAN_POINT ( 'NONE',  ( 814.4686193811664907, -459.2817908451519884, 346.2056067578752732 ) ) ;
#17732 = CARTESIAN_POINT ( 'NONE',  ( 745.1769319972822814, -425.8055962898680491, -346.2694204179732083 ) ) ;
#17733 = CARTESIAN_POINT ( 'NONE',  ( 777.5031285880264704, -142.8164208402382656, -374.9108240113588408 ) ) ;
#17734 = CARTESIAN_POINT ( 'NONE',  ( 777.5031285880264704, -406.8164208402375266, -374.9108240113588408 ) ) ;
#17735 = DIRECTION ( 'NONE',  ( 0.000000000000000000, 0.000000000000000000, -1.000000000000000000 ) ) ;
#17736 = CARTESIAN_POINT ( 'NONE',  ( 807.5423716828161105, 14.92167643740321381, 362.2119215644372048 ) ) ;
#17737 = EDGE_LOOP ( 'NONE', ( #22280, #24090 ) ) ;
#17738 = EDGE_CURVE ( 'NONE', #19609, #16032, #25663, .T. ) ;
#17739 = CARTESIAN_POINT ( 'NONE',  ( 810.1134526219336749, -176.5328690171416213, -357.8822607201570349 ) ) ;
#17740 = LINE ( 'NONE', #20509, #40303 ) ;
#17741 = CARTESIAN_POINT ( 'NONE',  ( 812.6845335610512393, -319.9874144716866340, 353.5525998758768651 ) ) ;
#17742 = CARTESIAN_POINT ( 'NONE',  ( 764.8639956371174549, -128.0891481129655745, 319.7806653035542581 ) ) ;
#17743 = ORIENTED_EDGE ( 'NONE', *, *, #45522, .T. ) ;
#17744 = CARTESIAN_POINT ( 'NONE',  ( 803.6646147819161570, -305.9073299311467622, 348.8264449731210561 ) ) ;
#17745 = CARTESIAN_POINT ( 'NONE',  ( 782.4968714119720516, -58.81642084023854267, -305.0891759886411023 ) ) ;
#17746 = CARTESIAN_POINT ( 'NONE',  ( 792.3570229623691148, -93.18005720387479585, 373.1304606946836770 ) ) ;
#17747 = ORIENTED_EDGE ( 'NONE', *, *, #21824, .T. ) ;
#17748 = CARTESIAN_POINT ( 'NONE',  ( 746.4236121716829757, -447.8272453906067199, -328.8385539511384650 ) ) ;
#17749 = ORIENTED_EDGE ( 'NONE', *, *, #7822, .T. ) ;
#17750 = CONTEXT_DEPENDENT_SHAPE_REPRESENTATION ( #12528, #24013 ) ;
#17751 = CARTESIAN_POINT ( 'NONE',  ( 756.3353852180819104, -29.90732993114771787, 331.1735550268788302 ) ) ;
#17752 = CARTESIAN_POINT ( 'NONE',  ( 804.9363028652555840, -304.2709662947832499, -338.2165204200192079 ) ) ;
#17754 = CARTESIAN_POINT ( 'NONE',  ( 813.9316612368132837, -271.4419599262321867, 348.6739635108323228 ) ) ;
#17753 = CARTESIAN_POINT ( 'NONE',  ( 792.2312462859673587, -371.9073299311465917, 307.2067596250082602 ) ) ;
#17755 = CARTESIAN_POINT ( 'NONE',  ( 803.8556311672234642, -57.62377810805111267, 365.6418435158340117 ) ) ;
#17756 = CARTESIAN_POINT ( 'NONE',  ( 793.0897708529556667, -246.5545181178799510, -361.3366627262616362 ) ) ;
#17757 = CARTESIAN_POINT ( 'NONE',  ( 767.8955696845333705, -240.4527844766015221, -362.1676090361162323 ) ) ;
#17758 = CARTESIAN_POINT ( 'NONE',  ( 803.6646147819162707, -449.9073299311464211, -348.8264449731211130 ) ) ;
#17759 = CARTESIAN_POINT ( 'NONE',  ( 771.1735550268778070, -105.1800572038747248, -316.3353852180827630 ) ) ;
#17760 = DIRECTION ( 'NONE',  ( -0.000000000000000000, 1.000000000000000000, -0.000000000000000000 ) ) ;
#17761 = CARTESIAN_POINT ( 'NONE',  ( 815.2698199232961542, -376.8164208402375834, 342.5225473063383106 ) ) ;
#17763 = DIRECTION ( 'NONE',  ( 1.000000000000000000, 0.000000000000000000, 0.000000000000000000 ) ) ;
#17762 = CARTESIAN_POINT ( 'NONE',  ( 759.9999999999992042, 205.0000000000000568, 319.9999999999999432 ) ) ;
#17764 = CARTESIAN_POINT ( 'NONE',  ( 745.5313806188320314, -63.28179084515324604, -333.7943932421247268 ) ) ;
#17765 = CARTESIAN_POINT ( 'NONE',  ( -37.63011601220122770, -501.1515549466498669, -368.0974687824633520 ) ) ;
#17766 = DIRECTION ( 'NONE',  ( 0.000000000000000000, 0.000000000000000000, 1.000000000000000000 ) ) ;
#17767 = CARTESIAN_POINT ( 'NONE',  ( 755.5913626894240451, -253.6454272087889876, 346.6156483768012890 ) ) ;
#17768 = CARTESIAN_POINT ( 'NONE',  ( 756.3353852180819104, -101.9073299311474727, 331.1735550268788302 ) ) ;
#17769 = EDGE_LOOP ( 'NONE', ( #17544, #13816, #15805, #36695 ) ) ;
#17770 = CARTESIAN_POINT ( 'NONE',  ( 799.2566176426618085, -0.009063572426172561425, -324.0069404352559559 ) ) ;
#17771 = CARTESIAN_POINT ( 'NONE',  ( 745.4481719005789273, -99.72551174932931417, -347.5162901302853697 ) ) ;
#17772 = CARTESIAN_POINT ( 'NONE',  ( 764.0069404352550464, -279.0783235625958127, 359.2566176426627180 ) ) ;
#17773 = CARTESIAN_POINT ( 'NONE',  ( 879.9999999999992042, 239.9999999999998295, -210.0000000000000000 ) ) ;
#17774 = CARTESIAN_POINT ( 'NONE',  ( 810.4231160770870019, -48.55451811788057626, 321.9338519418446936 ) ) ;
#17775 = CARTESIAN_POINT ( 'NONE',  ( 749.2812353651451076, -246.4527844766016074, -323.2262854647983090 ) ) ;
#17776 = CARTESIAN_POINT ( 'NONE',  ( 805.0032342141412300, -181.5436935675108145, 314.9967657858571783 ) ) ;
#17777 = CARTESIAN_POINT ( 'NONE',  ( 762.1405469898971887, -73.54369356751118403, 357.8594530101015607 ) ) ;
#17778 = DIRECTION ( 'NONE',  ( 1.892425610156518354E-16, 1.000000000000000000, -0.000000000000000000 ) ) ;
#17779 = CARTESIAN_POINT ( 'NONE',  ( 768.8385539511368734, -287.2601417444140566, -306.4236121716840557 ) ) ;
#17780 = CARTESIAN_POINT ( 'NONE',  ( 814.4686193811664907, -435.2817908451521021, 346.2056067578752732 ) ) ;
#17781 = CARTESIAN_POINT ( 'NONE',  ( 811.0346526505616112, -302.6346026584196238, -323.0537975583477532 ) ) ;
#17782 = DIRECTION ( 'NONE',  ( 1.000000000000000000, -0.000000000000000000, -0.000000000000000000 ) ) ;
#17783 = CARTESIAN_POINT ( 'NONE',  ( 804.9511171171677688, -365.8055962898682765, 335.8780910478229202 ) ) ;
#17784 = CARTESIAN_POINT ( 'NONE',  ( 745.0891759886404770, -52.27096629478401724, 342.4968714119734159 ) ) ;
#17785 = CARTESIAN_POINT ( 'NONE',  ( 792.1044303154645831, -396.4527844766010389, -317.8323909638837677 ) ) ;
#17786 = CARTESIAN_POINT ( 'NONE',  ( 793.2243759319678702, -50.53286901714203339, 318.4439275373583200 ) ) ;
#17787 = CARTESIAN_POINT ( 'NONE',  ( 764.8639956371174549, -200.0891481129653187, -319.7806653035542013 ) ) ;
#17788 = CARTESIAN_POINT ( 'NONE',  ( 815.0009284576459549, -102.3510508353236901, -338.7629533639073429 ) ) ;
#17789 = CARTESIAN_POINT ( 'NONE',  ( 771.2368401574024119, -205.4419599262324425, 374.2805881961240857 ) ) ;
#17790 = CARTESIAN_POINT ( 'NONE',  ( 771.2633955100217236, -23.90732993114773919, 363.4237431249939618 ) ) ;
#17791 = ORIENTED_EDGE ( 'NONE', *, *, #28721, .F. ) ;
#17792 = CARTESIAN_POINT ( 'NONE',  ( 772.3691319403857278, -215.2601417444141987, -315.8894580844506663 ) ) ;
#17793 = CARTESIAN_POINT ( 'NONE',  ( 797.6776695296629214, -211.5436935675107861, 357.6776695296636603 ) ) ;
#17794 = PRODUCT_DEFINITION_SHAPE ( 'NONE', 'NONE',  #45733 ) ;
#17795 = CARTESIAN_POINT ( 'NONE',  ( 788.7631598425961101, -49.44195992623295410, -305.7194118038759143 ) ) ;
#17796 = CARTESIAN_POINT ( 'NONE',  ( 781.8018195045267476, -334.2709662947830793, 365.1927285166407273 ) ) ;
#17797 = DIRECTION ( 'NONE',  ( 0.000000000000000000, 0.000000000000000000, 1.000000000000000000 ) ) ;
#17798 = ORIENTED_EDGE ( 'NONE', *, *, #35606, .F. ) ;
#17799 = CARTESIAN_POINT ( 'NONE',  ( 776.9566956441375396, -36.89650538077844288, 364.8461984189686405 ) ) ;
#17800 = CARTESIAN_POINT ( 'NONE',  ( 788.6739635108323228, -319.6454272087888739, -373.9316612368139090 ) ) ;
#17801 = CARTESIAN_POINT ( 'NONE',  ( 767.7687537140311633, -263.9073299311469327, 372.7932403749916830 ) ) ;
#17802 = CARTESIAN_POINT ( 'NONE',  ( 758.0141637701419768, -15.07832356259669560, 367.2620300519063790 ) ) ;
#17803 = CARTESIAN_POINT ( 'NONE',  ( 763.8424801807145741, -162.0090635724256742, -320.5453621957614700 ) ) ;
#17804 = CARTESIAN_POINT ( 'NONE',  ( 781.8018195045266339, -142.2709662947837330, -365.1927285166406705 ) ) ;
#17805 = CARTESIAN_POINT ( 'NONE',  ( 767.8955696845334842, -336.4527844766012663, -362.1676090361161755 ) ) ;
#17806 = ORIENTED_EDGE ( 'NONE', *, *, #4320, .T. ) ;
#17807 = CARTESIAN_POINT ( 'NONE',  ( 787.4397851343537695, -285.7255117493286889, 374.2001403089903988 ) ) ;
#17808 = LINE ( 'NONE', #42739, #12268 ) ;
#17809 = CARTESIAN_POINT ( 'NONE',  ( 804.8461984189677878, -218.1908817542437191, 336.9566956441385628 ) ) ;
#17810 = CARTESIAN_POINT ( 'NONE',  ( 764.0069404352550464, -327.0783235625956991, 359.2566176426627180 ) ) ;
#17811 = CARTESIAN_POINT ( 'NONE',  ( -78.83651009197140525, 260.0000000000000568, -191.9749999999935994 ) ) ;
#17812 = CARTESIAN_POINT ( 'NONE',  ( 773.4516893846965786, -163.6454272087893003, 315.8398074228977066 ) ) ;
#17813 = CARTESIAN_POINT ( 'NONE',  ( 804.4286716492782716, -17.36187538569322086, 345.3141322388244703 ) ) ;
#17814 = VERTEX_POINT ( 'NONE', #11116 ) ;
#17815 = CARTESIAN_POINT ( 'NONE',  ( 764.1737431748507561, -394.3726999360613377, -371.6461892240376415 ) ) ;
#17816 = CARTESIAN_POINT ( 'NONE',  ( 792.2312462859673587, 12.09267006885214180, -307.2067596250082602 ) ) ;
#17817 = CARTESIAN_POINT ( 'NONE',  ( 749.5768839229115201, -228.5545181178799794, 358.0661480581553064 ) ) ;
#17818 = CARTESIAN_POINT ( 'NONE',  ( 793.2243759319678702, -194.5328690171415644, 318.4439275373583200 ) ) ;
#17819 = CARTESIAN_POINT ( 'NONE',  ( 800.2193346964447755, -354.9982390220557704, -355.1360043628815788 ) ) ;
#17820 = CARTESIAN_POINT ( 'NONE',  ( 805.2837595273609850, -458.7363362996973706, 340.5290396650784714 ) ) ;
#17821 = FACE_OUTER_BOUND ( 'NONE', #26584, .T. ) ;
#17822 = CARTESIAN_POINT ( 'NONE',  ( 755.5913626894240451, -205.6454272087891297, -346.6156483768012890 ) ) ;
#17823 = CARTESIAN_POINT ( 'NONE',  ( 814.2001403089898304, -17.36187538569322086, 347.4397851343538264 ) ) ;
#17824 = CARTESIAN_POINT ( 'NONE',  ( 744.7301800767019131, -76.81642084023845030, 337.4774526936615757 ) ) ;
#17825 = CARTESIAN_POINT ( 'NONE',  ( -37.63011601220122770, -365.3551492539851893, -18.13243251470705886 ) ) ;
#17826 = CARTESIAN_POINT ( 'NONE',  ( 796.9462024416508257, -420.4527844766009821, -308.9653473494370246 ) ) ;
#17827 = DIRECTION ( 'NONE',  ( -0.000000000000000000, -0.000000000000000000, 1.000000000000000000 ) ) ;
#17828 = CARTESIAN_POINT ( 'NONE',  ( 807.2620300519052989, -360.0090635724250774, 318.0141637701419768 ) ) ;
#17829 = CARTESIAN_POINT ( 'NONE',  ( 801.6550554848130332, -456.5036469134198001, -360.7619500998734452 ) ) ;
#17830 = CARTESIAN_POINT ( 'NONE',  ( 792.3570229623688874, -333.1800572038740142, 373.1304606946836202 ) ) ;
#17831 = CARTESIAN_POINT ( 'NONE',  ( 747.2067596250078623, -51.18005720387493085, -352.2312462859687230 ) ) ;
#17832 = CARTESIAN_POINT ( 'NONE',  ( 788.7366044899766848, -275.9073299311469896, -316.5762568750059813 ) ) ;
#17833 = DIRECTION ( 'NONE',  ( -0.000000000000000000, 1.000000000000000000, -0.000000000000000000 ) ) ;
#17834 = CARTESIAN_POINT ( 'NONE',  ( 771.2633955100217236, -431.9073299311464211, 363.4237431249939618 ) ) ;
#17835 = COLOUR_RGB ( '',0.7921568627450980005, 0.8196078431372548767, 0.9333333333333333481 ) ;
#17836 = CARTESIAN_POINT ( 'NONE',  ( 800.9840315886518738, -196.9181544815164386, 354.1144889064786412 ) ) ;
#17837 = CARTESIAN_POINT ( 'NONE',  ( 814.2805881961230625, -73.64542720878957027, -331.2368401574024119 ) ) ;
#17838 = CARTESIAN_POINT ( 'NONE',  ( 805.0264073115434940, -78.35105083532376113, -339.4763451958999099 ) ) ;
#17839 = CARTESIAN_POINT ( 'NONE',  ( 813.2346286133761168, -101.2601417444146250, 328.9521613784389160 ) ) ;
#17840 = CARTESIAN_POINT ( 'NONE',  ( 804.6798772138710092, -399.7255117493283478, 334.6312213355106451 ) ) ;
#17841 = CARTESIAN_POINT ( 'NONE',  ( 786.2056067578752163, -155.8055962898689586, 374.4686193811670023 ) ) ;
#17842 = CARTESIAN_POINT ( 'NONE',  ( 804.4286716492782716, 6.638124614306706306, -345.3141322388244703 ) ) ;
#17843 = ORIENTED_EDGE ( 'NONE', *, *, #3514, .T. ) ;
#17844 = CARTESIAN_POINT ( 'NONE',  ( 803.6646147819161570, -113.9073299311474301, -348.8264449731210561 ) ) ;
#17845 = CARTESIAN_POINT ( 'NONE',  ( 802.7791456095903868, -388.7146871989592114, -329.0155153010375102 ) ) ;
#17846 = ADVANCED_FACE ( 'NONE', ( #39297 ), #32373, .T. ) ;
#17848 = CARTESIAN_POINT ( 'NONE',  ( 755.5713283507202505, -221.3618753856925707, 334.6858677611754729 ) ) ;
#17847 = CARTESIAN_POINT ( 'NONE',  ( 797.6776695296629214, -211.5436935675107861, 357.6776695296636603 ) ) ;
#17849 = CARTESIAN_POINT ( 'NONE',  ( 768.8385539511368734, -383.2601417444137155, -306.4236121716840557 ) ) ;
#17850 = DIRECTION ( 'NONE',  ( 0.000000000000000000, 0.000000000000000000, 1.000000000000000000 ) ) ;
#17851 = ORIENTED_EDGE ( 'NONE', *, *, #2980, .T. ) ;
#17852 = CARTESIAN_POINT ( 'NONE',  ( 804.4286716492782716, -425.3618753856919170, 345.3141322388244703 ) ) ;
#17853 = ORIENTED_EDGE ( 'NONE', *, *, #12031, .T. ) ;
#17854 =( NAMED_UNIT ( * ) PLANE_ANGLE_UNIT ( ) SI_UNIT ( $, .RADIAN. ) );
#17855 = CARTESIAN_POINT ( 'NONE',  ( 759.0252816721024374, -240.9982390220561683, -368.0189434323527280 ) ) ;
#17856 = CARTESIAN_POINT ( 'NONE',  ( 815.2698199232962679, -160.8164208402382371, 342.5225473063383674 ) ) ;
#17857 = CARTESIAN_POINT ( 'NONE',  ( 783.0745993439762742, -272.1908817542434917, 365.1016975059196739 ) ) ;
#17858 = ORIENTED_EDGE ( 'NONE', *, *, #34797, .F. ) ;
#17859 = CARTESIAN_POINT ( 'NONE',  ( 754.8072714833583632, -244.8164208402379245, -338.1981804954721156 ) ) ;
#17860 = VERTEX_POINT ( 'NONE', #8334 ) ;
#17861 = CARTESIAN_POINT ( 'NONE',  ( 781.7834795799800531, -370.8164208402375834, -315.0636971347436202 ) ) ;
#17862 = CARTESIAN_POINT ( 'NONE',  ( 804.4286716492782716, -17.36187538569322086, -345.3141322388244703 ) ) ;
#17863 = CARTESIAN_POINT ( 'NONE',  ( 779.4709603349208464, -216.3510508353233490, 314.7162404726379918 ) ) ;
#17864 = CARTESIAN_POINT ( 'NONE',  ( -786.4999999999993179, -513.1383975375929367, -369.9999999999999432 ) ) ;
#17865 = CARTESIAN_POINT ( 'NONE',  ( -468.8365100919714337, 260.0000000000001705, -199.9999999999908766 ) ) ;
#17866 = EDGE_CURVE ( 'NONE', #37975, #8835, #15501, .T. ) ;
#17867 = ORIENTED_EDGE ( 'NONE', *, *, #31416, .F. ) ;
#17868 = CARTESIAN_POINT ( 'NONE',  ( 788.7366044899766848, -11.90732993114778182, -316.5762568750059813 ) ) ;
#17869 = CARTESIAN_POINT ( 'NONE',  ( 799.9999999999993179, -512.9681489794448908, -339.9999999999999432 ) ) ;
#17870 = CARTESIAN_POINT ( 'NONE',  ( 829.9999999999992042, 290.0000000000001137, -320.0000000000000568 ) ) ;
#17871 = ORIENTED_EDGE ( 'NONE', *, *, #11703, .F. ) ;
#17872 = CARTESIAN_POINT ( 'NONE',  ( 750.9282345327678740, -256.9181544815163534, -319.8311093483690115 ) ) ;
#17873 = AXIS2_PLACEMENT_3D ( 'NONE', #45195, #31096, #27875 ) ;
#17874 = CARTESIAN_POINT ( 'NONE',  ( 773.7305795820266212, -153.2817908451529831, 374.8230680027170365 ) ) ;
#17876 = CARTESIAN_POINT ( 'NONE',  ( 800.2193346964447755, -258.9982390220561115, -355.1360043628815788 ) ) ;
#17875 = DIRECTION ( 'NONE',  ( 0.000000000000000000, 0.000000000000000000, -1.000000000000000000 ) ) ;
#17877 = CARTESIAN_POINT ( 'NONE',  ( 798.7617431975189675, -411.6237781080499758, -323.0428371773161871 ) ) ;
#17878 = DIRECTION ( 'NONE',  ( -1.000000000000000000, -0.000000000000000000, 0.000000000000000000 ) ) ;
#17879 = CARTESIAN_POINT ( 'NONE',  ( 798.5707757039680246, -125.4636090269712412, -356.7845633553585003 ) ) ;
#17880 = EDGE_CURVE ( 'NONE', #10740, #12298, #44361, .T. ) ;
#17881 = CARTESIAN_POINT ( 'NONE',  ( 521.6730038022808458, 199.9999999999999147, -122.7905160835442615 ) ) ;
#17882 = CARTESIAN_POINT ( 'NONE',  ( 746.0683387631852383, 4.558040073766884248, -331.3260364891676204 ) ) ;
#17883 = CARTESIAN_POINT ( 'NONE',  ( 751.9810565676468741, -314.0891481129650629, -360.9747183278973921 ) ) ;
#17884 = DIRECTION ( 'NONE',  ( 0.000000000000000000, 0.3826834323650836756, 0.9238795325112892920 ) ) ;
#17885 = CARTESIAN_POINT ( 'NONE',  ( 785.3141322388236176, -21.72551174932956641, 364.4286716492789537 ) ) ;
#17886 = CARTESIAN_POINT ( 'NONE',  ( 746.4236121716829757, -255.8272453906072315, 328.8385539511384650 ) ) ;
#17887 = CARTESIAN_POINT ( 'NONE',  ( 766.5853460496234675, -205.9874144716870035, -372.3518521366060554 ) ) ;
#17888 = CARTESIAN_POINT ( 'NONE',  ( 814.5518280994195948, -231.7255117493288310, 332.4837098697145734 ) ) ;
#17889 = CARTESIAN_POINT ( 'NONE',  ( 767.7687537140311633, -431.9073299311464211, -372.7932403749916830 ) ) ;
#17890 = CARTESIAN_POINT ( 'NONE',  ( -208.8365100919714052, 240.0000000000001137, -202.7499999999925251 ) ) ;
#17891 = CARTESIAN_POINT ( 'NONE',  ( 754.8072714833581358, -316.8164208402377540, 338.1981804954720587 ) ) ;
#17892 = VECTOR ( 'NONE', #39930, 1000.000000000000000 ) ;
#17893 = CARTESIAN_POINT ( 'NONE',  ( 793.0897708529556667, -102.5545181178804057, 361.3366627262616362 ) ) ;
#17894 = CARTESIAN_POINT ( 'NONE',  ( 766.9102291470427417, -66.55451811788050520, 318.6633372737382501 ) ) ;
#17895 = CARTESIAN_POINT ( 'NONE',  ( 787.6308680596127942, 12.73985825558503926, -364.1105419155492768 ) ) ;
#17896 = DIRECTION ( 'NONE',  ( 0.000000000000000000, 0.000000000000000000, 1.000000000000000000 ) ) ;
#17898 = EDGE_CURVE ( 'NONE', #15183, #29231, #22636, .T. ) ;
#17897 = DIRECTION ( 'NONE',  ( 1.000000000000000000, 0.000000000000000000, 0.000000000000000000 ) ) ;
#17900 = CARTESIAN_POINT ( 'NONE',  ( 756.3353852180819104, -365.9073299311465917, 331.1735550268788302 ) ) ;
#17899 = CARTESIAN_POINT ( 'NONE',  ( 780.5290396650775619, -108.3510508353236759, 365.2837595273619513 ) ) ;
#17901 = VERTEX_POINT ( 'NONE', #22398 ) ;
#17902 = CARTESIAN_POINT ( 'NONE',  ( 754.9735926884551418, -282.3510508353230080, -340.5236548041000333 ) ) ;
#17903 = CARTESIAN_POINT ( 'NONE',  ( 800.0135310231082713, -110.0891481129656597, 325.0180583372163028 ) ) ;
#17904 = CARTESIAN_POINT ( 'NONE',  ( 800.1688906516307043, -298.1692326535049347, -369.0717654672308186 ) ) ;
#17905 = DIRECTION ( 'NONE',  ( -1.000000000000000000, 0.000000000000000000, 0.000000000000000000 ) ) ;
#17906 = CARTESIAN_POINT ( 'NONE',  ( 744.9990715423526808, -426.3510508353226669, 341.2370466360926002 ) ) ;
#17907 = VERTEX_POINT ( 'NONE', #5305 ) ;
#17908 = CARTESIAN_POINT ( 'NONE',  ( 781.7834795799800531, -322.8164208402377540, 315.0636971347436202 ) ) ;
#17909 = CARTESIAN_POINT ( 'NONE',  ( 756.1348686366196716, -41.26014174441479554, -347.5531968255698416 ) ) ;
#17910 = CARTESIAN_POINT ( 'NONE',  ( 759.9864689768902508, -170.0891481129654608, -354.9819416627836404 ) ) ;
#17911 = CARTESIAN_POINT ( 'NONE',  ( 768.0187753319979720, -224.6346026584198228, -318.0580252608186242 ) ) ;
#17912 = CARTESIAN_POINT ( 'NONE',  ( 759.7806653035534055, -414.9982390220555430, 324.8639956371180801 ) ) ;
#17913 = CARTESIAN_POINT ( 'NONE',  ( 796.9462024416508257, -132.4527844766018916, -308.9653473494370246 ) ) ;
#17914 = ORIENTED_EDGE ( 'NONE', *, *, #27798, .T. ) ;
#17915 = CARTESIAN_POINT ( 'NONE',  ( 755.3201227861273992, -147.7255117493291721, -345.3687786644892981 ) ) ;
#17916 = ORIENTED_EDGE ( 'NONE', *, *, #11193, .F. ) ;
#17917 = CARTESIAN_POINT ( 'NONE',  ( 780.5236548040995785, -404.7363362996975980, -314.9735926884559944 ) ) ;
#17918 = EDGE_CURVE ( 'NONE', #10012, #35031, #2291, .T. ) ;
#17919 = CARTESIAN_POINT ( 'NONE',  ( 755.3028492785439312, -447.2817908451521021, 335.9200461376539693 ) ) ;
#17920 = CARTESIAN_POINT ( 'NONE',  ( 766.7756240680305382, -134.5328690171417350, 361.5560724626415663 ) ) ;
#17923 = CARTESIAN_POINT ( 'NONE',  ( 746.7653713866222915, -377.2601417444137724, 351.0478386215610271 ) ) ;
#17922 = CARTESIAN_POINT ( 'NONE',  ( 441.1634899080286232, 256.4999999999999432, -199.9999999999972431 ) ) ;
#17921 = DIRECTION ( 'NONE',  ( -0.000000000000000000, 1.000000000000000000, -0.000000000000000000 ) ) ;
#17924 = EDGE_CURVE ( 'NONE', #11158, #8116, #18795, .T. ) ;
#17925 = VERTEX_POINT ( 'NONE', #40651 ) ;
#17926 = CARTESIAN_POINT ( 'NONE',  ( 780.5236548040995785, -404.7363362996975980, -314.9735926884559944 ) ) ;
#17927 = DIRECTION ( 'NONE',  ( 1.000000000000000000, 0.000000000000000000, 0.000000000000000000 ) ) ;
#17928 = AXIS2_PLACEMENT_3D ( 'NONE', #35942, #36168, #4310 ) ;
#17929 = CARTESIAN_POINT ( 'NONE',  ( 764.1737431748507561, -178.3726999360619629, -371.6461892240376415 ) ) ;
#17930 = PRODUCT_DEFINITION_FORMATION_WITH_SPECIFIED_SOURCE ( 'ANY', '', #13724, .NOT_KNOWN. ) ;
#17931 = CARTESIAN_POINT ( 'NONE',  ( 804.1009440267234822, -47.46360902697148987, 314.0944755984392600 ) ) ;
#17933 = CARTESIAN_POINT ( 'NONE',  ( -208.8365100919714052, 260.0000000000001137, -208.0249999999927013 ) ) ;
#17932 = CARTESIAN_POINT ( 'NONE',  ( 181.1634899080285948, 260.0000000000000000, -199.9999999999953957 ) ) ;
#17934 = CARTESIAN_POINT ( 'NONE',  ( 766.7756240680305382, -302.5328690171411949, -361.5560724626415663 ) ) ;
#17935 = CARTESIAN_POINT ( 'NONE',  ( 701.1634899080286232, 258.0939999999999372, -199.9999999999990337 ) ) ;
#17936 = CARTESIAN_POINT ( 'NONE',  ( 813.5763878283155464, -171.8272453906074304, -351.1614460488615350 ) ) ;
#17937 = DIRECTION ( 'NONE',  ( 1.000000000000000000, 0.000000000000000000, 0.000000000000000000 ) ) ;
#17938 = CARTESIAN_POINT ( 'NONE',  ( 919.9999999999993179, 219.9999999999998863, -360.0000000000000000 ) ) ;
#17939 = EDGE_CURVE ( 'NONE', #16583, #5387, #23074, .T. ) ;
#17940 = CARTESIAN_POINT ( 'NONE',  ( 754.7162404726377645, -374.7363362996978253, 339.4709603349214717 ) ) ;
#17941 = CARTESIAN_POINT ( 'NONE',  ( 754.3581564841646241, -329.4636090269706870, 316.1443688327762516 ) ) ;
#17942 = CARTESIAN_POINT ( 'NONE',  ( 758.8095938919644823, -200.0891481129653471, -311.6929314249762797 ) ) ;
#17943 = FACE_OUTER_BOUND ( 'NONE', #38028, .T. ) ;
#17944 = CARTESIAN_POINT ( 'NONE',  ( 801.9419747391806368, 5.547215523397618142, -351.9812246680014027 ) ) ;
#17945 = CARTESIAN_POINT ( 'NONE',  ( 768.9521613784389729, -153.8272453906075157, 373.2346286133773106 ) ) ;
#17946 = CARTESIAN_POINT ( 'NONE',  ( 781.2497674668890113, -108.3510508353236759, -375.3608509340180603 ) ) ;
#17947 = CARTESIAN_POINT ( 'NONE',  ( 751.6929314249748586, -126.9982390220565094, 318.8095938919659034 ) ) ;
#17948 = CARTESIAN_POINT ( 'NONE',  ( 745.0891759886404770, -340.2709662947831362, -342.4968714119734159 ) ) ;
#17949 = DIRECTION ( 'NONE',  ( -1.000000000000000000, -0.000000000000000000, -0.000000000000000000 ) ) ;
#17950 = DIRECTION ( 'NONE',  ( -1.000000000000000000, -0.000000000000000000, -0.000000000000000000 ) ) ;
#17951 = CARTESIAN_POINT ( 'NONE',  ( 774.6858677611749044, -177.7255117493290868, 315.5713283507209894 ) ) ;
#17952 = CARTESIAN_POINT ( 'NONE',  ( 805.2837595273609850, -2.736336299698892027, 340.5290396650784714 ) ) ;
#17953 = EDGE_CURVE ( 'NONE', #28279, #10881, #25438, .T. ) ;
#17954 = CARTESIAN_POINT ( 'NONE',  ( 807.5423716828161105, -417.0783235625954148, -362.2119215644372048 ) ) ;
#17955 = CARTESIAN_POINT ( 'NONE',  ( 759.0252816721024374, -408.9982390220556567, -368.0189434323527280 ) ) ;
#17957 = EDGE_CURVE ( 'NONE', #15534, #44890, #34262, .T. ) ;
#17956 = CARTESIAN_POINT ( 'NONE',  ( 789.9999999999992042, 205.0000000000000568, -319.9999999999999432 ) ) ;
#17958 = CARTESIAN_POINT ( 'NONE',  ( 781.2497674668890113, -12.35105083532396897, 375.3608509340180603 ) ) ;
#17959 = ORIENTED_EDGE ( 'NONE', *, *, #21824, .F. ) ;
#17960 = VECTOR ( 'NONE', #26279, 1000.000000000000000 ) ;
#17961 = CARTESIAN_POINT ( 'NONE',  ( 748.3538107759620743, -184.7146871989598083, -355.8262568251490165 ) ) ;
#17962 = CARTESIAN_POINT ( 'NONE',  ( -809.9999999999993179, -512.9681489794448908, -350.0000000000000000 ) ) ;
#17963 = CARTESIAN_POINT ( 'NONE',  ( 761.9338519418445230, -326.5328690171411381, 370.4231160770881957 ) ) ;
#17964 = CARTESIAN_POINT ( 'NONE',  ( 801.9419747391806368, -138.4527844766019200, 351.9812246680014027 ) ) ;
#17965 = AXIS2_PLACEMENT_3D ( 'NONE', #1641, #5333, #27054 ) ;
#17966 = ORIENTED_EDGE ( 'NONE', *, *, #3591, .T. ) ;
#17967 = CARTESIAN_POINT ( 'NONE',  ( 764.8639956371174549, -320.0891481129648355, 319.7806653035542013 ) ) ;
#17968 = CARTESIAN_POINT ( 'NONE',  ( 777.5031285880264704, -46.81642084023858530, -374.9108240113588408 ) ) ;
#17969 = CARTESIAN_POINT ( 'NONE',  ( 745.4481719005789273, -99.72551174932931417, 347.5162901302853697 ) ) ;
#17970 = ORIENTED_EDGE ( 'NONE', *, *, #29198, .F. ) ;
#17971 = CARTESIAN_POINT ( 'NONE',  ( 778.7629533639073998, -440.7363362996975980, -375.0009284576466371 ) ) ;
#17972 = ORIENTED_EDGE ( 'NONE', *, *, #45351, .T. ) ;
#17973 = SHAPE_DEFINITION_REPRESENTATION ( #44674, #10941 ) ;
#17974 = AXIS2_PLACEMENT_3D ( 'NONE', #28585, #16077, #27162 ) ;
#17975 = EDGE_CURVE ( 'NONE', #36773, #41197, #3327, .T. ) ;
#17976 = CARTESIAN_POINT ( 'NONE',  ( 788.8264449731200330, -309.1800572038740711, -363.6646147819171233 ) ) ;
#17978 = CARTESIAN_POINT ( 'NONE',  ( 764.3348316497523456, -286.7146871989594388, 308.6759233522265617 ) ) ;
#17977 = CARTESIAN_POINT ( 'NONE',  ( 814.9108240113580450, -400.2709662947828519, 337.5031285880265273 ) ) ;
#17979 = EDGE_CURVE ( 'NONE', #7749, #24881, #40186, .T. ) ;
#17980 = CARTESIAN_POINT ( 'NONE',  ( 758.0141637701419768, -63.07832356259653750, 367.2620300519063790 ) ) ;
#17981 = CARTESIAN_POINT ( 'NONE',  ( 769.0155153010367712, -298.3726999360616787, -362.7791456095907279 ) ) ;
#17982 = CARTESIAN_POINT ( 'NONE',  ( 792.1044303154645831, -252.4527844766015789, -317.8323909638837677 ) ) ;
#17983 = CARTESIAN_POINT ( 'NONE',  ( 799.9999999999993179, -462.9681489794448339, 309.9999999999998863 ) ) ;
#17984 = CARTESIAN_POINT ( 'NONE',  ( 764.8639956371174549, -128.0891481129655176, -319.7806653035542013 ) ) ;
#17985 = CARTESIAN_POINT ( 'NONE',  ( 796.7737145352015204, -404.6346026584193396, 370.7187646348536987 ) ) ;
#17987 = CARTESIAN_POINT ( 'NONE',  ( 792.9530673105016376, -457.3789191291447196, 369.8291253130404357 ) ) ;
#17986 = LINE ( 'NONE', #1336, #20395 ) ;
#17988 = CARTESIAN_POINT ( 'NONE',  ( 773.7305795820266212, -81.28179084515319630, -374.8230680027170365 ) ) ;
#17989 = CARTESIAN_POINT ( 'NONE',  ( 989.9999999999992042, 56.78581973499402835, 212.6378164459127049 ) ) ;
#17991 = EDGE_CURVE ( 'NONE', #17401, #18157, #26163, .T. ) ;
#17990 = CARTESIAN_POINT ( 'NONE',  ( 784.9999999999992042, 205.0000000000000568, -255.0000000000000000 ) ) ;
#17992 = CARTESIAN_POINT ( 'NONE',  ( 802.5472867521000353, -268.3726999360616787, 350.8726784830461156 ) ) ;
#17993 = CARTESIAN_POINT ( 'NONE',  ( 781.8018195045266339, -142.2709662947837330, 365.1927285166406705 ) ) ;
#17994 = VERTEX_POINT ( 'NONE', #33722 ) ;
#17995 = CARTESIAN_POINT ( 'NONE',  ( 787.5531968255692163, -45.82724539060783542, -316.1348686366205811 ) ) ;
#17996 = VECTOR ( 'NONE', #30363, 1000.000000000000000 ) ;
#17997 = CIRCLE ( 'NONE', #35680, 6.119000000000013095 ) ;
#17998 = CARTESIAN_POINT ( 'NONE',  ( 801.1904061080338124, -116.0891481129656313, -368.3070685750236066 ) ) ;
#17999 = CARTESIAN_POINT ( 'NONE',  ( 805.0264073115434940, -342.3510508353228943, 339.4763451958999099 ) ) ;
#18000 = FACE_OUTER_BOUND ( 'NONE', #19138, .T. ) ;
#18001 = CARTESIAN_POINT ( 'NONE',  ( 813.5763878283155464, -51.82724539060782121, 351.1614460488615350 ) ) ;
#18002 = CARTESIAN_POINT ( 'NONE',  ( 746.8695393053150156, -245.9073299311469896, -327.6429770376306010 ) ) ;
#18003 = CARTESIAN_POINT ( 'NONE',  ( 782.5225473063381969, -214.2709662947834488, 375.2698199232970637 ) ) ;
#18004 = CARTESIAN_POINT ( 'NONE',  ( 785.3141322388236176, -69.72551174932942786, 364.4286716492789537 ) ) ;
#18005 =( NAMED_UNIT ( * ) SI_UNIT ( $, .STERADIAN. ) SOLID_ANGLE_UNIT ( ) );
#18006 = CARTESIAN_POINT ( 'NONE',  ( 812.6845335610512393, -295.9874144716866908, -353.5525998758768651 ) ) ;
#18007 = AXIS2_PLACEMENT_3D ( 'NONE', #18565, #39597, #4011 ) ;
#18008 = CARTESIAN_POINT ( 'NONE',  ( 791.0478386215596629, -453.8272453906066630, 306.7653713866226326 ) ) ;
#18009 = CARTESIAN_POINT ( 'NONE',  ( 782.5225473063381969, -310.2709662947832499, -375.2698199232970637 ) ) ;
#18010 = CARTESIAN_POINT ( 'NONE',  ( 939.9999999999993179, -600.0000000000001137, 360.0000000000000000 ) ) ;
#18011 = CARTESIAN_POINT ( 'NONE',  ( 787.6308680596127942, -371.2601417444136587, 364.1105419155492768 ) ) ;
#18012 = CARTESIAN_POINT ( 'NONE',  ( 787.5162901302840055, -59.36187538569307520, 305.4481719005793252 ) ) ;
#18013 = CARTESIAN_POINT ( 'NONE',  ( 778.2165204200184689, -382.8164208402374697, -364.9363028652563230 ) ) ;
#18014 = CARTESIAN_POINT ( 'NONE',  ( 765.8855110935204493, -70.16923265350563099, 319.0159684113471599 ) ) ;
#18015 = CARTESIAN_POINT ( 'NONE',  ( 804.9363028652555840, -208.2709662947835341, -338.2165204200192079 ) ) ;
#18016 = CARTESIAN_POINT ( 'NONE',  ( 788.7631598425961101, -97.44195992623281199, -305.7194118038759143 ) ) ;
#18017 = CARTESIAN_POINT ( 'NONE',  ( 814.8230680027162407, -221.8055962898687881, 333.7305795820267917 ) ) ;
#18018 = CARTESIAN_POINT ( 'NONE',  ( 774.6858677611749044, -33.72551174932952733, 315.5713283507209894 ) ) ;
#18019 = ORIENTED_EDGE ( 'NONE', *, *, #39979, .F. ) ;
#18020 = CARTESIAN_POINT ( 'NONE',  ( 764.0069404352550464, -207.0783235625960685, -359.2566176426627180 ) ) ;
#18021 = CARTESIAN_POINT ( 'NONE',  ( 771.2633955100217236, -215.9073299311471317, 363.4237431249939618 ) ) ;
#18022 = CARTESIAN_POINT ( 'NONE',  ( 748.3538107759620743, -16.71468719896031985, -355.8262568251490165 ) ) ;
#18023 = CARTESIAN_POINT ( 'NONE',  ( 795.1360043628808398, -332.0891481129649492, 360.2193346964456282 ) ) ;
#18024 = CARTESIAN_POINT ( 'NONE',  ( 802.7276637122909051, -452.9681489794449476, -352.0069550970126784 ) ) ;
#18025 = CARTESIAN_POINT ( 'NONE',  ( -858.8365100919713768, 258.0940000000002215, -206.1189999999881479 ) ) ;
#18026 = ORIENTED_EDGE ( 'NONE', *, *, #33961, .F. ) ;
#18027 = CARTESIAN_POINT ( 'NONE',  ( 765.8855110935204493, -46.16923265350568784, 319.0159684113471599 ) ) ;
#18028 = CARTESIAN_POINT ( 'NONE',  ( 812.3518521366052028, -337.0999726633342561, -326.5853460496235243 ) ) ;
#18029 = CARTESIAN_POINT ( 'NONE',  ( 800.9747183278959710, -300.9982390220559409, 311.9810565676471583 ) ) ;
#18030 = CARTESIAN_POINT ( 'NONE',  ( 795.6651683502461765, -10.71468719896033761, 371.3240766477733814 ) ) ;
#18031 = CARTESIAN_POINT ( 'NONE',  ( 758.4439275373578084, -180.5545181178801499, -353.2243759319684386 ) ) ;
#18032 = CARTESIAN_POINT ( 'NONE',  ( 804.6798772138708955, -135.7255117493291152, -334.6312213355107019 ) ) ;
#18033 = CARTESIAN_POINT ( 'NONE',  ( 803.4237431249931660, -351.1800572038740142, -331.2633955100225194 ) ) ;
#18034 = ORIENTED_EDGE ( 'NONE', *, *, #90, .F. ) ;
#18035 = CARTESIAN_POINT ( 'NONE',  ( 748.9653473494363425, -290.6346026584195101, 356.9462024416521331 ) ) ;
#18036 = VECTOR ( 'NONE', #3182, 1000.000000000000000 ) ;
#18037 = CARTESIAN_POINT ( 'NONE',  ( -26.63011601220122060, -563.3203001761230553, -342.3463313526983143 ) ) ;
#18038 = CARTESIAN_POINT ( 'NONE',  ( 776.9566956441375396, -348.8965053807774552, 364.8461984189686405 ) ) ;
#18039 = DIRECTION ( 'NONE',  ( 0.000000000000000000, 0.000000000000000000, 1.000000000000000000 ) ) ;
#18040 = VECTOR ( 'NONE', #4993, 1000.000000000000000 ) ;
#18041 = CARTESIAN_POINT ( 'NONE',  ( 804.6971507214547046, -171.2817908451529263, 344.0799538623459739 ) ) ;
#18042 = CARTESIAN_POINT ( 'NONE',  ( 755.5713283507202505, -29.36187538569318178, 334.6858677611754729 ) ) ;
#18043 = ORIENTED_EDGE ( 'NONE', *, *, #20725, .F. ) ;
#18044 = CARTESIAN_POINT ( 'NONE',  ( 768.9521613784389729, -369.8272453906068904, -373.2346286133773106 ) ) ;
#18045 = CARTESIAN_POINT ( 'NONE',  ( 792.3570229623691148, 2.819942796124898621, -373.1304606946836770 ) ) ;
#18046 = CARTESIAN_POINT ( 'NONE',  ( 814.8207195650702488, -266.1908817542435486, 336.2433038121456548 ) ) ;
#18047 = CARTESIAN_POINT ( 'NONE',  ( 805.0264073115434940, -198.3510508353234059, 339.4763451958999099 ) ) ;
#18048 = CARTESIAN_POINT ( 'NONE',  ( 755.3201227861273992, -363.7255117493284047, -345.3687786644892981 ) ) ;
#18049 = CARTESIAN_POINT ( 'NONE',  ( 781.8018195045266339, 1.729033705215812011, 365.1927285166406705 ) ) ;
#18050 = DIRECTION ( 'NONE',  ( 0.000000000000000000, 1.000000000000000000, 0.000000000000000000 ) ) ;
#18051 = CARTESIAN_POINT ( 'NONE',  ( 804.4086373105744769, -217.6454272087891582, -333.3843516231986541 ) ) ;
#18052 = CARTESIAN_POINT ( 'NONE',  ( 758.8095938919642549, -8.089148112965974136, 311.6929314249763365 ) ) ;
#18053 = CARTESIAN_POINT ( 'NONE',  ( 814.9108240113580450, -88.27096629478390355, 337.5031285880265273 ) ) ;
#18054 = DIRECTION ( 'NONE',  ( 0.000000000000000000, 0.000000000000000000, 1.000000000000000000 ) ) ;
#18055 = CARTESIAN_POINT ( 'NONE',  ( 777.5031285880264704, -406.8164208402375266, -374.9108240113588408 ) ) ;
#18056 = AXIS2_PLACEMENT_3D ( 'NONE', #36285, #4871, #18739 ) ;
#18057 = CARTESIAN_POINT ( 'NONE',  ( 784.4999999999993179, -110.5936016518799221, 750.6326042729449455 ) ) ;
#18058 = AXIS2_PLACEMENT_3D ( 'NONE', #5147, #40275, #26160 ) ;
#18059 = CARTESIAN_POINT ( 'NONE',  ( 809.0717654672305343, -364.9181544815158986, 360.1688906516309885 ) ) ;
#18060 = CARTESIAN_POINT ( 'NONE',  ( -200.7583438952258348, 239.9999999999992326, -244.9999999999999716 ) ) ;
#18061 = CARTESIAN_POINT ( 'NONE',  ( 814.2001403089898304, -329.3618753856922581, 347.4397851343538264 ) ) ;
#18062 = CARTESIAN_POINT ( 'NONE',  ( 796.7737145352015204, -68.63460265842033436, -370.7187646348536987 ) ) ;
#18063 = CARTESIAN_POINT ( 'NONE',  ( 754.8072714833581358, -292.8164208402376971, -338.1981804954720587 ) ) ;
#18064 = CARTESIAN_POINT ( 'NONE',  ( -208.8365100919714052, 256.5000000000001137, -199.9999999999926956 ) ) ;
#18065 = CARTESIAN_POINT ( 'NONE',  ( 759.7806653035534055, -438.9982390220553157, 324.8639956371180801 ) ) ;
#18066 = CARTESIAN_POINT ( 'NONE',  ( 760.7433823573367135, -204.0090635724255606, 355.9930595647440441 ) ) ;
#18067 = CARTESIAN_POINT ( 'NONE',  ( 791.0478386215596629, -69.82724539060775726, -306.7653713866226326 ) ) ;
#18068 = CARTESIAN_POINT ( 'NONE',  ( 773.3843516231979720, -85.44195992623282621, -364.4086373105754433 ) ) ;
#18069 = CARTESIAN_POINT ( 'NONE',  ( 764.3348316497523456, -94.71468719896007826, 308.6759233522265617 ) ) ;
#18070 = CARTESIAN_POINT ( 'NONE',  ( 805.1927285166399315, -400.8164208402374697, 341.8018195045277707 ) ) ;
#18071 = VECTOR ( 'NONE', #18638, 1000.000000000000000 ) ;
#18072 = CARTESIAN_POINT ( 'NONE',  ( 803.6646147819161570, -449.9073299311463643, 348.8264449731210561 ) ) ;
#18073 = VERTEX_POINT ( 'NONE', #18966 ) ;
#18074 = CARTESIAN_POINT ( 'NONE',  ( 802.1676090361156639, -86.63460265842023489, -327.8955696845344505 ) ) ;
#18075 = AXIS2_PLACEMENT_3D ( 'NONE', #11649, #15344, #11864 ) ;
#18076 = CONICAL_SURFACE ( 'NONE', #45377, 8.025000000000003908, 0.7853981633974446153 ) ;
#18077 = CARTESIAN_POINT ( 'NONE',  ( 794.1144889064781864, -394.1692326535045368, -360.9840315886528401 ) ) ;
#18079 = CARTESIAN_POINT ( 'NONE',  ( 795.1360043628808398, -236.0891481129652334, 360.2193346964456282 ) ) ;
#18078 = CARTESIAN_POINT ( 'NONE',  ( 771.2633955100217236, -215.9073299311471317, 363.4237431249939618 ) ) ;
#18080 = CARTESIAN_POINT ( 'NONE',  ( 745.1769319972822814, -401.8055962898681059, -346.2694204179732083 ) ) ;
#18081 = CARTESIAN_POINT ( 'NONE',  ( 779.9999999999992042, -452.9681489794448339, -370.0000000000000568 ) ) ;
#18082 = EDGE_LOOP ( 'NONE', ( #19481, #31200, #17165, #5259 ) ) ;
#18083 = CARTESIAN_POINT ( 'NONE',  ( 801.9419747391806368, -426.4527844766010389, 351.9812246680014027 ) ) ;
#18084 = ORIENTED_EDGE ( 'NONE', *, *, #31160, .F. ) ;
#18085 =( NAMED_UNIT ( * ) PLANE_ANGLE_UNIT ( ) SI_UNIT ( $, .RADIAN. ) );
#18086 = CARTESIAN_POINT ( 'NONE',  ( 745.4481719005789273, -243.7255117493287742, -347.5162901302853129 ) ) ;
#18087 = CARTESIAN_POINT ( 'NONE',  ( 763.0537975583476964, -168.4527844766018347, 371.0346526505628617 ) ) ;
#18088 = AXIS2_PLACEMENT_3D ( 'NONE', #25436, #509, #4216 ) ;
#18089 = CARTESIAN_POINT ( 'NONE',  ( 769.0155153010367712, -250.3726999360618208, 362.7791456095907279 ) ) ;
#18090 = VERTEX_POINT ( 'NONE', #29798 ) ;
#18091 = CARTESIAN_POINT ( 'NONE',  ( 775.8780910478218402, -57.28179084515326736, -364.9511171171680530 ) ) ;
#18093 = ADVANCED_FACE ( 'NONE', ( #12255 ), #32101, .F. ) ;
#18092 = CARTESIAN_POINT ( 'NONE',  ( 803.6646147819162707, -257.9073299311469327, -348.8264449731211130 ) ) ;
#18094 = AXIS2_PLACEMENT_3D ( 'NONE', #27933, #6685, #30948 ) ;
#18095 = ORIENTED_EDGE ( 'NONE', *, *, #9669, .T. ) ;
#18096 = CARTESIAN_POINT ( 'NONE',  ( 764.8639956371174549, -344.0891481129647786, -319.7806653035542013 ) ) ;
#18097 = CARTESIAN_POINT ( 'NONE',  ( 756.3353852180819104, -5.907329931147798696, -331.1735550268788302 ) ) ;
#18098 = AXIS2_PLACEMENT_3D ( 'NONE', #19406, #36508, #8577 ) ;
#18099 = CARTESIAN_POINT ( 'NONE',  ( 756.7813123517142913, -235.9874144716868898, 329.9779781133712504 ) ) ;
#18100 = FACE_OUTER_BOUND ( 'NONE', #27791, .T. ) ;
#18101 = PLANE ( 'NONE',  #8644 ) ;
#18102 = ORIENTED_EDGE ( 'NONE', *, *, #25259, .T. ) ;
#18103 = CARTESIAN_POINT ( 'NONE',  ( 781.7834795799800531, -34.81642084023861372, -315.0636971347436202 ) ) ;
#18104 = DIRECTION ( 'NONE',  ( 0.000000000000000000, 0.000000000000000000, 1.000000000000000000 ) ) ;
#18105 = DIRECTION ( 'NONE',  ( 0.000000000000000000, 0.000000000000000000, 1.000000000000000000 ) ) ;
#18106 = ORIENTED_EDGE ( 'NONE', *, *, #6607, .F. ) ;
#18107 = CARTESIAN_POINT ( 'NONE',  ( 749.5768839229115201, -276.5545181178798657, -358.0661480581553064 ) ) ;
#18108 = CIRCLE ( 'NONE', #7018, 6.118999999999985562 ) ;
#18109 = CARTESIAN_POINT ( 'NONE',  ( 744.6391490659812007, -182.7363362996983369, 338.7502325331110455 ) ) ;
#18110 = VECTOR ( 'NONE', #40102, 1000.000000000000000 ) ;
#18112 = CARTESIAN_POINT ( 'NONE',  ( 803.4237431249931660, -255.1800572038742700, -331.2633955100225194 ) ) ;
#18111 = DIRECTION ( 'NONE',  ( 1.000000000000000000, 0.000000000000000000, -0.000000000000000000 ) ) ;
#18113 = CARTESIAN_POINT ( 'NONE',  ( -829.9999999999994316, 579.9999999999998863, -360.0000000000000000 ) ) ;
#18114 = CARTESIAN_POINT ( 'NONE',  ( 798.5707757039680246, -101.4636090269713264, -356.7845633553585003 ) ) ;
#18115 = AXIS2_PLACEMENT_3D ( 'NONE', #4033, #7505, #11192 ) ;
#18116 = EDGE_CURVE ( 'NONE', #29342, #42674, #5549, .T. ) ;
#18117 = CARTESIAN_POINT ( 'NONE',  ( -786.4999999999993179, -512.9681489794448908, -352.0000000000000000 ) ) ;
#18118 = CARTESIAN_POINT ( 'NONE',  ( 801.9858362298568863, 20.92167643740319605, -312.7379699480935642 ) ) ;
#18119 = CARTESIAN_POINT ( 'NONE',  ( 772.4837098697145166, -311.3618753856923149, -374.5518280994205611 ) ) ;
#18120 = FACE_OUTER_BOUND ( 'NONE', #39811, .T. ) ;
#18121 = CARTESIAN_POINT ( 'NONE',  ( 771.2633955100217236, -23.90732993114773919, 363.4237431249939618 ) ) ;
#18122 = CARTESIAN_POINT ( 'NONE',  ( 748.6759233522253680, -256.3726999360617924, 324.3348316497537098 ) ) ;
#18123 = CARTESIAN_POINT ( 'NONE',  ( 746.7653713866222915, -209.2601417444142839, -351.0478386215610271 ) ) ;
#18124 = CARTESIAN_POINT ( 'NONE',  ( 796.7737145352015204, -236.6346026584198228, 370.7187646348536987 ) ) ;
#18125 = CARTESIAN_POINT ( 'NONE',  ( 812.7932403749906598, -447.1800572038736732, -327.7687537140311633 ) ) ;
#18126 = DIRECTION ( 'NONE',  ( 1.000000000000000000, 0.000000000000000000, 0.000000000000000000 ) ) ;
#18127 = CARTESIAN_POINT ( 'NONE',  ( 800.0135310231082713, -326.0891481129649492, 325.0180583372163028 ) ) ;
#18128 = CIRCLE ( 'NONE', #6304, 2.749999999999919176 ) ;
#18129 = CARTESIAN_POINT ( 'NONE',  ( 779.4763451958990572, -104.7363362996985785, 365.0264073115438919 ) ) ;
#18130 = CARTESIAN_POINT ( 'NONE',  ( 799.2566176426618085, -72.00906357242594424, 324.0069404352559559 ) ) ;
#18131 = CARTESIAN_POINT ( 'NONE',  ( 804.9511171171677688, 18.19440371013048008, -335.8780910478229202 ) ) ;
#18132 = AXIS2_PLACEMENT_3D ( 'NONE', #17475, #24596, #41728 ) ;
#18133 = CARTESIAN_POINT ( 'NONE',  ( 879.9999999999992042, 99.99999999999984368, -350.0000000000000000 ) ) ;
#18134 = CARTESIAN_POINT ( 'NONE',  ( 767.9999999999992042, 205.0000000000000568, -329.9999999999999432 ) ) ;
#18136 = CARTESIAN_POINT ( 'NONE',  ( 801.9419747391806368, -354.4527844766012095, 351.9812246680014027 ) ) ;
#18135 = CARTESIAN_POINT ( 'NONE',  ( 783.0433043558608688, -144.8965053807781089, 315.1538015810313027 ) ) ;
#18137 = EDGE_LOOP ( 'NONE', ( #8977, #36899 ) ) ;
#18138 = CARTESIAN_POINT ( 'NONE',  ( 770.0799878456142551, -277.9874144716867477, -362.9823548866085616 ) ) ;
#18139 = CARTESIAN_POINT ( 'NONE',  ( 755.0636971347428243, -124.2709662947837899, 341.7834795799807353 ) ) ;
#18140 = CARTESIAN_POINT ( 'NONE',  ( 754.0944755984390895, -279.6237781080503737, -364.1009440267246760 ) ) ;
#18141 = CARTESIAN_POINT ( 'NONE',  ( 939.9999999999992042, 74.99999999999984368, 350.0000000000000000 ) ) ;
#18142 = CARTESIAN_POINT ( 'NONE',  ( 746.7653713866222915, -401.2601417444137155, 351.0478386215610271 ) ) ;
#18143 = EDGE_CURVE ( 'NONE', #28937, #35282, #30245, .T. ) ;
#18144 = ORIENTED_EDGE ( 'NONE', *, *, #32011, .F. ) ;
#18145 = CARTESIAN_POINT ( 'NONE',  ( 764.8639956371174549, -320.0891481129648355, 319.7806653035542013 ) ) ;
#18146 = AXIS2_PLACEMENT_3D ( 'NONE', #3061, #10218, #31236 ) ;
#18147 = CARTESIAN_POINT ( 'NONE',  ( 755.5713283507202505, -173.3618753856927128, -334.6858677611754729 ) ) ;
#18148 = CARTESIAN_POINT ( 'NONE',  ( 788.8264449731200330, -213.1800572038743553, -363.6646147819171233 ) ) ;
#18149 = CARTESIAN_POINT ( 'NONE',  ( 795.1360043628807261, -452.0891481129646650, 360.2193346964456282 ) ) ;
#18150 = ADVANCED_FACE ( 'NONE', ( #19401, #36952 ), #26772, .F. ) ;
#18151 = VECTOR ( 'NONE', #6828, 1000.000000000000114 ) ;
#18152 = CARTESIAN_POINT ( 'NONE',  ( 747.2067596250078623, -147.1800572038746395, -352.2312462859687230 ) ) ;
#18153 = APPLICATION_CONTEXT ( 'automotive_design' ) ;
#18154 = VERTEX_POINT ( 'NONE', #1833 ) ;
#18155 = CIRCLE ( 'NONE', #29189, 10.00000000000000888 ) ;
#18156 = CARTESIAN_POINT ( 'NONE',  ( 768.0187753319979720, -152.6346026584200786, -318.0580252608186242 ) ) ;
#18157 = VERTEX_POINT ( 'NONE', #30025 ) ;
#18158 = CARTESIAN_POINT ( 'NONE',  ( 757.4527132478984868, -376.3726999360614514, -329.1273215169538844 ) ) ;
#18159 = CARTESIAN_POINT ( 'NONE',  ( 781.7834795799800531, 13.18357915976123174, 315.0636971347436202 ) ) ;
#18160 = CARTESIAN_POINT ( 'NONE',  ( 745.4481719005789273, -219.7255117493289447, 347.5162901302853129 ) ) ;
#18161 = CARTESIAN_POINT ( 'NONE',  ( 769.1273215169530886, -118.7146871989600072, 317.4527132478988847 ) ) ;
#18164 = CARTESIAN_POINT ( 'NONE',  ( 754.0944755984390895, -399.6237781080500326, 364.1009440267246760 ) ) ;
#18163 = LINE ( 'NONE', #11447, #15903 ) ;
#18162 = DIRECTION ( 'NONE',  ( 0.000000000000000000, 0.000000000000000000, -1.000000000000000000 ) ) ;
#18165 = ORIENTED_EDGE ( 'NONE', *, *, #14254, .F. ) ;
#18166 = CARTESIAN_POINT ( 'NONE',  ( 793.0897708529556667, -390.5545181178794678, -361.3366627262616362 ) ) ;
#18167 = DIRECTION ( 'NONE',  ( 1.000000000000000000, 0.000000000000000000, 0.000000000000000000 ) ) ;
#18168 = CARTESIAN_POINT ( 'NONE',  ( 744.6391490659812007, -158.7363362996984222, -338.7502325331110455 ) ) ;
#18169 = CARTESIAN_POINT ( 'NONE',  ( 771.3260364891663130, -43.64542720878966975, 306.0683387631859773 ) ) ;
#18170 = VECTOR ( 'NONE', #40072, 1000.000000000000000 ) ;
#18172 = CARTESIAN_POINT ( 'NONE',  ( 989.9999999999992042, 240.0000000000000568, 210.0000000000000000 ) ) ;
#18171 = LINE ( 'NONE', #8216, #12336 ) ;
#18173 = CARTESIAN_POINT ( 'NONE',  ( 795.9930595647434757, -315.0783235625957559, -320.7433823573372820 ) ) ;
#18174 = CARTESIAN_POINT ( 'NONE',  ( 794.9819416627830151, -444.9982390220554862, -319.9864689768909898 ) ) ;
#18176 = VECTOR ( 'NONE', #29190, 1000.000000000000000 ) ;
#18175 = CARTESIAN_POINT ( 'NONE',  ( 797.8822607201568644, -174.5545181178801784, -370.1134526219340160 ) ) ;
#18177 = CARTESIAN_POINT ( 'NONE',  ( -784.4999999999993179, -512.9681489794448908, -339.9999999999999432 ) ) ;
#18178 = CARTESIAN_POINT ( 'NONE',  ( -338.8365100919713200, 260.0000000000001137, -208.0249999999917918 ) ) ;
#18179 = CARTESIAN_POINT ( 'NONE',  ( 755.5913626894240451, -373.6454272087887034, 346.6156483768012890 ) ) ;
#18180 = CARTESIAN_POINT ( 'NONE',  ( 793.5525998758768083, -343.0999726633342561, 372.6845335610516941 ) ) ;
#18181 = CARTESIAN_POINT ( 'NONE',  ( 777.5031285880264704, -190.8164208402381234, -374.9108240113588408 ) ) ;
#18182 = CARTESIAN_POINT ( 'NONE',  ( 759.9999999999992042, -462.9681489794448339, 309.9999999999998863 ) ) ;
#18183 = CARTESIAN_POINT ( 'NONE',  ( 771.2633955100217236, 0.09267006885218045942, -363.4237431249939618 ) ) ;
#18184 = CIRCLE ( 'NONE', #6361, 7.999999999999896083 ) ;
#18185 = CARTESIAN_POINT ( 'NONE',  ( 752.7379699480933368, -132.0090635724257595, 361.9858362298580232 ) ) ;
#18186 = CARTESIAN_POINT ( 'NONE',  ( 754.0944755984390895, -87.62377810805102740, -364.1009440267246760 ) ) ;
#18187 = CARTESIAN_POINT ( 'NONE',  ( 787.5162901302840055, -107.3618753856928976, 305.4481719005792684 ) ) ;
#18188 = CARTESIAN_POINT ( 'NONE',  ( 763.2262854647970016, -344.6346026584195101, -309.2812353651462445 ) ) ;
#18189 = CIRCLE ( 'NONE', #35875, 2.749999999999891642 ) ;
#18190 = DIRECTION ( 'NONE',  ( -0.000000000000000000, 1.000000000000000000, -0.000000000000000000 ) ) ;
#18191 = LINE ( 'NONE', #18413, #16848 ) ;
#18192 = CARTESIAN_POINT ( 'NONE',  ( 756.5762568750052424, -219.1800572038744122, 348.7366044899774238 ) ) ;
#18193 = CARTESIAN_POINT ( 'NONE',  ( 755.8990559732751535, -443.4636090269702322, 365.9055244015606831 ) ) ;
#18194 = CARTESIAN_POINT ( 'NONE',  ( 783.7566961878529810, -408.8965053807772847, -305.1792804349288417 ) ) ;
#18195 = CARTESIAN_POINT ( 'NONE',  ( 759.0252816721024374, -432.9982390220555999, -368.0189434323527280 ) ) ;
#18196 = DIRECTION ( 'NONE',  ( -0.000000000000000000, -0.000000000000000000, 1.000000000000000000 ) ) ;
#18197 = CARTESIAN_POINT ( 'NONE',  ( 754.0944755984390895, 8.376221891948691933, 364.1009440267246760 ) ) ;
#18198 = ORIENTED_EDGE ( 'NONE', *, *, #15402, .T. ) ;
#18199 = EDGE_CURVE ( 'NONE', #39971, #11672, #44110, .T. ) ;
#18200 = CARTESIAN_POINT ( 'NONE',  ( 804.4286716492782716, -17.36187538569322086, 345.3141322388244703 ) ) ;
#18201 = CARTESIAN_POINT ( 'NONE',  ( 800.1688906516307043, -202.1692326535051905, -369.0717654672308186 ) ) ;
#18202 = DIRECTION ( 'NONE',  ( 1.000000000000000000, 0.000000000000000000, 0.000000000000000000 ) ) ;
#18203 = CARTESIAN_POINT ( 'NONE',  ( 766.5853460496234675, -301.9874144716867477, 372.3518521366060554 ) ) ;
#18204 = CARTESIAN_POINT ( 'NONE',  ( 756.5762568750052424, -171.1800572038745543, 348.7366044899774238 ) ) ;
#18205 = VERTEX_POINT ( 'NONE', #40878 ) ;
#18206 = CARTESIAN_POINT ( 'NONE',  ( 762.1405469898971887, -289.5436935675103882, 357.8594530101015607 ) ) ;
#18207 = AXIS2_PLACEMENT_3D ( 'NONE', #33257, #10949, #15700 ) ;
#18208 = EDGE_CURVE ( 'NONE', #24210, #17589, #4808, .T. ) ;
#18209 = CARTESIAN_POINT ( 'NONE',  ( 800.9747183278959710, -36.99823902205679360, -311.9810565676471583 ) ) ;
#18210 = AXIS2_PLACEMENT_3D ( 'NONE', #26711, #30648, #40383 ) ;
#18211 = CARTESIAN_POINT ( 'NONE',  ( 811.0346526505617248, -86.63460265842024910, 323.0537975583478101 ) ) ;
#18212 = ORIENTED_EDGE ( 'NONE', *, *, #36226, .T. ) ;
#18213 = CARTESIAN_POINT ( 'NONE',  ( 766.4474001241216001, -451.0999726633339151, -307.3154664389482491 ) ) ;
#18214 = ORIENTED_EDGE ( 'NONE', *, *, #3549, .T. ) ;
#18215 = PRODUCT_CONTEXT ( 'NONE', #4845, 'mechanical' ) ;
#18217 = CARTESIAN_POINT ( 'NONE',  ( 793.9708237608222134, -334.9181544815160692, 319.2295555964448681 ) ) ;
#18216 = CARTESIAN_POINT ( 'NONE',  ( 801.9419747391806368, -66.45278447660216159, 351.9812246680014027 ) ) ;
#18218 = VECTOR ( 'NONE', #19335, 1000.000000000000000 ) ;
#18220 = CARTESIAN_POINT ( 'NONE',  ( 773.7943932421234194, -287.8055962898685038, 305.5313806188329409 ) ) ;
#18219 = CARTESIAN_POINT ( 'NONE',  ( 787.5162901302840055, -395.3618753856919739, 305.4481719005793252 ) ) ;
#18221 = CARTESIAN_POINT ( 'NONE',  ( 807.5423716828161105, -81.07832356259649487, 362.2119215644372048 ) ) ;
#18222 = CARTESIAN_POINT ( 'NONE',  ( 802.5472867521000353, -292.3726999360616219, -350.8726784830461156 ) ) ;
#18223 = CARTESIAN_POINT ( 'NONE',  ( 781.8018195045266339, -286.2709662947833635, -365.1927285166406705 ) ) ;
#18224 = FACE_OUTER_BOUND ( 'NONE', #23678, .T. ) ;
#18225 = CARTESIAN_POINT ( 'NONE',  ( 802.1676090361156639, -134.6346026584201070, -327.8955696845344505 ) ) ;
#18226 = EDGE_CURVE ( 'NONE', #36701, #22122, #12931, .T. ) ;
#18227 = FACE_BOUND ( 'NONE', #8107, .T. ) ;
#18228 = CARTESIAN_POINT ( 'NONE',  ( 777.5031285880264704, -382.8164208402374697, 374.9108240113588408 ) ) ;
#18230 = PLANE ( 'NONE',  #3458 ) ;
#18229 = CARTESIAN_POINT ( 'NONE',  ( -454.7528517110260964, 200.0000000000001137, -122.7905160835438068 ) ) ;
#18231 = ADVANCED_FACE ( 'NONE', ( #4086 ), #27248, .F. ) ;
#18232 = CARTESIAN_POINT ( 'NONE',  ( 778.7629533639073998, -80.73633629969864955, -375.0009284576466371 ) ) ;
#18233 = CARTESIAN_POINT ( 'NONE',  ( 701.1634899080286232, 259.9999999999999432, -202.7499999999988916 ) ) ;
#18234 = LINE ( 'NONE', #39241, #29744 ) ;
#18235 = CARTESIAN_POINT ( 'NONE',  ( 804.4086373105744769, -265.6454272087889876, 333.3843516231986541 ) ) ;
#18236 = CARTESIAN_POINT ( 'NONE',  ( 791.9812246680005501, -140.6346026584201070, 361.9419747391813189 ) ) ;
#18237 = EDGE_CURVE ( 'NONE', #45366, #8774, #8510, .T. ) ;
#18238 = ORIENTED_EDGE ( 'NONE', *, *, #34495, .F. ) ;
#18239 = CARTESIAN_POINT ( 'NONE',  ( 796.1575198192839480, -54.00906357242601530, -359.4546378042384163 ) ) ;
#18240 = CARTESIAN_POINT ( 'NONE',  ( 763.0537975583476964, -120.4527844766019768, -371.0346526505628617 ) ) ;
#18241 = CARTESIAN_POINT ( 'NONE',  ( 803.2186876482843445, -343.9874144716865771, 350.0220218866286928 ) ) ;
#18242 = VECTOR ( 'NONE', #3452, 1000.000000000000000 ) ;
#18243 = CARTESIAN_POINT ( 'NONE',  ( 989.9999999999992042, -426.1357934546398383, -350.0000000000000000 ) ) ;
#18244 = CARTESIAN_POINT ( 'NONE',  ( 793.5525998758768083, -55.09997266333508747, 372.6845335610516941 ) ) ;
#18246 = VECTOR ( 'NONE', #27921, 1000.000000000000000 ) ;
#18245 = CARTESIAN_POINT ( 'NONE',  ( 744.7301800767019131, -220.8164208402379529, -337.4774526936615757 ) ) ;
#18247 = CARTESIAN_POINT ( 'NONE',  ( 797.6776695296629214, -115.5436935675110988, 357.6776695296636603 ) ) ;
#18248 = DIRECTION ( 'NONE',  ( -0.000000000000000000, 1.000000000000000000, -0.000000000000000000 ) ) ;
#18249 = CARTESIAN_POINT ( 'NONE',  ( 803.8556311672234642, -321.6237781080502600, -365.6418435158340117 ) ) ;
#18250 = AXIS2_PLACEMENT_3D ( 'NONE', #15539, #8616, #30073 ) ;
#18251 = ADVANCED_FACE ( 'NONE', ( #10540 ), #24616, .F. ) ;
#18252 = CARTESIAN_POINT ( 'NONE',  ( 811.3240766477731540, -460.3726999360611103, 355.6651683502462902 ) ) ;
#18253 = CARTESIAN_POINT ( 'NONE',  ( 805.0032342141412300, -301.5436935675105588, -314.9967657858571783 ) ) ;
#18254 = DIRECTION ( 'NONE',  ( 0.000000000000000000, 0.000000000000000000, 1.000000000000000000 ) ) ;
#18255 = CARTESIAN_POINT ( 'NONE',  ( 755.8398074228967971, -379.4419599262318457, 333.4516893846970333 ) ) ;
#18256 = CARTESIAN_POINT ( 'NONE',  ( 796.9462024416508257, -36.45278447660224685, 308.9653473494370246 ) ) ;
#18257 = CARTESIAN_POINT ( 'NONE',  ( 765.0180583372156207, -408.9982390220556567, -360.0135310231089534 ) ) ;
#18258 = VECTOR ( 'NONE', #29901, 1000.000000000000000 ) ;
#18259 = EDGE_CURVE ( 'NONE', #22319, #16495, #20077, .T. ) ;
#18260 = CARTESIAN_POINT ( 'NONE',  ( 770.0799878456142551, -37.98741447168752927, 362.9823548866085616 ) ) ;
#18261 = CARTESIAN_POINT ( 'NONE',  ( 783.7566961878529810, -72.89650538077830788, -305.1792804349288417 ) ) ;
#18262 = CARTESIAN_POINT ( 'NONE',  ( 746.0683387631852383, -211.4419599262324709, 331.3260364891676204 ) ) ;
#18263 = CARTESIAN_POINT ( 'NONE',  ( 764.8639956371174549, -56.08914811296581604, 319.7806653035542581 ) ) ;
#18264 = ORIENTED_EDGE ( 'NONE', *, *, #1528, .T. ) ;
#18265 = CARTESIAN_POINT ( 'NONE',  ( 776.9566956441375396, -204.8965053807779100, -364.8461984189686405 ) ) ;
#18266 = EDGE_CURVE ( 'NONE', #7675, #10697, #40225, .T. ) ;
#18267 = CARTESIAN_POINT ( 'NONE',  ( 801.9419747391806368, -186.4527844766017779, 351.9812246680014027 ) ) ;
#18268 = EDGE_CURVE ( 'NONE', #33524, #44027, #9258, .T. ) ;
#18269 = CARTESIAN_POINT ( 'NONE',  ( 778.7502325331095108, -24.35105083532392811, -304.6391490659818828 ) ) ;
#18270 = CARTESIAN_POINT ( 'NONE',  ( 803.6646147819162707, -329.9073299311467622, 348.8264449731211130 ) ) ;
#18271 = DIRECTION ( 'NONE',  ( -1.000000000000000000, -0.000000000000000000, -0.000000000000000000 ) ) ;
#18272 = CARTESIAN_POINT ( 'NONE',  ( 799.9999999999993179, 205.0000000000000568, -360.0000000000000000 ) ) ;
#18273 = EDGE_LOOP ( 'NONE', ( #24262, #19964 ) ) ;
#18274 = CARTESIAN_POINT ( 'NONE',  ( 759.2295555964440155, -40.16923265350570915, 353.9708237608231229 ) ) ;
#18275 = CARTESIAN_POINT ( 'NONE',  ( 754.3581564841646241, -329.4636090269706870, -316.1443688327762516 ) ) ;
#18276 = CARTESIAN_POINT ( 'NONE',  ( 808.3070685750232087, -306.9982390220558841, 361.1904061080339829 ) ) ;
#18277 = CARTESIAN_POINT ( 'NONE',  ( 744.9990715423526808, 5.648949164675971524, 341.2370466360926002 ) ) ;
#18278 = CARTESIAN_POINT ( 'NONE',  ( 772.4468031744293057, -201.8272453906073451, -363.8651313633793620 ) ) ;
#18279 = CARTESIAN_POINT ( 'NONE',  ( 754.8072714833581358, -196.8164208402380950, -338.1981804954720587 ) ) ;
#18280 = CARTESIAN_POINT ( 'NONE',  ( 774.6312213355098493, -359.3618753856921444, -364.6798772138717482 ) ) ;
#18281 = VERTEX_POINT ( 'NONE', #41339 ) ;
#18282 = CARTESIAN_POINT ( 'NONE',  ( 789.5670355615794733, -453.0432664090020012, -363.0970091259334822 ) ) ;
#18283 = CARTESIAN_POINT ( 'NONE',  ( 814.5518280994195948, -279.7255117493288026, 332.4837098697145734 ) ) ;
#18284 = CARTESIAN_POINT ( 'NONE',  ( 701.1634899080286232, 229.9999999999999147, -202.7499999999988916 ) ) ;
#18285 = DIRECTION ( 'NONE',  ( -1.000000000000000000, 0.000000000000000000, 0.000000000000000000 ) ) ;
#18286 = CARTESIAN_POINT ( 'NONE',  ( 796.1575198192839480, -174.0090635724256742, 359.4546378042384163 ) ) ;
#18287 = CARTESIAN_POINT ( 'NONE',  ( 794.9819416627830151, -36.99823902205679360, 319.9864689768909898 ) ) ;
#18288 = ORIENTED_EDGE ( 'NONE', *, *, #15112, .F. ) ;
#18289 = CARTESIAN_POINT ( 'NONE',  ( 807.2620300519052989, -408.0090635724249069, -318.0141637701419768 ) ) ;
#18290 = CARTESIAN_POINT ( 'NONE',  ( 810.7187646348534145, 5.547215523397618142, -356.7737145352016341 ) ) ;
#18291 = CARTESIAN_POINT ( 'NONE',  ( 810.4231160770870019, -264.5545181178798657, 321.9338519418446936 ) ) ;
#18292 = CARTESIAN_POINT ( 'NONE',  ( 755.0488828828309806, -209.8055962898687881, 344.1219089521771934 ) ) ;
#18293 = CARTESIAN_POINT ( 'NONE',  ( 768.0187753319979720, -368.6346026584193964, -318.0580252608186242 ) ) ;
#18294 = DIRECTION ( 'NONE',  ( 0.000000000000000000, 0.000000000000000000, 1.000000000000000000 ) ) ;
#18295 = CARTESIAN_POINT ( 'NONE',  ( 788.8264449731200330, 2.819942796124898177, 363.6646147819171233 ) ) ;
#18296 = CARTESIAN_POINT ( 'NONE',  ( -919.9999999999993179, 219.9999999999998863, 350.0000000000000000 ) ) ;
#18297 = CARTESIAN_POINT ( 'NONE',  ( 790.0220218866281812, -271.0999726633344267, -363.2186876482849129 ) ) ;
#18298 = CARTESIAN_POINT ( 'NONE',  ( 792.3570229623688874, 2.819942796124898177, 373.1304606946836202 ) ) ;
#18299 = CARTESIAN_POINT ( 'NONE',  ( 800.9747183278959710, -108.9982390220565804, 311.9810565676471583 ) ) ;
#18300 = PLANE ( 'NONE',  #16605 ) ;
#18301 = CARTESIAN_POINT ( 'NONE',  ( 801.1904061080338124, -452.0891481129646081, -368.3070685750236066 ) ) ;
#18302 = FACE_OUTER_BOUND ( 'NONE', #40600, .T. ) ;
#18303 = CARTESIAN_POINT ( 'NONE',  ( 788.6739635108323228, -391.6454272087885897, 373.9316612368139090 ) ) ;
#18304 = EDGE_CURVE ( 'NONE', #33295, #24190, #33578, .T. ) ;
#18305 = CARTESIAN_POINT ( 'NONE',  ( -200.7583438952259485, 394.6698570112193920, -244.9999999999999716 ) ) ;
#18306 = CARTESIAN_POINT ( 'NONE',  ( 744.7301800767019131, -316.8164208402377540, 337.4774526936615757 ) ) ;
#18307 = CARTESIAN_POINT ( 'NONE',  ( 772.5602148656447525, -105.7255117493293000, -305.7998596910095443 ) ) ;
#18308 = CARTESIAN_POINT ( 'NONE',  ( 768.0187753319979720, -272.6346026584196807, -318.0580252608186242 ) ) ;
#18309 = DIRECTION ( 'NONE',  ( -1.000000000000000000, 0.000000000000000000, -0.000000000000000000 ) ) ;
#18310 = CARTESIAN_POINT ( 'NONE',  ( 755.5713283507202505, -413.3618753856920307, 334.6858677611754729 ) ) ;
#18311 = CARTESIAN_POINT ( 'NONE',  ( 784.1219089521767955, -189.2817908451528979, 315.0488828828318333 ) ) ;
#18312 = CARTESIAN_POINT ( 'NONE',  ( 814.4686193811664907, -75.28179084515321051, -346.2056067578752732 ) ) ;
#18313 = CARTESIAN_POINT ( 'NONE',  ( 783.0433043558608688, -96.89650538077825104, -315.1538015810313027 ) ) ;
#18314 = CARTESIAN_POINT ( 'NONE',  ( 807.5423716828161105, -105.0783235625964096, 362.2119215644372048 ) ) ;
#18315 = CARTESIAN_POINT ( 'NONE',  ( 778.1981804954715471, -418.2709662947828519, 314.8072714833591021 ) ) ;
#18316 = AXIS2_PLACEMENT_3D ( 'NONE', #25454, #21762, #64 ) ;
#18317 = CARTESIAN_POINT ( 'NONE',  ( 804.4286716492782716, -449.3618753856918602, 345.3141322388244703 ) ) ;
#18319 = VERTEX_POINT ( 'NONE', #2770 ) ;
#18318 = CARTESIAN_POINT ( 'NONE',  ( 757.2208543904082489, -112.7146871989600356, -350.9844846989624330 ) ) ;
#18320 = CARTESIAN_POINT ( 'NONE',  ( 756.3353852180819104, -101.9073299311474727, -331.1735550268788302 ) ) ;
#18321 = CARTESIAN_POINT ( 'NONE',  ( 803.2186876482843445, -415.9874144716862361, -350.0220218866286928 ) ) ;
#18323 = CARTESIAN_POINT ( 'NONE',  ( 802.1676090361155502, -230.6346026584197944, 327.8955696845344505 ) ) ;
#18322 = CARTESIAN_POINT ( 'NONE',  ( 804.4286716492782716, -233.3618753856925423, 345.3141322388244703 ) ) ;
#18324 = CARTESIAN_POINT ( 'NONE',  ( 805.9055244015594326, -387.6237781080499758, -315.8990559732753240 ) ) ;
#18325 = DIRECTION ( 'NONE',  ( -0.000000000000000000, 1.000000000000000000, -0.000000000000000000 ) ) ;
#18326 = ORIENTED_EDGE ( 'NONE', *, *, #28143, .T. ) ;
#18327 = CARTESIAN_POINT ( 'NONE',  ( 755.0636971347428243, -436.2709662947827951, 341.7834795799807353 ) ) ;
#18328 = VERTEX_POINT ( 'NONE', #156 ) ;
#18329 = CARTESIAN_POINT ( 'NONE',  ( 754.9967657858570647, -193.5436935675108714, 365.0032342141425943 ) ) ;
#18330 = CARTESIAN_POINT ( 'NONE',  ( 776.9254006560222479, -260.1908817542435486, 314.8983024940802125 ) ) ;
#18331 = ORIENTED_EDGE ( 'NONE', *, *, #33345, .F. ) ;
#18332 = CARTESIAN_POINT ( 'NONE',  ( 799.2566176426618085, -72.00906357242594424, -324.0069404352559559 ) ) ;
#18333 = CARTESIAN_POINT ( 'NONE',  ( 766.5853460496234675, -229.9874144716869466, 372.3518521366060554 ) ) ;
#18334 = CARTESIAN_POINT ( 'NONE',  ( 801.9419747391806368, -258.4527844766016074, -351.9812246680014027 ) ) ;
#18335 = ORIENTED_EDGE ( 'NONE', *, *, #15654, .T. ) ;
#18336 = CARTESIAN_POINT ( 'NONE',  ( 805.1927285166397041, -400.8164208402373561, -341.8018195045277707 ) ) ;
#18337 = CARTESIAN_POINT ( 'NONE',  ( 791.9812246680005501, -44.63460265842040542, -361.9419747391813189 ) ) ;
#18338 = CARTESIAN_POINT ( 'NONE',  ( 780.5290396650775619, -252.3510508353232353, 365.2837595273619513 ) ) ;
#18339 = DIRECTION ( 'NONE',  ( 1.000000000000000000, -0.000000000000000000, -0.000000000000000000 ) ) ;
#18340 = LINE ( 'NONE', #25235, #40368 ) ;
#18341 = CARTESIAN_POINT ( 'NONE',  ( 800.0135310231082713, -14.08914811296595460, -325.0180583372163028 ) ) ;
#18342 = CARTESIAN_POINT ( 'NONE',  ( 999.9999999999992042, -600.0000000000001137, 360.0000000000000000 ) ) ;
#18343 = CARTESIAN_POINT ( 'NONE',  ( 989.9999999999992042, 50.81038600091411439, 193.6948738798775764 ) ) ;
#18344 = ORIENTED_EDGE ( 'NONE', *, *, #5817, .F. ) ;
#18345 = CARTESIAN_POINT ( 'NONE',  ( 809.0717654672305343, -316.9181544815160692, -360.1688906516309885 ) ) ;
#18346 = CARTESIAN_POINT ( 'NONE',  ( 745.7194118038753459, -181.6454272087892434, 348.7631598425976449 ) ) ;
#18347 = VECTOR ( 'NONE', #9864, 1000.000000000000000 ) ;
#18349 = CARTESIAN_POINT ( 'NONE',  ( 767.8955696845333705, -264.4527844766016074, -362.1676090361162323 ) ) ;
#18348 = CARTESIAN_POINT ( 'NONE',  ( 999.9999999999992042, -600.0000000000001137, 360.0000000000000000 ) ) ;
#18350 = CARTESIAN_POINT ( 'NONE',  ( 784.4999999999993179, -544.8427095258973623, -350.0000000000000000 ) ) ;
#18351 = CARTESIAN_POINT ( 'NONE',  ( 773.4516893846965786, -115.6454272087894424, -315.8398074228977066 ) ) ;
#18352 = CARTESIAN_POINT ( 'NONE',  ( 782.5225473063381969, -22.27096629478410250, 375.2698199232970637 ) ) ;
#18353 = LINE ( 'NONE', #11856, #17322 ) ;
#18354 = CARTESIAN_POINT ( 'NONE',  ( 748.9653473494365699, -338.6346026584195101, -356.9462024416520762 ) ) ;
#18355 = PLANE ( 'NONE',  #10629 ) ;
#18356 = CARTESIAN_POINT ( 'NONE',  ( 788.8264449731200330, 2.819942796124898177, 363.6646147819171233 ) ) ;
#18357 = CARTESIAN_POINT ( 'NONE',  ( 745.1792804349281596, -278.1908817542434917, 343.7566961878542884 ) ) ;
#18358 = CARTESIAN_POINT ( 'NONE',  ( 773.7943932421234194, -191.8055962898689017, -305.5313806188329409 ) ) ;
#18359 = CARTESIAN_POINT ( 'NONE',  ( 804.7487373415286811, -211.5436935675107861, 364.7487373415288516 ) ) ;
#18360 = CARTESIAN_POINT ( 'NONE',  ( 801.1904061080336987, 3.910851887033985896, -368.3070685750235498 ) ) ;
#18361 = FACE_OUTER_BOUND ( 'NONE', #42921, .T. ) ;
#18362 = ORIENTED_EDGE ( 'NONE', *, *, #8497, .T. ) ;
#18363 = CARTESIAN_POINT ( 'NONE',  ( 795.1360043628807261, -332.0891481129649492, 360.2193346964456282 ) ) ;
#18364 = EDGE_CURVE ( 'NONE', #11223, #17152, #14246, .T. ) ;
#18365 = CARTESIAN_POINT ( 'NONE',  ( 759.0159684113467620, -88.91815448151682233, 325.8855110935213020 ) ) ;
#18366 = CARTESIAN_POINT ( 'NONE',  ( 765.8855110935204493, 25.83076734649409545, -319.0159684113471599 ) ) ;
#18367 = DIRECTION ( 'NONE',  ( 0.000000000000000000, 0.000000000000000000, 1.000000000000000000 ) ) ;
#18368 = CARTESIAN_POINT ( 'NONE',  ( 794.9999999999993179, -373.0259173205825505, -36.60293108048681887 ) ) ;
#18370 = CARTESIAN_POINT ( 'NONE',  ( 781.7834795799800531, -370.8164208402375834, 315.0636971347436202 ) ) ;
#18369 = CARTESIAN_POINT ( 'NONE',  ( 805.0264073115434940, -150.3510508353235480, 339.4763451958999099 ) ) ;
#18371 = VERTEX_POINT ( 'NONE', #20307 ) ;
#18372 = CARTESIAN_POINT ( 'NONE',  ( 800.7704444035546203, -292.1692326535048210, -326.0291762391768771 ) ) ;
#18373 = CARTESIAN_POINT ( 'NONE',  ( 768.8385539511368734, -311.2601417444139429, -306.4236121716840557 ) ) ;
#18374 = FACE_OUTER_BOUND ( 'NONE', #7105, .T. ) ;
#18375 = CARTESIAN_POINT ( 'NONE',  ( 803.8556311672234642, -441.6237781080499190, 365.6418435158340117 ) ) ;
#18376 = ORIENTED_EDGE ( 'NONE', *, *, #36838, .F. ) ;
#18377 = CARTESIAN_POINT ( 'NONE',  ( 765.0180583372156207, -336.9982390220558273, 360.0135310231089534 ) ) ;
#18378 = CARTESIAN_POINT ( 'NONE',  ( 756.1348686366196716, -65.26014174441471027, -347.5531968255698416 ) ) ;
#18379 = CYLINDRICAL_SURFACE ( 'NONE', #33500, 30.00000000000008171 ) ;
#18380 = CARTESIAN_POINT ( 'NONE',  ( 744.7301800767019131, -148.8164208402382656, -337.4774526936615757 ) ) ;
#18381 = ORIENTED_EDGE ( 'NONE', *, *, #36740, .F. ) ;
#18382 = CARTESIAN_POINT ( 'NONE',  ( 774.6858677611749044, -153.7255117493291721, -315.5713283507209894 ) ) ;
#18383 = EDGE_LOOP ( 'NONE', ( #24195, #9552, #42841, #10704 ) ) ;
#18384 = CARTESIAN_POINT ( 'NONE',  ( 772.4468031744293057, -417.8272453906067199, -363.8651313633793620 ) ) ;
#18385 = CARTESIAN_POINT ( 'NONE',  ( 798.5707757039680246, -461.4636090269701754, 356.7845633553585003 ) ) ;
#18386 = CARTESIAN_POINT ( 'NONE',  ( 759.0252816721024374, -216.9982390220562252, 368.0189434323527280 ) ) ;
#18387 = CARTESIAN_POINT ( 'NONE',  ( 772.3691319403857278, -119.2601417444145397, 315.8894580844506663 ) ) ;
#18390 = CARTESIAN_POINT ( 'NONE',  ( 766.5853460496234675, -397.9874144716864066, 372.3518521366060554 ) ) ;
#18389 = CARTESIAN_POINT ( 'NONE',  ( 181.1634899080285948, 240.0000000000000284, -202.7499999999952536 ) ) ;
#18388 = CARTESIAN_POINT ( 'NONE',  ( 794.9999999999993179, 205.0000000000000568, -255.0000000000000000 ) ) ;
#18391 = ORIENTED_EDGE ( 'NONE', *, *, #8646, .F. ) ;
#18392 = CARTESIAN_POINT ( 'NONE',  ( 760.7433823573367135, -396.0090635724249637, -355.9930595647440441 ) ) ;
#18393 = FACE_OUTER_BOUND ( 'NONE', #24886, .T. ) ;
#18394 = CARTESIAN_POINT ( 'NONE',  ( 799.9636004259356241, -166.9181544815165523, -311.2241431872006956 ) ) ;
#18395 = CARTESIAN_POINT ( 'NONE',  ( 773.7305795820266212, -81.28179084515319630, 374.8230680027170365 ) ) ;
#18397 = PLANE ( 'NONE',  #12947 ) ;
#18396 = FACE_OUTER_BOUND ( 'NONE', #36935, .T. ) ;
#18398 = CARTESIAN_POINT ( 'NONE',  ( 796.7845633553578182, -321.6237781080502600, -358.5707757039688204 ) ) ;
#18399 = LINE ( 'NONE', #11693, #32979 ) ;
#18400 = CARTESIAN_POINT ( 'NONE',  ( 788.6739635108323228, -175.6454272087892718, -373.9316612368139090 ) ) ;
#18401 = DIRECTION ( 'NONE',  ( 1.000000000000000000, 0.000000000000000000, 0.000000000000000000 ) ) ;
#18402 = CARTESIAN_POINT ( 'NONE',  ( 701.1634899080286232, 259.9999999999999432, -193.8809999999990623 ) ) ;
#18403 = CARTESIAN_POINT ( 'NONE',  ( 772.4468031744293057, -417.8272453906067199, 363.8651313633793620 ) ) ;
#18404 = CARTESIAN_POINT ( 'NONE',  ( 805.0032342141413437, -205.5436935675108145, -314.9967657858572352 ) ) ;
#18405 = LINE ( 'NONE', #18182, #16532 ) ;
#18406 = CARTESIAN_POINT ( 'NONE',  ( 801.9419747391806368, -18.45278447660230725, -351.9812246680014027 ) ) ;
#18407 = AXIS2_PLACEMENT_3D ( 'NONE', #45508, #21237, #13625 ) ;
#18408 = CARTESIAN_POINT ( 'NONE',  ( 760.0363995740630116, -130.9181544815166660, 368.7758568127991907 ) ) ;
#18409 = CARTESIAN_POINT ( 'NONE',  ( 761.9338519418445230, -86.53286901714194812, -370.4231160770881957 ) ) ;
#18410 = CARTESIAN_POINT ( 'NONE',  ( 796.7737145352015204, -116.6346026584201780, 370.7187646348536987 ) ) ;
#18411 = CARTESIAN_POINT ( 'NONE',  ( 811.0346526505616112, -326.6346026584193396, -323.0537975583477532 ) ) ;
#18412 = CARTESIAN_POINT ( 'NONE',  ( -773.4999999999993179, -494.6608068873671300, -357.6536686473015720 ) ) ;
#18413 = CARTESIAN_POINT ( 'NONE',  ( 181.1634899080285948, 260.0000000000000000, -202.7499999999952536 ) ) ;
#18414 = CARTESIAN_POINT ( 'NONE',  ( 774.6858677611749044, -225.7255117493289163, 315.5713283507209894 ) ) ;
#18415 = CARTESIAN_POINT ( 'NONE',  ( 799.2566176426618085, -0.009063572426172561425, 324.0069404352559559 ) ) ;
#18416 = CARTESIAN_POINT ( 'NONE',  ( 786.2056067578752163, -395.8055962898682765, -374.4686193811670023 ) ) ;
#18417 = CARTESIAN_POINT ( 'NONE',  ( 782.5225473063381969, -406.2709662947829088, -375.2698199232970637 ) ) ;
#18418 = CARTESIAN_POINT ( 'NONE',  ( 51.16348990802859475, 230.0000000000000284, -202.7499999999943441 ) ) ;
#18419 = CARTESIAN_POINT ( 'NONE',  ( 773.7943932421234194, -47.80559628986931386, 305.5313806188329409 ) ) ;
#18420 = EDGE_LOOP ( 'NONE', ( #33705, #25735, #44082, #3186, #16889, #10137 ) ) ;
#18421 = CARTESIAN_POINT ( 'NONE',  ( 799.4546378042377910, -177.0783235625961538, -356.1575198192848006 ) ) ;
#18422 = CARTESIAN_POINT ( 'NONE',  ( 797.8594530101008786, -37.54369356751132614, 322.1405469898980982 ) ) ;
#18423 = CARTESIAN_POINT ( 'NONE',  ( 813.2346286133761168, -197.2601417444143124, -328.9521613784389160 ) ) ;
#18424 = LINE ( 'NONE', #17962, #43022 ) ;
#18425 = CARTESIAN_POINT ( 'NONE',  ( 752.4576283171824116, -357.0783235625956422, 317.7880784355627952 ) ) ;
#18426 = CARTESIAN_POINT ( 'NONE',  ( 757.8323909638828582, -146.6346026584200786, 352.1044303154654358 ) ) ;
#18427 = VERTEX_POINT ( 'NONE', #28314 ) ;
#18428 = CARTESIAN_POINT ( 'NONE',  ( 800.0135310231082713, -134.0891481129655745, -325.0180583372163028 ) ) ;
#18429 = CARTESIAN_POINT ( 'NONE',  ( 765.0180583372156207, -336.9982390220558273, 360.0135310231089534 ) ) ;
#18430 = CARTESIAN_POINT ( 'NONE',  ( 808.0189434323515343, -38.08914811296587999, -319.0252816721025511 ) ) ;
#18431 = ADVANCED_FACE ( 'NONE', ( #9689 ), #43034, .T. ) ;
#18432 = ORIENTED_EDGE ( 'NONE', *, *, #18463, .F. ) ;
#18433 = CARTESIAN_POINT ( 'NONE',  ( 805.6418435158337843, -437.4636090269703459, -363.8556311672236916 ) ) ;
#18434 = AXIS2_PLACEMENT_3D ( 'NONE', #35989, #871, #7826 ) ;
#18435 = VERTEX_POINT ( 'NONE', #10532 ) ;
#18436 = CARTESIAN_POINT ( 'NONE',  ( 801.5560724626406000, -336.5545181178796952, -326.7756240680316182 ) ) ;
#18438 = CARTESIAN_POINT ( 'NONE',  ( 804.1105419155481968, -387.8272453906067767, 347.6308680596136469 ) ) ;
#18437 = CARTESIAN_POINT ( 'NONE',  ( 756.3353852180819104, -53.90732993114765037, 331.1735550268788302 ) ) ;
#18439 = CARTESIAN_POINT ( 'NONE',  ( 774.6312213355099630, -287.3618753856923718, -364.6798772138717482 ) ) ;
#18441 = CARTESIAN_POINT ( 'NONE',  ( 761.9338519418445230, -302.5328690171411949, 370.4231160770881957 ) ) ;
#18440 = CARTESIAN_POINT ( 'NONE',  ( 810.7187646348534145, -378.4527844766011526, 356.7737145352016341 ) ) ;
#18442 = CARTESIAN_POINT ( 'NONE',  ( 764.3348316497523456, -70.71468719896014932, 308.6759233522265617 ) ) ;
#18443 = CARTESIAN_POINT ( 'NONE',  ( 783.0745993439762742, -272.1908817542434917, -365.1016975059196739 ) ) ;
#18444 = CARTESIAN_POINT ( 'NONE',  ( 765.0180583372156207, -288.9982390220559978, -360.0135310231089534 ) ) ;
#18445 = CARTESIAN_POINT ( 'NONE',  ( 959.5497976682736407, 239.9999999999998863, -2132.806278688367456 ) ) ;
#18446 = CARTESIAN_POINT ( 'NONE',  ( 792.1044303154645831, -132.4527844766018916, -317.8323909638837677 ) ) ;
#18447 = CARTESIAN_POINT ( 'NONE',  ( 794.9999999999993179, -365.3551492539851893, -8.132432514707076621 ) ) ;
#18448 = ORIENTED_EDGE ( 'NONE', *, *, #44480, .T. ) ;
#18449 = CARTESIAN_POINT ( 'NONE',  ( 796.7737145352015204, -428.6346026584192259, 370.7187646348536987 ) ) ;
#18451 = DIRECTION ( 'NONE',  ( 0.000000000000000000, 1.000000000000000000, 0.000000000000000000 ) ) ;
#18450 = DIRECTION ( 'NONE',  ( 0.000000000000000000, 0.000000000000000000, -1.000000000000000000 ) ) ;
#18452 = CARTESIAN_POINT ( 'NONE',  ( 813.5763878283155464, -75.82724539060775726, -351.1614460488615350 ) ) ;
#18453 = CARTESIAN_POINT ( 'NONE',  ( -521.6730038022809595, 230.0000000000001421, -2132.806278688367456 ) ) ;
#18454 = DIRECTION ( 'NONE',  ( -1.000000000000000000, -0.000000000000000000, -0.000000000000000000 ) ) ;
#18455 = EDGE_CURVE ( 'NONE', #6, #16721, #35016, .T. ) ;
#18456 = CARTESIAN_POINT ( 'NONE',  ( 766.9102291470427417, -258.5545181178799226, 318.6633372737382501 ) ) ;
#18457 = CARTESIAN_POINT ( 'NONE',  ( 756.3353852180819104, -149.9073299311473875, 331.1735550268788302 ) ) ;
#18458 = ORIENTED_EDGE ( 'NONE', *, *, #39900, .T. ) ;
#18459 = CARTESIAN_POINT ( 'NONE',  ( 789.9200121543843807, -313.9874144716866908, 317.0176451133914384 ) ) ;
#18460 = CARTESIAN_POINT ( 'NONE',  ( 790.8050863131179540, -452.8379544210779954, -362.5841948692291226 ) ) ;
#18461 = CARTESIAN_POINT ( 'NONE',  ( 773.7305795820266212, -57.28179084515326736, 374.8230680027170365 ) ) ;
#18462 = CARTESIAN_POINT ( 'NONE',  ( 772.4837098697144029, -239.3618753856924570, -374.5518280994205611 ) ) ;
#18463 = EDGE_CURVE ( 'NONE', #13016, #40052, #45433, .T. ) ;
#18464 = CARTESIAN_POINT ( 'NONE',  ( 755.2512626584698410, -199.5436935675108430, 315.2512626584710915 ) ) ;
#18465 = CARTESIAN_POINT ( 'NONE',  ( 785.3687786644884454, -107.3618753856928976, 315.3201227861279676 ) ) ;
#18466 = DIRECTION ( 'NONE',  ( -1.000000000000000000, -4.625929269271485914E-16, -0.000000000000000000 ) ) ;
#18467 = CARTESIAN_POINT ( 'NONE',  ( 798.0661480581538854, -314.5328690171411949, -309.5768839229118043 ) ) ;
#18468 = CARTESIAN_POINT ( 'NONE',  ( 794.5607502887775127, -462.9631818684622999, 371.8524697363486666 ) ) ;
#18469 = CARTESIAN_POINT ( 'NONE',  ( 811.0346526505616112, -326.6346026584193396, -323.0537975583477532 ) ) ;
#18470 = LINE ( 'NONE', #32549, #20231 ) ;
#18471 = CARTESIAN_POINT ( 'NONE',  ( 755.8398074228967971, -403.4419599262317888, 333.4516893846970333 ) ) ;
#18472 = EDGE_LOOP ( 'NONE', ( #33693, #28426, #22247, #20631 ) ) ;
#18473 = DIRECTION ( 'NONE',  ( -0.000000000000000000, -0.000000000000000000, -1.000000000000000000 ) ) ;
#18474 = CARTESIAN_POINT ( 'NONE',  ( 803.6646147819161570, -425.9073299311463074, -348.8264449731210561 ) ) ;
#18475 = CARTESIAN_POINT ( 'NONE',  ( 760.5453621957607311, -69.07832356259653750, 323.8424801807151425 ) ) ;
#18476 = CARTESIAN_POINT ( 'NONE',  ( 801.9419747391806368, -210.4527844766016926, -351.9812246680014027 ) ) ;
#18477 = CARTESIAN_POINT ( 'NONE',  ( 813.2346286133761168, -77.26014174441466764, -328.9521613784389160 ) ) ;
#18479 = ADVANCED_FACE ( 'NONE', ( #28786 ), #3844, .F. ) ;
#18478 = FACE_OUTER_BOUND ( 'NONE', #7396, .T. ) ;
#18480 = CARTESIAN_POINT ( 'NONE',  ( 776.2433038121456548, -204.8965053807779100, 374.8207195650711014 ) ) ;
#18481 = CARTESIAN_POINT ( 'NONE',  ( 759.9864689768902508, -50.08914811296584446, 354.9819416627836404 ) ) ;
#18482 = EDGE_CURVE ( 'NONE', #8774, #37957, #17487, .T. ) ;
#18483 = EDGE_LOOP ( 'NONE', ( #11501, #24542, #43974, #3252 ) ) ;
#18484 = CARTESIAN_POINT ( 'NONE',  ( 804.9511171171677688, -221.8055962898687881, -335.8780910478229202 ) ) ;
#18485 = CARTESIAN_POINT ( 'NONE',  ( 800.2193346964447755, -234.9982390220561683, 355.1360043628815788 ) ) ;
#18486 = CARTESIAN_POINT ( 'NONE',  ( 811.6461892240364477, -52.71468719896020616, -324.1737431748509835 ) ) ;
#18487 = CARTESIAN_POINT ( 'NONE',  ( 800.0135310231082713, -350.0891481129648923, 325.0180583372163028 ) ) ;
#18488 = EDGE_CURVE ( 'NONE', #38048, #39281, #18108, .T. ) ;
#18489 = LINE ( 'NONE', #39748, #39450 ) ;
#18490 = ORIENTED_EDGE ( 'NONE', *, *, #31734, .F. ) ;
#18491 = CARTESIAN_POINT ( 'NONE',  ( 752.7379699480933368, -348.0090635724251342, -361.9858362298580232 ) ) ;
#18492 = CARTESIAN_POINT ( 'NONE',  ( 812.7932403749906598, -279.1800572038741848, 327.7687537140311633 ) ) ;
#18493 = CARTESIAN_POINT ( 'NONE',  ( 781.2497674668890113, -12.35105083532396897, 375.3608509340180603 ) ) ;
#18494 = CARTESIAN_POINT ( 'NONE',  ( 776.9254006560222479, -188.1908817542437760, -314.8983024940802125 ) ) ;
#18495 = CARTESIAN_POINT ( 'NONE',  ( 757.8323909638827445, -170.6346026584199649, -352.1044303154654358 ) ) ;
#18496 = CARTESIAN_POINT ( 'NONE',  ( 758.0580252608178853, -390.4527844766011526, -328.0187753319985404 ) ) ;
#18497 = ORIENTED_EDGE ( 'NONE', *, *, #33183, .T. ) ;
#18498 = EDGE_LOOP ( 'NONE', ( #30572, #22263, #36421, #1164, #8876, #26980, #18331 ) ) ;
#18499 = CARTESIAN_POINT ( 'NONE',  ( 777.5031285880264704, -286.8164208402378677, 374.9108240113588408 ) ) ;
#18500 = EDGE_CURVE ( 'NONE', #5810, #26734, #42648, .T. ) ;
#18501 = CARTESIAN_POINT ( 'NONE',  ( 181.1634899080285948, 260.0000000000000000, -208.0249999999954014 ) ) ;
#18502 = CARTESIAN_POINT ( 'NONE',  ( 804.4086373105744769, -217.6454272087891582, 333.3843516231986541 ) ) ;
#18503 = CARTESIAN_POINT ( 'NONE',  ( -37.63011601220122770, -512.9681489794448908, -339.9999999999999432 ) ) ;
#18504 = ADVANCED_FACE ( 'NONE', ( #14018 ), #25077, .T. ) ;
#18505 = CARTESIAN_POINT ( 'NONE',  ( 801.5560724626406000, -144.5545181178802636, 326.7756240680316182 ) ) ;
#18506 = CARTESIAN_POINT ( 'NONE',  ( 759.9864689768902508, -50.08914811296584446, 354.9819416627836404 ) ) ;
#18507 = EDGE_LOOP ( 'NONE', ( #23773, #43014 ) ) ;
#18508 = CARTESIAN_POINT ( 'NONE',  ( 768.9521613784389729, -417.8272453906067199, -373.2346286133773106 ) ) ;
#18509 = CARTESIAN_POINT ( 'NONE',  ( 805.6418435158337843, -269.4636090269708006, 363.8556311672236916 ) ) ;
#18510 = CARTESIAN_POINT ( 'NONE',  ( 800.7704444035546203, -220.1692326535051052, 326.0291762391768771 ) ) ;
#18511 = CARTESIAN_POINT ( 'NONE',  ( 771.1735550268778070, -345.1800572038739006, -316.3353852180827630 ) ) ;
#18512 = CARTESIAN_POINT ( 'NONE',  ( 989.9999999999992042, 62.79977829742938411, 207.3621835540872951 ) ) ;
#18513 = CARTESIAN_POINT ( 'NONE',  ( 754.8072714833581358, -4.816420840238714085, 338.1981804954720587 ) ) ;
#18514 = DIRECTION ( 'NONE',  ( 0.000000000000000000, -1.000000000000000000, 0.000000000000000000 ) ) ;
#18515 = CARTESIAN_POINT ( 'NONE',  ( 804.4086373105744769, -241.6454272087890729, -333.3843516231986541 ) ) ;
#18516 = ADVANCED_FACE ( 'NONE', ( #25304 ), #7768, .T. ) ;
#18517 = CARTESIAN_POINT ( 'NONE',  ( 782.4968714119720516, -34.81642084023861372, 305.0891759886411023 ) ) ;
#18518 = CARTESIAN_POINT ( 'NONE',  ( 747.2067596250078623, -99.18005720387478164, 352.2312462859687230 ) ) ;
#18519 = CYLINDRICAL_SURFACE ( 'NONE', #18825, 10.00000000000000888 ) ;
#18520 = SURFACE_SIDE_STYLE ('',( #28905 ) ) ;
#18521 = CARTESIAN_POINT ( 'NONE',  ( 754.3581564841646241, -377.4636090269704596, 316.1443688327762516 ) ) ;
#18522 = DIRECTION ( 'NONE',  ( 1.000000000000000000, 0.000000000000000000, 0.000000000000000000 ) ) ;
#18523 = CARTESIAN_POINT ( 'NONE',  ( 777.5031285880264704, -310.8164208402377540, 374.9108240113588408 ) ) ;
#18524 = CARTESIAN_POINT ( 'NONE',  ( 788.7366044899766848, -323.9073299311468190, -316.5762568750059813 ) ) ;
#18525 = LINE ( 'NONE', #32606, #29161 ) ;
#18526 = CARTESIAN_POINT ( 'NONE',  ( 778.1981804954714335, -442.2709662947826814, 314.8072714833589885 ) ) ;
#18527 = CARTESIAN_POINT ( 'NONE',  ( 775.8780910478218402, -201.2817908451528126, 364.9511171171680530 ) ) ;
#18528 = CARTESIAN_POINT ( 'NONE',  ( 746.4236121716829757, -63.82724539060779279, -328.8385539511384650 ) ) ;
#18529 = CARTESIAN_POINT ( 'NONE',  ( 764.0069404352550464, -135.0783235625962959, -359.2566176426627180 ) ) ;
#18530 = CARTESIAN_POINT ( 'NONE',  ( 756.1443688327750579, -117.6237781080509279, 314.3581564841659315 ) ) ;
#18531 = CARTESIAN_POINT ( 'NONE',  ( 765.0180583372156207, -432.9982390220555999, 360.0135310231089534 ) ) ;
#18532 = EDGE_CURVE ( 'NONE', #22342, #23098, #38746, .T. ) ;
#18533 = CARTESIAN_POINT ( 'NONE',  ( 776.2433038121456548, -156.8965053807780805, 374.8207195650711014 ) ) ;
#18534 = CARTESIAN_POINT ( 'NONE',  ( 755.5713283507202505, -5.361875385693257279, -334.6858677611754729 ) ) ;
#18536 = ORIENTED_EDGE ( 'NONE', *, *, #5443, .T. ) ;
#18535 = CARTESIAN_POINT ( 'NONE',  ( 754.9735926884551418, -138.3510508353236048, -340.5236548041000333 ) ) ;
#18537 = CARTESIAN_POINT ( 'NONE',  ( 802.1676090361156639, -110.6346026584201638, -327.8955696845344505 ) ) ;
#18538 = CARTESIAN_POINT ( 'NONE',  ( 799.4546378042377910, -393.0783235625954717, -356.1575198192848006 ) ) ;
#18540 = CARTESIAN_POINT ( 'NONE',  ( 794.9819416627830151, -276.9982390220559978, 319.9864689768909898 ) ) ;
#18539 = CARTESIAN_POINT ( 'NONE',  ( 788.8264449731200330, -261.1800572038741848, 363.6646147819171233 ) ) ;
#18541 = AXIS2_PLACEMENT_3D ( 'NONE', #26822, #16441, #8840 ) ;
#18542 = CARTESIAN_POINT ( 'NONE',  ( 799.9999999999993179, 205.0000000000000568, 255.0000000000000000 ) ) ;
#18543 = ORIENTED_EDGE ( 'NONE', *, *, #22489, .F. ) ;
#18544 = CARTESIAN_POINT ( 'NONE',  ( 804.9363028652555840, -424.2709662947829088, 338.2165204200192079 ) ) ;
#18545 = ORIENTED_EDGE ( 'NONE', *, *, #26159, .F. ) ;
#18546 = CARTESIAN_POINT ( 'NONE',  ( 751.6929314249750860, -198.9982390220562536, 318.8095938919659034 ) ) ;
#18547 = CARTESIAN_POINT ( 'NONE',  ( 775.8780910478218402, -273.2817908451526137, 364.9511171171680530 ) ) ;
#18548 = ORIENTED_EDGE ( 'NONE', *, *, #10556, .T. ) ;
#18549 = CARTESIAN_POINT ( 'NONE',  ( 757.0176451133909268, -85.09997266333499510, -349.9200121543848354 ) ) ;
#18550 = CARTESIAN_POINT ( 'NONE',  ( 807.5423716828161105, -201.0783235625961254, 362.2119215644372048 ) ) ;
#18551 = CARTESIAN_POINT ( 'NONE',  ( 755.0636971347428243, -244.2709662947834204, -341.7834795799807353 ) ) ;
#18552 = ORIENTED_EDGE ( 'NONE', *, *, #31423, .T. ) ;
#18553 = CARTESIAN_POINT ( 'NONE',  ( 804.4286716492782716, -401.3618753856920307, -345.3141322388244703 ) ) ;
#18554 = CARTESIAN_POINT ( 'NONE',  ( 792.1044303154645831, -60.45278447660215448, -317.8323909638837677 ) ) ;
#18555 = ADVANCED_FACE ( 'NONE', ( #33159 ), #1710, .F. ) ;
#18556 = CARTESIAN_POINT ( 'NONE',  ( 779.4709603349208464, -264.3510508353232353, 314.7162404726379918 ) ) ;
#18557 = DIRECTION ( 'NONE',  ( 0.000000000000000000, 0.000000000000000000, -1.000000000000000000 ) ) ;
#18558 = DIRECTION ( 'NONE',  ( -1.000000000000000000, 1.892425610156518354E-16, 0.000000000000000000 ) ) ;
#18559 = EDGE_CURVE ( 'NONE', #34504, #36537, #4746, .T. ) ;
#18560 = CARTESIAN_POINT ( 'NONE',  ( 801.9419747391806368, -18.45278447660230725, -351.9812246680014027 ) ) ;
#18561 = CARTESIAN_POINT ( 'NONE',  ( -598.8365100919716042, 230.0000000000001421, -199.9999999999899671 ) ) ;
#18562 = ORIENTED_EDGE ( 'NONE', *, *, #44085, .F. ) ;
#18563 = CARTESIAN_POINT ( 'NONE',  ( 805.6418435158337843, -293.4636090269707438, -363.8556311672236916 ) ) ;
#18564 = CARTESIAN_POINT ( 'NONE',  ( 746.4236121716829757, -159.8272453906075157, 328.8385539511384650 ) ) ;
#18566 = CARTESIAN_POINT ( 'NONE',  ( 756.5762568750052424, -267.1800572038742985, -348.7366044899774238 ) ) ;
#18565 = CARTESIAN_POINT ( 'NONE',  ( 799.9999999999993179, 205.0000000000000568, -255.0000000000000000 ) ) ;
#18567 = CARTESIAN_POINT ( 'NONE',  ( 755.3028492785439312, -135.2817908451530116, -335.9200461376539693 ) ) ;
#18568 = EDGE_CURVE ( 'NONE', #22786, #25461, #18399, .T. ) ;
#18569 = CARTESIAN_POINT ( 'NONE',  ( 745.0891759886404770, -28.27096629478409540, 342.4968714119734159 ) ) ;
#18570 = VECTOR ( 'NONE', #43437, 1000.000000000000000 ) ;
#18571 = DIRECTION ( 'NONE',  ( -1.000000000000000000, -0.000000000000000000, -0.000000000000000000 ) ) ;
#18572 = CARTESIAN_POINT ( 'NONE',  ( 791.1614460488616487, -11.26014174441488258, -373.5763878283158874 ) ) ;
#18573 = CARTESIAN_POINT ( 'NONE',  ( 767.7687537140311633, -359.9073299311467053, -372.7932403749916830 ) ) ;
#18574 = DIRECTION ( 'NONE',  ( 0.000000000000000000, -0.6438296778008192334, -0.7651688349527138167 ) ) ;
#18575 = CARTESIAN_POINT ( 'NONE',  ( 767.8955696845333705, -24.45278447660229304, 362.1676090361162323 ) ) ;
#18576 = CARTESIAN_POINT ( 'NONE',  ( 812.3518521366052028, -289.0999726633343698, 326.5853460496235243 ) ) ;
#18577 = CARTESIAN_POINT ( 'NONE',  ( 744.8212110874229666, -234.8965053807777963, -336.2046728542121627 ) ) ;
#18578 = CARTESIAN_POINT ( 'NONE',  ( 759.0252816721024374, -240.9982390220561683, 368.0189434323527280 ) ) ;
#18579 = CARTESIAN_POINT ( 'NONE',  ( 796.7737145352015204, 3.365397341579444479, -370.7187646348536987 ) ) ;
#18580 = FACE_BOUND ( 'NONE', #24575, .T. ) ;
#18581 = EDGE_LOOP ( 'NONE', ( #21312, #15630, #24308, #29750 ) ) ;
#18582 = CARTESIAN_POINT ( 'NONE',  ( 797.6776695296629214, -331.5436935675104451, 357.6776695296636603 ) ) ;
#18583 = CARTESIAN_POINT ( 'NONE',  ( 800.9840315886518738, -100.9181544815167513, 354.1144889064786412 ) ) ;
#18584 = CARTESIAN_POINT ( 'NONE',  ( 799.4546378042377910, 14.92167643740321381, -356.1575198192848006 ) ) ;
#18585 = DIRECTION ( 'NONE',  ( 1.000000000000000000, 0.000000000000000000, 0.000000000000000000 ) ) ;
#18586 = FACE_OUTER_BOUND ( 'NONE', #22176, .T. ) ;
#18588 = CARTESIAN_POINT ( 'NONE',  ( 804.4286716492782716, -353.3618753856922012, 345.3141322388244703 ) ) ;
#18587 = CARTESIAN_POINT ( 'NONE',  ( 802.7791456095903868, -148.7146871989598935, 329.0155153010375102 ) ) ;
#18589 = ORIENTED_EDGE ( 'NONE', *, *, #36318, .T. ) ;
#18590 = CARTESIAN_POINT ( 'NONE',  ( 758.6633372737375112, -308.5328690171412518, -326.9102291470432533 ) ) ;
#18591 = CARTESIAN_POINT ( 'NONE',  ( 803.4237431249931660, -159.1800572038746111, 331.2633955100225194 ) ) ;
#18592 = CARTESIAN_POINT ( 'NONE',  ( 781.2497674668890113, -324.3510508353229511, -375.3608509340180603 ) ) ;
#18593 = DIRECTION ( 'NONE',  ( 0.000000000000000000, 0.000000000000000000, 1.000000000000000000 ) ) ;
#18594 = CARTESIAN_POINT ( 'NONE',  ( 812.6845335610512393, -439.9874144716862929, 353.5525998758768651 ) ) ;
#18595 = ORIENTED_EDGE ( 'NONE', *, *, #41940, .F. ) ;
#18596 = CARTESIAN_POINT ( 'NONE',  ( 785.3687786644884454, -323.3618753856923149, 315.3201227861279676 ) ) ;
#18597 = CARTESIAN_POINT ( 'NONE',  ( 756.1348686366196716, -89.26014174441463922, -347.5531968255698416 ) ) ;
#18598 = CARTESIAN_POINT ( 'NONE',  ( 785.3687786644884454, -443.3618753856917465, 315.3201227861279676 ) ) ;
#18599 = CARTESIAN_POINT ( 'NONE',  ( 767.7687537140311633, -143.9073299311473590, -372.7932403749916830 ) ) ;
#18600 = EDGE_LOOP ( 'NONE', ( #18212, #29989 ) ) ;
#18601 = CIRCLE ( 'NONE', #11247, 8.000000000000007105 ) ;
#18602 = CARTESIAN_POINT ( 'NONE',  ( 774.6858677611749044, -129.7255117493292289, -315.5713283507209894 ) ) ;
#18603 = ORIENTED_EDGE ( 'NONE', *, *, #42189, .T. ) ;
#18604 = CARTESIAN_POINT ( 'NONE',  ( 775.8780910478218402, -417.2817908451522158, -364.9511171171680530 ) ) ;
#18605 = CARTESIAN_POINT ( 'NONE',  ( 788.7366044899766848, 12.09267006885214180, 316.5762568750059813 ) ) ;
#18606 = CARTESIAN_POINT ( 'NONE',  ( 801.1904061080336987, -236.0891481129651766, 368.3070685750235498 ) ) ;
#18607 = CARTESIAN_POINT ( 'NONE',  ( 796.7845633553578182, -177.6237781080507148, 358.5707757039688204 ) ) ;
#18609 = CARTESIAN_POINT ( 'NONE',  ( 1238.921997096861332, 240.0000000000000853, -360.0000000000000000 ) ) ;
#18608 = CARTESIAN_POINT ( 'NONE',  ( 786.4999999999993179, -513.1383975375929367, -369.9999999999999432 ) ) ;
#18610 = ORIENTED_EDGE ( 'NONE', *, *, #39960, .T. ) ;
#18611 = CARTESIAN_POINT ( 'NONE',  ( 766.0291762391763086, -394.9181544815158418, -360.7704444035551319 ) ) ;
#18612 = DIRECTION ( 'NONE',  ( 0.000000000000000000, 0.000000000000000000, 1.000000000000000000 ) ) ;
#18613 = CARTESIAN_POINT ( 'NONE',  ( 814.2805881961230625, -217.6454272087891582, -331.2368401574024119 ) ) ;
#18614 = CARTESIAN_POINT ( 'NONE',  ( 749.5768839229115201, -60.55451811788051941, 358.0661480581553064 ) ) ;
#18616 = FACE_BOUND ( 'NONE', #25798, .T. ) ;
#18615 = DIRECTION ( 'NONE',  ( -0.000000000000000000, -0.000000000000000000, 1.000000000000000000 ) ) ;
#18617 = CARTESIAN_POINT ( 'NONE',  ( 754.8983024940795303, -330.8965053807774552, -336.9254006560228163 ) ) ;
#18618 = DIRECTION ( 'NONE',  ( 0.000000000000000000, -1.000000000000000000, 0.000000000000000000 ) ) ;
#18619 = CARTESIAN_POINT ( 'NONE',  ( 793.5525998758768083, -199.0999726633346825, -372.6845335610516941 ) ) ;
#18620 = DIRECTION ( 'NONE',  ( 1.000000000000000000, -1.880165489482579047E-16, 0.000000000000000000 ) ) ;
#18621 = PLANE ( 'NONE',  #37829 ) ;
#18622 = CARTESIAN_POINT ( 'NONE',  ( 801.5560724626406000, -384.5545181178795247, 326.7756240680316182 ) ) ;
#18623 = AXIS2_PLACEMENT_3D ( 'NONE', #26324, #19173, #39765 ) ;
#18624 = CARTESIAN_POINT ( 'NONE',  ( 767.7687537140311633, -239.9073299311470748, -372.7932403749916830 ) ) ;
#18625 = DIRECTION ( 'NONE',  ( -0.000000000000000000, 1.000000000000000000, -0.000000000000000000 ) ) ;
#18626 = CARTESIAN_POINT ( 'NONE',  ( 788.8264449731200330, -21.18005720387502677, -363.6646147819171233 ) ) ;
#18627 = CARTESIAN_POINT ( 'NONE',  ( 755.8990559732751535, -179.4636090269710849, 365.9055244015606831 ) ) ;
#18628 = CARTESIAN_POINT ( 'NONE',  ( 771.2368401574024119, -109.4419599262327836, -374.2805881961240857 ) ) ;
#18629 = CARTESIAN_POINT ( 'NONE',  ( 804.7487373415286811, -115.5436935675110988, 364.7487373415288516 ) ) ;
#18630 = CARTESIAN_POINT ( 'NONE',  ( 792.2312462859673587, -371.9073299311465917, -307.2067596250082602 ) ) ;
#18631 = DIRECTION ( 'NONE',  ( 0.000000000000000000, -0.6755902076156505842, -0.7372773368101328550 ) ) ;
#18632 = DIRECTION ( 'NONE',  ( 0.000000000000000000, -0.9238795325112892920, 0.3826834323650836756 ) ) ;
#18633 = CARTESIAN_POINT ( 'NONE',  ( 800.0135310231082713, -230.0891481129652618, 325.0180583372163028 ) ) ;
#18634 = VECTOR ( 'NONE', #555, 1000.000000000000000 ) ;
#18635 = CARTESIAN_POINT ( 'NONE',  ( 802.2119215644370342, -462.0090635724247932, 367.5423716828165084 ) ) ;
#18636 = CARTESIAN_POINT ( 'NONE',  ( 745.1769319972822814, -401.8055962898681059, -346.2694204179732083 ) ) ;
#18637 = CARTESIAN_POINT ( 'NONE',  ( 804.1009440267234822, 0.5363909730283709099, -314.0944755984392600 ) ) ;
#18638 = DIRECTION ( 'NONE',  ( -0.000000000000000000, -0.000000000000000000, 1.000000000000000000 ) ) ;
#18639 = CARTESIAN_POINT ( 'NONE',  ( 766.5853460496234675, -13.98741447168760033, 372.3518521366060554 ) ) ;
#18640 = CARTESIAN_POINT ( 'NONE',  ( 805.0264073115434940, -198.3510508353234059, -339.4763451958999099 ) ) ;
#18641 = CARTESIAN_POINT ( 'NONE',  ( 797.6776695296629214, -19.54369356751139364, 357.6776695296636603 ) ) ;
#18642 = CARTESIAN_POINT ( 'NONE',  ( 814.8230680027162407, -221.8055962898687881, -333.7305795820267917 ) ) ;
#18643 = CARTESIAN_POINT ( 'NONE',  ( 805.9055244015594326, -339.6237781080502600, 315.8990559732753240 ) ) ;
#18644 = CARTESIAN_POINT ( 'NONE',  ( 791.9812246680005501, -164.6346026584200217, 361.9419747391813189 ) ) ;
#18645 = ORIENTED_EDGE ( 'NONE', *, *, #13155, .F. ) ;
#18646 = CARTESIAN_POINT ( 'NONE',  ( 746.0683387631852383, -427.4419599262317888, 331.3260364891676204 ) ) ;
#18647 = CARTESIAN_POINT ( 'NONE',  ( 778.1981804954714335, -154.2709662947836478, -314.8072714833589885 ) ) ;
#18648 = CARTESIAN_POINT ( 'NONE',  ( 757.8323909638827445, -338.6346026584195101, 352.1044303154654358 ) ) ;
#18649 = CARTESIAN_POINT ( 'NONE',  ( 763.2262854647970016, -56.63460265842036279, -309.2812353651462445 ) ) ;
#18650 = AXIS2_PLACEMENT_3D ( 'NONE', #24905, #38543, #35522 ) ;
#18651 = VERTEX_POINT ( 'NONE', #32940 ) ;
#18652 = CARTESIAN_POINT ( 'NONE',  ( 814.2805881961230625, -457.6454272087884760, -331.2368401574024119 ) ) ;
#18653 = EDGE_LOOP ( 'NONE', ( #5971, #4007, #6005, #38819 ) ) ;
#18654 = CARTESIAN_POINT ( 'NONE',  ( 769.0155153010367712, -322.3726999360615082, -362.7791456095907279 ) ) ;
#18656 = CARTESIAN_POINT ( 'NONE',  ( 780.5236548040995785, -380.7363362996977116, 314.9735926884559944 ) ) ;
#18655 = CARTESIAN_POINT ( 'NONE',  ( 805.1927285166397041, -64.81642084023852135, 341.8018195045277707 ) ) ;
#18657 = CARTESIAN_POINT ( 'NONE',  ( 805.1927285166397041, -304.8164208402376403, -341.8018195045277707 ) ) ;
#18659 = CARTESIAN_POINT ( 'NONE',  ( 798.0661480581538854, -290.5328690171412518, 309.5768839229118043 ) ) ;
#18658 = CARTESIAN_POINT ( 'NONE',  ( 754.9967657858570647, -385.5436935675102745, 365.0032342141425943 ) ) ;
#18660 = CARTESIAN_POINT ( 'NONE',  ( 804.1105419155481968, -291.8272453906071746, -347.6308680596136469 ) ) ;
#18661 = CARTESIAN_POINT ( 'NONE',  ( 794.9819416627830151, -276.9982390220559978, -319.9864689768909898 ) ) ;
#18662 = FACE_OUTER_BOUND ( 'NONE', #15032, .T. ) ;
#18663 = CARTESIAN_POINT ( 'NONE',  ( 767.8955696845333705, -168.4527844766018347, -362.1676090361162323 ) ) ;
#18664 = EDGE_CURVE ( 'NONE', #27191, #35548, #30722, .T. ) ;
#18665 = DIRECTION ( 'NONE',  ( 0.000000000000000000, 0.000000000000000000, 1.000000000000000000 ) ) ;
#18666 = ORIENTED_EDGE ( 'NONE', *, *, #39030, .F. ) ;
#18667 = CARTESIAN_POINT ( 'NONE',  ( 777.4774526936600978, -418.2709662947827383, 304.7301800767027657 ) ) ;
#18669 = DIRECTION ( 'NONE',  ( -1.000000000000000000, 0.000000000000000000, 0.000000000000000000 ) ) ;
#18668 = FACE_OUTER_BOUND ( 'NONE', #44898, .T. ) ;
#18670 = CARTESIAN_POINT ( 'NONE',  ( 814.8207195650702488, -98.19088175424404596, -336.2433038121456548 ) ) ;
#18671 = FACE_OUTER_BOUND ( 'NONE', #3243, .T. ) ;
#18672 = DIRECTION ( 'NONE',  ( 0.000000000000000000, 0.000000000000000000, 1.000000000000000000 ) ) ;
#18673 = CARTESIAN_POINT ( 'NONE',  ( 775.8780910478218402, -297.2817908451526137, 364.9511171171680530 ) ) ;
#18674 = CARTESIAN_POINT ( 'NONE',  ( 778.1981804954714335, -154.2709662947836478, 314.8072714833589885 ) ) ;
#18675 = ORIENTED_EDGE ( 'NONE', *, *, #7399, .F. ) ;
#18676 = CARTESIAN_POINT ( 'NONE',  ( 754.9967657858570647, -121.5436935675110561, -365.0032342141425943 ) ) ;
#18677 = CARTESIAN_POINT ( 'NONE',  ( 772.3691319403857278, -335.2601417444137724, 315.8894580844506663 ) ) ;
#18678 = CARTESIAN_POINT ( 'NONE',  ( 949.5497976682736407, 239.9999999999998863, -2132.806278688367456 ) ) ;
#18679 = CARTESIAN_POINT ( 'NONE',  ( 778.7629533639073998, -80.73633629969864955, 375.0009284576466371 ) ) ;
#18680 = CARTESIAN_POINT ( 'NONE',  ( 804.7487373415286811, -259.5436935675106156, -364.7487373415288516 ) ) ;
#18681 = EDGE_CURVE ( 'NONE', #3140, #25461, #24714, .T. ) ;
#18682 = CARTESIAN_POINT ( 'NONE',  ( 755.3201227861273992, -99.72551174932928575, 345.3687786644892981 ) ) ;
#18683 = CIRCLE ( 'NONE', #17928, 2.749999999999919176 ) ;
#18684 = CARTESIAN_POINT ( 'NONE',  ( -39.63011601220123481, -110.5936016518799221, 750.6326042729449455 ) ) ;
#18685 = CARTESIAN_POINT ( 'NONE',  ( 761.9338519418445230, -302.5328690171411949, -370.4231160770881957 ) ) ;
#18686 = AXIS2_PLACEMENT_3D ( 'NONE', #41151, #33970, #23566 ) ;
#18687 = CARTESIAN_POINT ( 'NONE',  ( 804.8461984189677878, -26.19088175424427334, 336.9566956441385628 ) ) ;
#18688 = CARTESIAN_POINT ( 'NONE',  ( 745.7998596910086917, -341.3618753856922012, -332.5602148656461168 ) ) ;
#18689 = DIRECTION ( 'NONE',  ( -1.000000000000000000, -0.000000000000000000, 0.000000000000000000 ) ) ;
#18690 = CARTESIAN_POINT ( 'NONE',  ( 783.0433043558608688, -408.8965053807772847, 315.1538015810313027 ) ) ;
#18691 = ORIENTED_EDGE ( 'NONE', *, *, #13335, .T. ) ;
#18692 = CARTESIAN_POINT ( 'NONE',  ( 778.2165204200184689, -430.8164208402374129, -364.9363028652563230 ) ) ;
#18693 = CARTESIAN_POINT ( 'NONE',  ( 749.8865473780648472, -92.53286901714190549, -322.1177392798429082 ) ) ;
#18694 = CARTESIAN_POINT ( 'NONE',  ( 1238.921997096861332, 430.0000000000002842, -320.0000000000000568 ) ) ;
#18695 = CARTESIAN_POINT ( 'NONE',  ( 746.0683387631852383, -235.4419599262323857, 331.3260364891676204 ) ) ;
#18696 = CARTESIAN_POINT ( 'NONE',  ( 756.5762568750052424, -51.18005720387493085, 348.7366044899774238 ) ) ;
#18697 = COLOUR_RGB ( '',0.7921568627450980005, 0.8196078431372548767, 0.9333333333333333481 ) ;
#18698 = CARTESIAN_POINT ( 'NONE',  ( 789.9200121543843807, -241.9874144716869182, -317.0176451133914384 ) ) ;
#18699 = CARTESIAN_POINT ( 'NONE',  ( 802.1676090361156639, -230.6346026584197659, 327.8955696845344505 ) ) ;
#18700 = CARTESIAN_POINT ( 'NONE',  ( 812.6845335610512393, -79.98741447168740137, -353.5525998758768651 ) ) ;
#18701 = CARTESIAN_POINT ( 'NONE',  ( 809.1994704715707485, -452.9681489794448908, -335.3884333643831042 ) ) ;
#18702 = EDGE_LOOP ( 'NONE', ( #33191, #42397, #27669, #25001, #24832, #43356 ) ) ;
#18703 = CARTESIAN_POINT ( 'NONE',  ( 760.5453621957607311, -69.07832356259653750, 323.8424801807151425 ) ) ;
#18704 = CARTESIAN_POINT ( 'NONE',  ( 807.2620300519052989, -336.0090635724251911, -318.0141637701419768 ) ) ;
#18705 = EDGE_CURVE ( 'NONE', #23565, #29447, #25450, .T. ) ;
#18706 = CARTESIAN_POINT ( 'NONE',  ( 810.7187646348534145, -282.4527844766014937, 356.7737145352016341 ) ) ;
#18707 = CARTESIAN_POINT ( 'NONE',  ( 768.8385539511368734, -23.26014174441484883, 306.4236121716840557 ) ) ;
#18708 = CARTESIAN_POINT ( 'NONE',  ( 801.5560724626406000, -168.5545181178802352, -326.7756240680316182 ) ) ;
#18709 = CARTESIAN_POINT ( 'NONE',  ( 794.9819416627830151, -180.9982390220563389, -319.9864689768909898 ) ) ;
#18710 = AXIS2_PLACEMENT_3D ( 'NONE', #12422, #34103, #29971 ) ;
#18711 = CARTESIAN_POINT ( 'NONE',  ( 804.9363028652555840, -376.2709662947829656, -338.2165204200192079 ) ) ;
#18712 = EDGE_CURVE ( 'NONE', #36831, #14331, #8008, .T. ) ;
#18713 = ORIENTED_EDGE ( 'NONE', *, *, #25160, .T. ) ;
#18714 = AXIS2_PLACEMENT_3D ( 'NONE', #41792, #6453, #31147 ) ;
#18715 = CARTESIAN_POINT ( 'NONE',  ( 796.7845633553578182, 14.37622189194867417, -358.5707757039688204 ) ) ;
#18716 = EDGE_LOOP ( 'NONE', ( #26077, #21774, #44804, #6999, #539 ) ) ;
#18717 = CARTESIAN_POINT ( 'NONE',  ( 808.3070685750230950, -306.9982390220558273, 361.1904061080339261 ) ) ;
#18718 = DIRECTION ( 'NONE',  ( -0.000000000000000000, -0.000000000000000000, 1.000000000000000000 ) ) ;
#18719 = CARTESIAN_POINT ( 'NONE',  ( 802.5472867521000353, -220.3726999360618208, 350.8726784830461156 ) ) ;
#18720 = CARTESIAN_POINT ( 'NONE',  ( 804.9511171171677688, -365.8055962898682765, 335.8780910478229202 ) ) ;
#18721 = CARTESIAN_POINT ( 'NONE',  ( 1007.605605532488426, -32.84703287382739489, 757.2634078669104838 ) ) ;
#18722 = CARTESIAN_POINT ( 'NONE',  ( 769.0155153010367712, -178.3726999360619629, 362.7791456095907279 ) ) ;
#18723 = CARTESIAN_POINT ( 'NONE',  ( 804.9363028652555840, -64.27096629478397460, 338.2165204200192079 ) ) ;
#18724 = EDGE_LOOP ( 'NONE', ( #8540, #8368, #25902, #18106 ) ) ;
#18725 = CARTESIAN_POINT ( 'NONE',  ( 760.0363995740630116, -418.9181544815157849, -368.7758568127991907 ) ) ;
#18726 = CARTESIAN_POINT ( 'NONE',  ( 751.6929314249750860, -6.998239022056886860, -318.8095938919659034 ) ) ;
#18727 = CARTESIAN_POINT ( 'NONE',  ( 744.6391490659812007, -254.7363362996981095, 338.7502325331110455 ) ) ;
#18728 = CARTESIAN_POINT ( 'NONE',  ( 766.7756240680305382, -206.5328690171415360, 361.5560724626415663 ) ) ;
#18729 = CARTESIAN_POINT ( 'NONE',  ( 797.6776695296629214, -403.5436935675101608, -357.6776695296636603 ) ) ;
#18730 = CARTESIAN_POINT ( 'NONE',  ( 792.1044303154646968, 11.54721552339759860, -317.8323909638837677 ) ) ;
#18731 = VECTOR ( 'NONE', #18111, 1000.000000000000000 ) ;
#18732 = EDGE_CURVE ( 'NONE', #11266, #31293, #829, .T. ) ;
#18733 = CARTESIAN_POINT ( 'NONE',  ( 768.0187753319979720, 15.36539734157940629, 318.0580252608186242 ) ) ;
#18734 = FILL_AREA_STYLE ('',( #4636 ) ) ;
#18735 = CARTESIAN_POINT ( 'NONE',  ( 763.0428371773158460, -251.4636090269709143, -358.7617431975195359 ) ) ;
#18736 = CARTESIAN_POINT ( 'NONE',  ( 772.5602148656447525, -57.72551174932945628, 305.7998596910095443 ) ) ;
#18737 = CARTESIAN_POINT ( 'NONE',  ( 772.5602148656447525, -105.7255117493293000, 305.7998596910095443 ) ) ;
#18738 = CYLINDRICAL_SURFACE ( 'NONE', #7781, 20.00000000000004974 ) ;
#18739 = DIRECTION ( 'NONE',  ( 1.000000000000000000, 0.000000000000000000, 0.000000000000000000 ) ) ;
#18740 = CARTESIAN_POINT ( 'NONE',  ( 748.6759233522253680, -400.3726999360612808, 324.3348316497537098 ) ) ;
#18741 = DIRECTION ( 'NONE',  ( 1.000000000000000000, 0.000000000000000000, 0.000000000000000000 ) ) ;
#18742 = CARTESIAN_POINT ( 'NONE',  ( 810.7187646348534145, -378.4527844766011526, 356.7737145352016341 ) ) ;
#18743 = CARTESIAN_POINT ( 'NONE',  ( 804.6798772138708955, -303.7255117493287457, -334.6312213355107019 ) ) ;
#18744 = CARTESIAN_POINT ( 'NONE',  ( 788.8264449731200330, -429.1800572038737869, 363.6646147819171233 ) ) ;
#18745 = VECTOR ( 'NONE', #32711, 1000.000000000000000 ) ;
#18746=STYLED_ITEM('',(#45758),#1418);
#18747 = CARTESIAN_POINT ( 'NONE',  ( 766.0291762391763086, -178.9181544815165239, 360.7704444035551319 ) ) ;
#18748 = CARTESIAN_POINT ( 'NONE',  ( 778.7629533639073998, -80.73633629969864955, -375.0009284576466371 ) ) ;
#18749 = CARTESIAN_POINT ( 'NONE',  ( 794.1144889064781864, -130.1692326535054463, -360.9840315886528401 ) ) ;
#18750 = CARTESIAN_POINT ( 'NONE',  ( 813.9316612368132837, -127.4419599262326983, 348.6739635108323228 ) ) ;
#18751 = CARTESIAN_POINT ( 'NONE',  ( 792.1044303154646968, -444.4527844766009821, 317.8323909638837677 ) ) ;
#18752 = EDGE_CURVE ( 'NONE', #26579, #28289, #22746, .T. ) ;
#18753 = CARTESIAN_POINT ( 'NONE',  ( 800.0135310231082713, -38.08914811296587999, -325.0180583372163028 ) ) ;
#18754 = CARTESIAN_POINT ( 'NONE',  ( 786.6156483768007774, -145.4419599262326699, -315.5913626894246136 ) ) ;
#18755 = CARTESIAN_POINT ( 'NONE',  ( 771.2633955100217236, -119.9073299311474443, -363.4237431249939618 ) ) ;
#18756 = EDGE_CURVE ( 'NONE', #14400, #29759, #32075, .T. ) ;
#18757 = CARTESIAN_POINT ( 'NONE',  ( 803.2186876482843445, -439.9874144716862929, -350.0220218866286928 ) ) ;
#18759 = CARTESIAN_POINT ( 'NONE',  ( 755.0636971347428243, -244.2709662947834204, 341.7834795799807353 ) ) ;
#18758 = CARTESIAN_POINT ( 'NONE',  ( 788.7366044899766848, -251.9073299311470748, 316.5762568750059813 ) ) ;
#18760 = DIRECTION ( 'NONE',  ( -0.000000000000000000, -6.938893903907241197E-16, 1.000000000000000000 ) ) ;
#18761 = ORIENTED_EDGE ( 'NONE', *, *, #14605, .F. ) ;
#18762 = CARTESIAN_POINT ( 'NONE',  ( 801.9419747391806368, -450.4527844766009821, 351.9812246680014027 ) ) ;
#18763 = AXIS2_PLACEMENT_3D ( 'NONE', #21932, #32082, #11540 ) ;
#18764 = EDGE_LOOP ( 'NONE', ( #7456, #25575 ) ) ;
#18765 = ADVANCED_FACE ( 'NONE', ( #21846 ), #1286, .F. ) ;
#18766 = EDGE_CURVE ( 'NONE', #17174, #4341, #29464, .T. ) ;
#18767 = AXIS2_PLACEMENT_3D ( 'NONE', #33843, #41461, #30370 ) ;
#18768 = CARTESIAN_POINT ( 'NONE',  ( 814.9108240113580450, -184.2709662947835909, 337.5031285880265273 ) ) ;
#18769 = CARTESIAN_POINT ( 'NONE',  ( 802.9823548866075953, -265.0999726633344267, 330.0799878456151077 ) ) ;
#18770 = EDGE_LOOP ( 'NONE', ( #18458, #44718, #37144, #20040 ) ) ;
#18771 = CARTESIAN_POINT ( 'NONE',  ( 776.9254006560222479, -92.19088175424406018, -314.8983024940802125 ) ) ;
#18772 = CARTESIAN_POINT ( 'NONE',  ( 751.2241431872005251, -208.1692326535051905, 359.9636004259367610 ) ) ;
#18773 = CARTESIAN_POINT ( 'NONE',  ( 765.0180583372156207, -264.9982390220561115, -360.0135310231089534 ) ) ;
#18774 = ORIENTED_EDGE ( 'NONE', *, *, #12744, .T. ) ;
#18775 = CARTESIAN_POINT ( 'NONE',  ( 801.9419747391806368, -378.4527844766011526, -351.9812246680014027 ) ) ;
#18776 = CARTESIAN_POINT ( 'NONE',  ( 804.9363028652555840, -64.27096629478397460, -338.2165204200192079 ) ) ;
#18777 = CARTESIAN_POINT ( 'NONE',  ( 775.9200461376533440, -263.8055962898686175, 315.3028492785443291 ) ) ;
#18778 = LINE ( 'NONE', #5133, #4187 ) ;
#18779 = DIRECTION ( 'NONE',  ( -0.000000000000000000, 0.000000000000000000, -1.000000000000000000 ) ) ;
#18780 = CARTESIAN_POINT ( 'NONE',  ( 809.0717654672305343, -4.918154481517067467, -360.1688906516309885 ) ) ;
#18781 = PLANE ( 'NONE',  #5576 ) ;
#18782 = EDGE_LOOP ( 'NONE', ( #16333, #39535 ) ) ;
#18783 = CARTESIAN_POINT ( 'NONE',  ( 797.8822607201568644, -318.5545181178796952, -370.1134526219340160 ) ) ;
#18784 = AXIS2_PLACEMENT_3D ( 'NONE', #9300, #33995, #12748 ) ;
#18785 = EDGE_CURVE ( 'NONE', #37618, #15749, #15148, .T. ) ;
#18786 = CARTESIAN_POINT ( 'NONE',  ( 791.0478386215596629, -165.8272453906074873, 306.7653713866226326 ) ) ;
#18788 = CARTESIAN_POINT ( 'NONE',  ( 794.9819416627830151, -252.9982390220560831, -319.9864689768909898 ) ) ;
#18787 = FACE_OUTER_BOUND ( 'NONE', #6760, .T. ) ;
#18789 = ADVANCED_FACE ( 'NONE', ( #25543 ), #19071, .F. ) ;
#18790 = CARTESIAN_POINT ( 'NONE',  ( 311.1634899080286232, 229.9999999999999716, -197.2499999999964473 ) ) ;
#18791 = CARTESIAN_POINT ( 'NONE',  ( 757.0176451133909268, -157.0999726633347962, -349.9200121543848354 ) ) ;
#18792 = CARTESIAN_POINT ( 'NONE',  ( 782.4968714119720516, -10.81642084023869543, 305.0891759886411023 ) ) ;
#18793 = DIRECTION ( 'NONE',  ( 1.000000000000000000, 0.000000000000000000, 0.000000000000000000 ) ) ;
#18795 = CIRCLE ( 'NONE', #21745, 2.749999999999835687 ) ;
#18794 = CARTESIAN_POINT ( 'NONE',  ( 745.4481719005789273, -339.7255117493285184, -347.5162901302853697 ) ) ;
#18796 = CARTESIAN_POINT ( 'NONE',  ( 181.1634899080285948, 260.0000000000000000, -199.9999999999953957 ) ) ;
#18797 = CARTESIAN_POINT ( 'NONE',  ( 802.1676090361156639, -62.63460265842031305, 327.8955696845344505 ) ) ;
#18798 = CONICAL_SURFACE ( 'NONE', #28374, 8.025000000000003908, 0.7853981633974446153 ) ;
#18799 = CARTESIAN_POINT ( 'NONE',  ( 802.2119215644370342, -294.0090635724253048, 367.5423716828165084 ) ) ;
#18800 = CARTESIAN_POINT ( 'NONE',  ( 773.7943932421234194, -239.8055962898687028, -305.5313806188329409 ) ) ;
#18801 = CARTESIAN_POINT ( 'NONE',  ( 812.7932403749906598, -255.1800572038742700, 327.7687537140311633 ) ) ;
#18802 = CARTESIAN_POINT ( 'NONE',  ( 814.5518280994195948, 8.274488250670337663, -332.4837098697145734 ) ) ;
#18803 = CARTESIAN_POINT ( 'NONE',  ( 998.9999999999992042, 479.9999999999999432, -360.0000000000000000 ) ) ;
#18804 = AXIS2_PLACEMENT_3D ( 'NONE', #35654, #7040, #38682 ) ;
#18805 = ORIENTED_EDGE ( 'NONE', *, *, #1836, .T. ) ;
#18806 = CARTESIAN_POINT ( 'NONE',  ( 804.4286716492782716, -329.3618753856922581, 345.3141322388244703 ) ) ;
#18807 = ADVANCED_FACE ( 'NONE', ( #40541 ), #26214, .F. ) ;
#18808 = CARTESIAN_POINT ( 'NONE',  ( 784.1219089521767955, -93.28179084515315367, 315.0488828828318333 ) ) ;
#18809 = CARTESIAN_POINT ( 'NONE',  ( 769.1273215169530886, 1.285312801039623753, -317.4527132478988847 ) ) ;
#18810 = CARTESIAN_POINT ( 'NONE',  ( -338.8365100919713200, 258.0940000000001078, -206.1189999999917859 ) ) ;
#18811 = EDGE_CURVE ( 'NONE', #15704, #32527, #15814, .T. ) ;
#18812 = CARTESIAN_POINT ( 'NONE',  ( -468.8365100919714337, 260.0000000000001705, -191.9749999999908709 ) ) ;
#18814 = CARTESIAN_POINT ( 'NONE',  ( 771.2633955100217236, -383.9073299311466485, 363.4237431249939618 ) ) ;
#18813 = CARTESIAN_POINT ( 'NONE',  ( 787.6308680596127942, -155.2601417444144261, 364.1105419155492768 ) ) ;
#18815 = ORIENTED_EDGE ( 'NONE', *, *, #37974, .T. ) ;
#18816 = ADVANCED_FACE ( 'NONE', ( #1051 ), #18076, .F. ) ;
#18817 = CARTESIAN_POINT ( 'NONE',  ( 796.7845633553578182, -321.6237781080502600, -358.5707757039688204 ) ) ;
#18818 = CARTESIAN_POINT ( 'NONE',  ( 804.4286716492782716, -161.3618753856927697, 345.3141322388244703 ) ) ;
#18819 = COLOUR_RGB ( '',0.7921568627450980005, 0.8196078431372548767, 0.9333333333333333481 ) ;
#18820 = CARTESIAN_POINT ( 'NONE',  ( 745.1769319972822814, -329.8055962898683902, -346.2694204179732083 ) ) ;
#18821 = DIRECTION ( 'NONE',  ( -1.000000000000000000, -0.000000000000000000, 0.000000000000000000 ) ) ;
#18822 = CARTESIAN_POINT ( 'NONE',  ( 772.5602148656447525, 14.27448825067031812, 305.7998596910095443 ) ) ;
#18823 = ORIENTED_EDGE ( 'NONE', *, *, #38798, .T. ) ;
#18824 = CARTESIAN_POINT ( 'NONE',  ( 802.1676090361156639, -350.6346026584192828, 327.8955696845344505 ) ) ;
#18825 = AXIS2_PLACEMENT_3D ( 'NONE', #942, #29371, #28441 ) ;
#18826 = CARTESIAN_POINT ( 'NONE',  ( 799.4546378042377910, -81.07832356259649487, -356.1575198192848006 ) ) ;
#18827 = ORIENTED_EDGE ( 'NONE', *, *, #36789, .F. ) ;
#18828 = CARTESIAN_POINT ( 'NONE',  ( 804.9363028652555840, -448.2709662947827951, 338.2165204200192079 ) ) ;
#18829 = CARTESIAN_POINT ( 'NONE',  ( 755.2512626584698410, -175.5436935675108998, -315.2512626584710915 ) ) ;
#18830 = ORIENTED_EDGE ( 'NONE', *, *, #41132, .F. ) ;
#18831 = CARTESIAN_POINT ( 'NONE',  ( 762.3223304703356007, -175.5436935675108998, -322.3223304703362828 ) ) ;
#18832 = ORIENTED_EDGE ( 'NONE', *, *, #24955, .T. ) ;
#18833 = CARTESIAN_POINT ( 'NONE',  ( 796.9571628226829034, -431.4636090269702322, -321.2382568024804641 ) ) ;
#18834 = CIRCLE ( 'NONE', #3368, 10.00000000000000888 ) ;
#18835 = CARTESIAN_POINT ( 'NONE',  ( 802.5472867521000353, -460.3726999360611103, 350.8726784830461156 ) ) ;
#18836 = CARTESIAN_POINT ( 'NONE',  ( 795.9930595647434757, -147.0783235625962959, 320.7433823573372820 ) ) ;
#18839 = CARTESIAN_POINT ( 'NONE',  ( 812.6845335610512393, -415.9874144716862361, 353.5525998758768651 ) ) ;
#18838 = LINE ( 'NONE', #136, #3391 ) ;
#18837 = DIRECTION ( 'NONE',  ( 0.000000000000000000, 0.000000000000000000, 1.000000000000000000 ) ) ;
#18840 = AXIS2_PLACEMENT_3D ( 'NONE', #44179, #5371, #5160 ) ;
#18841 = VECTOR ( 'NONE', #31210, 1000.000000000000000 ) ;
#18842 = ORIENTED_EDGE ( 'NONE', *, *, #19601, .F. ) ;
#18843 = CARTESIAN_POINT ( 'NONE',  ( 766.9102291470427417, -426.5545181178794678, -318.6633372737382501 ) ) ;
#18844 = DIRECTION ( 'NONE',  ( 1.000000000000000000, 0.000000000000000000, 0.000000000000000000 ) ) ;
#18845 = CARTESIAN_POINT ( 'NONE',  ( 750.9282345327678740, -208.9181544815164102, -319.8311093483690115 ) ) ;
#18846 = CARTESIAN_POINT ( 'NONE',  ( 812.3518521366052028, -73.09997266333502353, 326.5853460496235243 ) ) ;
#18848 = LINE ( 'NONE', #11457, #45464 ) ;
#18847 = DIRECTION ( 'NONE',  ( 1.000000000000000000, 0.000000000000000000, 0.000000000000000000 ) ) ;
#18849 = CARTESIAN_POINT ( 'NONE',  ( 801.3366627262608972, -320.5328690171411949, -353.0897708529566899 ) ) ;
#18850 = DIRECTION ( 'NONE',  ( 0.000000000000000000, -0.3826834323650836756, -0.9238795325112892920 ) ) ;
#18851 = CARTESIAN_POINT ( 'NONE',  ( 797.8822607201568644, -198.5545181178800647, -370.1134526219340160 ) ) ;
#18852 = LINE ( 'NONE', #33161, #42949 ) ;
#18853 = DIRECTION ( 'NONE',  ( 0.000000000000000000, 0.000000000000000000, -1.000000000000000000 ) ) ;
#18854 = CARTESIAN_POINT ( 'NONE',  ( 757.0176451133909268, -397.0999726633340288, 349.9200121543848354 ) ) ;
#18855 = AXIS2_PLACEMENT_3D ( 'NONE', #22121, #29303, #4134 ) ;
#18856 = CARTESIAN_POINT ( 'NONE',  ( 751.9810565676468741, -242.0891481129652618, -360.9747183278973921 ) ) ;
#18857 = FACE_OUTER_BOUND ( 'NONE', #10569, .T. ) ;
#18858 = CARTESIAN_POINT ( 'NONE',  ( 774.6858677611749044, -9.725511749329603717, -315.5713283507209894 ) ) ;
#18859 = AXIS2_PLACEMENT_3D ( 'NONE', #31315, #20473, #9844 ) ;
#18860 = CARTESIAN_POINT ( 'NONE',  ( 815.3608509340175488, -170.7363362996983938, 341.2497674668889545 ) ) ;
#18861 = CARTESIAN_POINT ( 'NONE',  ( 795.6651683502461765, -130.7146871989599504, -371.3240766477733814 ) ) ;
#18862 = CARTESIAN_POINT ( 'NONE',  ( 777.5031285880264704, -118.8164208402383508, 374.9108240113588408 ) ) ;
#18863 = CARTESIAN_POINT ( 'NONE',  ( 754.9967657858570647, -361.5436935675103882, -365.0032342141425374 ) ) ;
#18864 = CARTESIAN_POINT ( 'NONE',  ( 799.9999999999993179, -365.3551492539851893, -8.132432514707076621 ) ) ;
#18865 = DIRECTION ( 'NONE',  ( -0.000000000000000000, -0.000000000000000000, 1.000000000000000000 ) ) ;
#18866 = CARTESIAN_POINT ( 'NONE',  ( 795.1360043628807261, -236.0891481129651766, 360.2193346964456282 ) ) ;
#18867 = CARTESIAN_POINT ( 'NONE',  ( 757.0176451133909268, -37.09997266333514432, 349.9200121543848354 ) ) ;
#18868 = CARTESIAN_POINT ( 'NONE',  ( 800.2193346964447755, -402.9982390220555430, -355.1360043628815788 ) ) ;
#18869 = AXIS2_PLACEMENT_3D ( 'NONE', #14896, #22252, #42368 ) ;
#18870 = CARTESIAN_POINT ( 'NONE',  ( 781.2370466360911223, 3.263663700301089765, -304.9990715423533629 ) ) ;
#18871 = CARTESIAN_POINT ( 'NONE',  ( 879.9999999999992042, 529.9999999999997726, -244.9999999999999716 ) ) ;
#18872 = CARTESIAN_POINT ( 'NONE',  ( 761.9338519418445230, -38.53286901714206891, 370.4231160770881957 ) ) ;
#18873 = ORIENTED_EDGE ( 'NONE', *, *, #27521, .F. ) ;
#18874 = AXIS2_PLACEMENT_3D ( 'NONE', #41433, #34254, #9785 ) ;
#18875 = CARTESIAN_POINT ( 'NONE',  ( 789.9200121543843807, -193.9874144716870319, -317.0176451133914384 ) ) ;
#18876 = CARTESIAN_POINT ( 'NONE',  ( 801.9419747391806368, -18.45278447660230725, 351.9812246680014027 ) ) ;
#18877 = CARTESIAN_POINT ( 'NONE',  ( 747.3154664389472828, -235.9874144716868898, -326.4474001241230781 ) ) ;
#18878 = CARTESIAN_POINT ( 'NONE',  ( 919.9999999999993179, 154.9999999999998863, 360.0000000000000000 ) ) ;
#18879 = CARTESIAN_POINT ( 'NONE',  ( 773.7943932421234194, -359.8055962898683333, 305.5313806188329409 ) ) ;
#18880 = VERTEX_POINT ( 'NONE', #38599 ) ;
#18881 = CARTESIAN_POINT ( 'NONE',  ( 807.5423716828161105, -417.0783235625954148, 362.2119215644372048 ) ) ;
#18882 = CARTESIAN_POINT ( 'NONE',  ( 800.2193346964447755, -354.9982390220557704, 355.1360043628815788 ) ) ;
#18883 = CARTESIAN_POINT ( 'NONE',  ( 777.5031285880264704, -94.81642084023843609, -374.9108240113588408 ) ) ;
#18884 = CIRCLE ( 'NONE', #24766, 2.749999999999919176 ) ;
#18885 = ORIENTED_EDGE ( 'NONE', *, *, #35330, .T. ) ;
#18886 = CARTESIAN_POINT ( 'NONE',  ( 796.1575198192839480, -6.009063572426154742, -359.4546378042384163 ) ) ;
#18887 = VECTOR ( 'NONE', #25471, 1000.000000000000000 ) ;
#18888 = ORIENTED_EDGE ( 'NONE', *, *, #35964, .F. ) ;
#18889 = CARTESIAN_POINT ( 'NONE',  ( 779.4763451958990572, -320.7363362996979390, -365.0264073115438919 ) ) ;
#18891 = CARTESIAN_POINT ( 'NONE',  ( 775.8780910478218402, -369.2817908451523294, 364.9511171171680530 ) ) ;
#18890 = CARTESIAN_POINT ( 'NONE',  ( 756.5762568750052424, -51.18005720387493085, 348.7366044899774238 ) ) ;
#18892 = CARTESIAN_POINT ( 'NONE',  ( 774.6312213355099630, -335.3618753856920307, -364.6798772138717482 ) ) ;
#18893 = VECTOR ( 'NONE', #16493, 1000.000000000000000 ) ;
#18895 = CARTESIAN_POINT ( 'NONE',  ( 768.8385539511368734, -335.2601417444137724, 306.4236121716840557 ) ) ;
#18894 = CARTESIAN_POINT ( 'NONE',  ( 759.0252816721024374, -408.9982390220556567, 368.0189434323527280 ) ) ;
#18896 = CARTESIAN_POINT ( 'NONE',  ( 755.3028492785439312, -303.2817908451525000, -335.9200461376539693 ) ) ;
#18897 = CARTESIAN_POINT ( 'NONE',  ( 801.9419747391806368, -282.4527844766014937, -351.9812246680014027 ) ) ;
#18898 = DIRECTION ( 'NONE',  ( 0.000000000000000000, 0.6755902076156505842, 0.7372773368101327440 ) ) ;
#18899 = CARTESIAN_POINT ( 'NONE',  ( 759.7806653035534055, -150.9982390220563957, -324.8639956371180801 ) ) ;
#18900 = CYLINDRICAL_SURFACE ( 'NONE', #36546, 18.00000000000001421 ) ;
#18901 = CARTESIAN_POINT ( 'NONE',  ( 804.7487373415286811, -427.5436935675101040, 364.7487373415288516 ) ) ;
#18902 = CIRCLE ( 'NONE', #4168, 8.024999999999948841 ) ;
#18903 = SHAPE_REPRESENTATION ( 'Fixed Blade Support Base', ( #26858 ), #32022 ) ;
#18905 = LINE ( 'NONE', #8270, #26293 ) ;
#18904 = LINE ( 'NONE', #18229, #4911 ) ;
#18906 = CARTESIAN_POINT ( 'NONE',  ( 786.2694204179717872, -69.28179084515321051, -305.1769319972829067 ) ) ;
#18907 = DIRECTION ( 'NONE',  ( 0.000000000000000000, 0.000000000000000000, -1.000000000000000000 ) ) ;
#18908 = CARTESIAN_POINT ( 'NONE',  ( -208.8365100919714052, 240.0000000000000853, -199.9999999999926956 ) ) ;
#18909 = AXIS2_PLACEMENT_3D ( 'NONE', #15802, #37041, #18837 ) ;
#18910 = CARTESIAN_POINT ( 'NONE',  ( 755.8894580844503253, -279.8272453906071746, 332.3691319403863531 ) ) ;
#18911 = CARTESIAN_POINT ( 'NONE',  ( 762.3223304703356007, -151.5436935675109851, 322.3223304703362828 ) ) ;
#18912 = EDGE_LOOP ( 'NONE', ( #32560, #30008, #6024, #3299 ) ) ;
#18913 = CARTESIAN_POINT ( 'NONE',  ( 748.9653473494365699, -146.6346026584200786, -356.9462024416520762 ) ) ;
#18914 = CARTESIAN_POINT ( 'NONE',  ( 765.8855110935204493, -334.1692326535047073, 319.0159684113471599 ) ) ;
#18915 = DIRECTION ( 'NONE',  ( -0.000000000000000000, 1.000000000000000000, -0.000000000000000000 ) ) ;
#18916 = CARTESIAN_POINT ( 'NONE',  ( 746.4236121716829757, -63.82724539060779279, 328.8385539511384650 ) ) ;
#18917 = CARTESIAN_POINT ( 'NONE',  ( 755.2512626584698410, -271.5436935675106156, -315.2512626584710915 ) ) ;
#18918 = CARTESIAN_POINT ( 'NONE',  ( 782.4968714119720516, -202.8164208402380950, 305.0891759886411023 ) ) ;
#18919 = CARTESIAN_POINT ( 'NONE',  ( 794.9819416627830151, -108.9982390220565804, 319.9864689768909898 ) ) ;
#18920 = ORIENTED_EDGE ( 'NONE', *, *, #32349, .T. ) ;
#18921 = CARTESIAN_POINT ( 'NONE',  ( 813.9316612368132837, -319.4419599262320730, -348.6739635108323228 ) ) ;
#18922 = AXIS2_PLACEMENT_3D ( 'NONE', #33307, #29619, #8162 ) ;
#18923 = CARTESIAN_POINT ( 'NONE',  ( 804.1105419155481968, -3.827245390607979303, 347.6308680596136469 ) ) ;
#18924 = CARTESIAN_POINT ( 'NONE',  ( 754.9967657858570647, -361.5436935675103882, -365.0032342141425374 ) ) ;
#18925 = DIRECTION ( 'NONE',  ( -1.880165489482579047E-16, -1.000000000000000000, -0.000000000000000000 ) ) ;
#18926 = CARTESIAN_POINT ( 'NONE',  ( 805.1016975059191054, -390.8965053807772279, 343.0745993439771837 ) ) ;
#18927 = ORIENTED_EDGE ( 'NONE', *, *, #10609, .F. ) ;
#18929 = CIRCLE ( 'NONE', #9354, 10.00000000000000888 ) ;
#18928 = CARTESIAN_POINT ( 'NONE',  ( 801.9419747391806368, -426.4527844766010389, -351.9812246680014027 ) ) ;
#18930 = CARTESIAN_POINT ( 'NONE',  ( 778.2165204200184689, -214.8164208402380666, -364.9363028652563230 ) ) ;
#18931 = CARTESIAN_POINT ( 'NONE',  ( 800.1688906516307043, -130.1692326535054463, -369.0717654672308186 ) ) ;
#18932 = LINE ( 'NONE', #3533, #13755 ) ;
#18933 = CARTESIAN_POINT ( 'NONE',  ( 744.9990715423526808, -234.3510508353232638, 341.2370466360926002 ) ) ;
#18934 = CARTESIAN_POINT ( 'NONE',  ( 794.9819416627830151, -60.99823902205671544, 319.9864689768909898 ) ) ;
#18935 = CARTESIAN_POINT ( 'NONE',  ( 756.7813123517142913, -235.9874144716868898, -329.9779781133712504 ) ) ;
#18936 = CARTESIAN_POINT ( 'NONE',  ( 771.1735550268778070, -249.1800572038742416, 316.3353852180827630 ) ) ;
#18937 = AXIS2_PLACEMENT_3D ( 'NONE', #44098, #1819, #20063 ) ;
#18938 = CARTESIAN_POINT ( 'NONE',  ( 751.2241431872005251, -64.16923265350563099, -359.9636004259367610 ) ) ;
#18939 = CARTESIAN_POINT ( 'NONE',  ( 808.0106897970731552, -452.9681489794447771, -338.3625385368115985 ) ) ;
#18940 = ORIENTED_EDGE ( 'NONE', *, *, #23484, .F. ) ;
#18941 = VERTEX_POINT ( 'NONE', #31440 ) ;
#18942 = CARTESIAN_POINT ( 'NONE',  ( 749.5768839229115201, -348.5545181178796383, -358.0661480581553064 ) ) ;
#18943 = CARTESIAN_POINT ( 'NONE',  ( 792.2312462859673587, -275.9073299311469896, 307.2067596250082602 ) ) ;
#18944 = CARTESIAN_POINT ( 'NONE',  ( 747.3154664389472828, -19.98741447168758256, 326.4474001241230781 ) ) ;
#18945 = CARTESIAN_POINT ( 'NONE',  ( 793.0897708529556667, -198.5545181178800647, -361.3366627262616362 ) ) ;
#18946 = CARTESIAN_POINT ( 'NONE',  ( 771.1735550268778070, -177.1800572038744690, -316.3353852180827630 ) ) ;
#18947 = CARTESIAN_POINT ( 'NONE',  ( 785.3687786644885591, -395.3618753856919739, -315.3201227861280813 ) ) ;
#18948 = EDGE_LOOP ( 'NONE', ( #38962, #31483 ) ) ;
#18949 = ORIENTED_EDGE ( 'NONE', *, *, #23149, .T. ) ;
#18950 = AXIS2_PLACEMENT_3D ( 'NONE', #20983, #35079, #43391 ) ;
#18951 = CARTESIAN_POINT ( 'NONE',  ( 815.2698199232961542, -328.8164208402375834, 342.5225473063383106 ) ) ;
#18952 = CARTESIAN_POINT ( 'NONE',  ( 799.9999999999993179, -462.9681489794448339, 309.9999999999998863 ) ) ;
#18953 = CIRCLE ( 'NONE', #10844, 30.00000000000008171 ) ;
#18954 = CARTESIAN_POINT ( 'NONE',  ( 959.5497976682736407, 229.9999999999998579, 339.9999999999998863 ) ) ;
#18955 = CARTESIAN_POINT ( 'NONE',  ( 766.0291762391763086, -202.9181544815164386, 360.7704444035551319 ) ) ;
#18956 = CARTESIAN_POINT ( 'NONE',  ( 759.7806653035534055, -54.99823902205672255, 324.8639956371180801 ) ) ;
#18957 = VERTEX_POINT ( 'NONE', #26882 ) ;
#18958 = CARTESIAN_POINT ( 'NONE',  ( 776.2046728542105711, -404.1908817542431507, -304.8212110874238761 ) ) ;
#18959 = VECTOR ( 'NONE', #44745, 1000.000000000000000 ) ;
#18960 = CARTESIAN_POINT ( 'NONE',  ( 745.4481719005789273, -51.72551174932947049, -347.5162901302853697 ) ) ;
#18961 = CARTESIAN_POINT ( 'NONE',  ( 755.0488828828309806, -233.8055962898687028, 344.1219089521771934 ) ) ;
#18962 = AXIS2_PLACEMENT_3D ( 'NONE', #24487, #29116, #6950 ) ;
#18963 = CARTESIAN_POINT ( 'NONE',  ( 804.9363028652555840, -400.2709662947828519, -338.2165204200192079 ) ) ;
#18964 = CARTESIAN_POINT ( 'NONE',  ( 767.8955696845334842, -0.4527844766023629286, -362.1676090361161755 ) ) ;
#18965 = CARTESIAN_POINT ( 'NONE',  ( 812.7932403749906598, -447.1800572038736732, 327.7687537140311633 ) ) ;
#18966 = CARTESIAN_POINT ( 'NONE',  ( -338.8365100919713200, 240.0000000000001137, -197.2499999999919282 ) ) ;
#18967 = CARTESIAN_POINT ( 'NONE',  ( 755.3028492785439312, -255.2817908451526705, -335.9200461376539693 ) ) ;
#18968 = CARTESIAN_POINT ( 'NONE',  ( 787.5162901302840055, -155.3618753856927128, -305.4481719005792684 ) ) ;
#18969 = AXIS2_PLACEMENT_3D ( 'NONE', #33653, #19794, #16101 ) ;
#18970 = CARTESIAN_POINT ( 'NONE',  ( 751.9810565676468741, -50.08914811296584446, 360.9747183278973921 ) ) ;
#18971 = CARTESIAN_POINT ( 'NONE',  ( 772.4837098697144029, -119.3618753856928691, 374.5518280994205611 ) ) ;
#18972 = DIRECTION ( 'NONE',  ( 0.000000000000000000, 0.000000000000000000, 1.000000000000000000 ) ) ;
#18973 = FACE_OUTER_BOUND ( 'NONE', #44593, .T. ) ;
#18974 = EDGE_CURVE ( 'NONE', #22826, #31261, #31351, .T. ) ;
#18975 = CARTESIAN_POINT ( 'NONE',  ( 797.8822607201568644, -390.5545181178794678, 370.1134526219340160 ) ) ;
#18976 = CARTESIAN_POINT ( 'NONE',  ( 939.9999999999992042, 62.85347435602262323, 357.4246812887967621 ) ) ;
#18977 = CARTESIAN_POINT ( 'NONE',  ( 767.6429770376289525, -345.1800572038739006, 306.8695393053162093 ) ) ;
#18978 = EDGE_CURVE ( 'NONE', #15586, #27126, #21024, .T. ) ;
#18979 = CARTESIAN_POINT ( 'NONE',  ( 755.0636971347428243, -316.2709662947832499, -341.7834795799807353 ) ) ;
#18980 = CARTESIAN_POINT ( 'NONE',  ( 805.0264073115434940, 17.64894916467593688, 339.4763451958999099 ) ) ;
#18981 = CARTESIAN_POINT ( 'NONE',  ( 814.8207195650702488, -98.19088175424404596, -336.2433038121456548 ) ) ;
#18982 = CARTESIAN_POINT ( 'NONE',  ( 790.8726784830453198, -106.7146871989600498, -362.5472867521010585 ) ) ;
#18983 = CARTESIAN_POINT ( 'NONE',  ( 810.1134526219336749, -128.5328690171417634, 357.8822607201570349 ) ) ;
#18984 = CARTESIAN_POINT ( 'NONE',  ( 785.3687786644885591, -443.3618753856917465, 315.3201227861280813 ) ) ;
#18985 = AXIS2_PLACEMENT_3D ( 'NONE', #9117, #29316, #34275 ) ;
#18986 = CARTESIAN_POINT ( 'NONE',  ( 792.1044303154645831, -36.45278447660223975, -317.8323909638837677 ) ) ;
#18987 = CARTESIAN_POINT ( 'NONE',  ( 790.8726784830453198, -130.7146871989599504, -362.5472867521010585 ) ) ;
#18988 = CARTESIAN_POINT ( 'NONE',  ( 755.3201227861273992, -123.7255117493292147, 345.3687786644892981 ) ) ;
#18989 = CARTESIAN_POINT ( 'NONE',  ( 803.8651313633788504, -437.2601417444135450, -332.4468031744301015 ) ) ;
#18991 = CARTESIAN_POINT ( 'NONE',  ( 758.0580252608178853, -246.4527844766016074, 328.0187753319985404 ) ) ;
#18990 = CARTESIAN_POINT ( 'NONE',  ( 771.1735550268778070, -273.1800572038742985, 316.3353852180827630 ) ) ;
#18992 = CARTESIAN_POINT ( 'NONE',  ( -598.8365100919716042, 260.0000000000001705, -199.9999999999899671 ) ) ;
#18993 = ORIENTED_EDGE ( 'NONE', *, *, #1284, .T. ) ;
#18994 = CARTESIAN_POINT ( 'NONE',  ( 803.6646147819161570, -449.9073299311463643, 348.8264449731210561 ) ) ;
#18995 = CIRCLE ( 'NONE', #28589, 8.024999999999948841 ) ;
#18996 = ORIENTED_EDGE ( 'NONE', *, *, #10845, .F. ) ;
#18997 = CARTESIAN_POINT ( 'NONE',  ( 751.9810565676468741, -170.0891481129654608, 360.9747183278973921 ) ) ;
#18998 = CARTESIAN_POINT ( 'NONE',  ( 758.4439275373578084, -300.5545181178797520, 353.2243759319684386 ) ) ;
#18999 = CARTESIAN_POINT ( 'NONE',  ( 801.3366627262608972, -416.5328690171409107, 353.0897708529566899 ) ) ;
#19000 = ORIENTED_EDGE ( 'NONE', *, *, #1578, .F. ) ;
#19001 = CARTESIAN_POINT ( 'NONE',  ( 755.5913626894240451, -85.64542720878952764, -346.6156483768012890 ) ) ;
#19002 = CARTESIAN_POINT ( 'NONE',  ( 802.1676090361155502, -278.6346026584196807, -327.8955696845344505 ) ) ;
#19003 = VERTEX_POINT ( 'NONE', #12800 ) ;
#19004 = CARTESIAN_POINT ( 'NONE',  ( 778.2165204200184689, -382.8164208402374697, -364.9363028652563230 ) ) ;
#19005 = CARTESIAN_POINT ( 'NONE',  ( 785.3687786644884454, -35.36187538569316047, -315.3201227861279676 ) ) ;
#19006 = CARTESIAN_POINT ( 'NONE',  ( 776.9566956441375396, -252.8965053807777394, 364.8461984189686405 ) ) ;
#19007 = PLANE ( 'NONE',  #18922 ) ;
#19008 = DIRECTION ( 'NONE',  ( 0.000000000000000000, 0.000000000000000000, 1.000000000000000000 ) ) ;
#19009 = CARTESIAN_POINT ( 'NONE',  ( 793.5525998758768083, -31.09997266333516919, -372.6845335610516941 ) ) ;
#19010 = DIRECTION ( 'NONE',  ( 0.000000000000000000, 0.000000000000000000, 1.000000000000000000 ) ) ;
#19011 = ORIENTED_EDGE ( 'NONE', *, *, #25000, .T. ) ;
#19012 = CARTESIAN_POINT ( 'NONE',  ( 752.7379699480933368, -324.0090635724251911, -361.9858362298580232 ) ) ;
#19013 = CARTESIAN_POINT ( 'NONE',  ( 799.9636004259356241, -166.9181544815165523, 311.2241431872006956 ) ) ;
#19015 = CARTESIAN_POINT ( 'NONE',  ( 800.0135310231082713, -278.0891481129651197, -325.0180583372163028 ) ) ;
#19014 = CARTESIAN_POINT ( 'NONE',  ( -786.4999999999993179, -494.6608068873671300, -357.6536686473015720 ) ) ;
#19016 = CARTESIAN_POINT ( 'NONE',  ( 200.7583438952258916, 294.6698570112193920, -244.9999999999999716 ) ) ;
#19017 = CARTESIAN_POINT ( 'NONE',  ( 775.8780910478218402, -153.2817908451529831, -364.9511171171680530 ) ) ;
#19018 = ADVANCED_FACE ( 'NONE', ( #38157 ), #9967, .F. ) ;
#19019 = APPLICATION_CONTEXT ( 'automotive_design' ) ;
#19020 = CARTESIAN_POINT ( 'NONE',  ( -26.63011601220122060, 26.27639943461401018, 900.0000000000001137 ) ) ;
#19021 = CARTESIAN_POINT ( 'NONE',  ( 795.6651683502461765, -10.71468719896033761, -371.3240766477733814 ) ) ;
#19022 = CARTESIAN_POINT ( 'NONE',  ( 813.1304606946831655, -329.9073299311467622, -352.3570229623691716 ) ) ;
#19023 = LINE ( 'NONE', #1451, #37923 ) ;
#19024 = CARTESIAN_POINT ( 'NONE',  ( 774.6312213355099630, -47.36187538569312494, 364.6798772138717482 ) ) ;
#19025 = CARTESIAN_POINT ( 'NONE',  ( 752.7379699480933368, -300.0090635724252479, 361.9858362298580232 ) ) ;
#19026 = CARTESIAN_POINT ( 'NONE',  ( 771.2368401574024119, -253.4419599262323572, -374.2805881961240857 ) ) ;
#19027 = CARTESIAN_POINT ( 'NONE',  ( 801.1904061080336987, -260.0891481129650060, 368.3070685750235498 ) ) ;
#19028 = CARTESIAN_POINT ( 'NONE',  ( 808.7758568127978833, -436.1692326535044231, -320.0363995740631822 ) ) ;
#19029 = ADVANCED_FACE ( 'NONE', ( #37287 ), #1119, .F. ) ;
#19030 = DIRECTION ( 'NONE',  ( 0.000000000000000000, 0.000000000000000000, -1.000000000000000000 ) ) ;
#19031 = VERTEX_POINT ( 'NONE', #20584 ) ;
#19032 = CARTESIAN_POINT ( 'NONE',  ( 791.9812246680005501, -356.6346026584193964, 361.9419747391813189 ) ) ;
#19033 = CARTESIAN_POINT ( 'NONE',  ( 786.5483106153019435, -127.6454272087894140, 364.1601925771022366 ) ) ;
#19034 = CARTESIAN_POINT ( 'NONE',  ( 783.0433043558608688, -0.8965053807785533513, -315.1538015810313027 ) ) ;
#19035 = LINE ( 'NONE', #29869, #35072 ) ;
#19036 = DIRECTION ( 'NONE',  ( 0.000000000000000000, 0.000000000000000000, 1.000000000000000000 ) ) ;
#19037 = CARTESIAN_POINT ( 'NONE',  ( 785.3141322388236176, -405.7255117493283478, 364.4286716492789537 ) ) ;
#19038 = ORIENTED_EDGE ( 'NONE', *, *, #45342, .F. ) ;
#19039 = CARTESIAN_POINT ( 'NONE',  ( 805.1016975059191054, -318.8965053807775121, -343.0745993439771837 ) ) ;
#19040 = CARTESIAN_POINT ( 'NONE',  ( 765.0180583372156207, -168.9982390220563673, 360.0135310231089534 ) ) ;
#19041 = CARTESIAN_POINT ( 'NONE',  ( 815.0009284576459549, -342.3510508353228943, -338.7629533639073429 ) ) ;
#19042 = LINE ( 'NONE', #43729, #38179 ) ;
#19043 = ADVANCED_FACE ( 'NONE', ( #33597, #10193 ), #45546, .T. ) ;
#19044 = EDGE_LOOP ( 'NONE', ( #37679, #20127 ) ) ;
#19045 = CARTESIAN_POINT ( 'NONE',  ( 774.6312213355099630, -359.3618753856920875, 364.6798772138717482 ) ) ;
#19046 = EDGE_CURVE ( 'NONE', #37602, #34587, #29, .T. ) ;
#19047 = ORIENTED_EDGE ( 'NONE', *, *, #9197, .T. ) ;
#19048 = CARTESIAN_POINT ( 'NONE',  ( 797.6776695296629214, -451.5436935675099903, 357.6776695296636603 ) ) ;
#19049 = CARTESIAN_POINT ( 'NONE',  ( 745.4481719005789273, -171.7255117493291152, -347.5162901302853129 ) ) ;
#19050 = CARTESIAN_POINT ( 'NONE',  ( 777.4774526936600978, -82.27096629478390355, 304.7301800767028226 ) ) ;
#19051 = EDGE_LOOP ( 'NONE', ( #19991, #36260, #8028, #41362 ) ) ;
#19052 = CARTESIAN_POINT ( 'NONE',  ( 768.0187753319979720, -176.6346026584199933, -318.0580252608186242 ) ) ;
#19053 = ORIENTED_EDGE ( 'NONE', *, *, #31446, .F. ) ;
#19054 = AXIS2_PLACEMENT_3D ( 'NONE', #14032, #44986, #13342 ) ;
#19055 = CARTESIAN_POINT ( 'NONE',  ( 786.5483106153019435, -415.6454272087885897, -364.1601925771022366 ) ) ;
#19056 = CARTESIAN_POINT ( 'NONE',  ( 803.4237431249931660, 8.819942796124882634, 331.2633955100225194 ) ) ;
#19057 = CARTESIAN_POINT ( 'NONE',  ( 755.2512626584698410, -223.5436935675107577, 315.2512626584710915 ) ) ;
#19058 = CARTESIAN_POINT ( 'NONE',  ( 765.8855110935204493, -166.1692326535053041, 319.0159684113471599 ) ) ;
#19061 = CARTESIAN_POINT ( 'NONE',  ( 801.9858362298568863, -411.0783235625954717, 312.7379699480935642 ) ) ;
#19060 = CARTESIAN_POINT ( 'NONE',  ( 879.9999999999992042, 239.9999999999998863, -224.9999999999999716 ) ) ;
#19059 = CARTESIAN_POINT ( 'NONE',  ( 999.9999999999992042, 248.9999999999998863, -359.0000000000000000 ) ) ;
#19062 = ORIENTED_EDGE ( 'NONE', *, *, #9522, .T. ) ;
#19063 = CARTESIAN_POINT ( 'NONE',  ( 793.9708237608222134, -430.9181544815157849, -319.2295555964448681 ) ) ;
#19064 = CARTESIAN_POINT ( 'NONE',  ( -190.7583438952259485, 394.6698570112193920, -244.9999999999999716 ) ) ;
#19065 = CARTESIAN_POINT ( 'NONE',  ( 804.1009440267234822, -191.4636090269709996, -314.0944755984392600 ) ) ;
#19066 = CARTESIAN_POINT ( 'NONE',  ( 744.6391490659812007, -62.73633629969871350, 338.7502325331110455 ) ) ;
#19068 = CARTESIAN_POINT ( 'NONE',  ( 792.1044303154645831, -204.4527844766016926, -317.8323909638837677 ) ) ;
#19067 = LINE ( 'NONE', #26439, #18258 ) ;
#19069 = ADVANCED_FACE ( 'NONE', ( #31662 ), #42067, .F. ) ;
#19070 = CARTESIAN_POINT ( 'NONE',  ( 783.0433043558608688, -336.8965053807774552, -315.1538015810313027 ) ) ;
#19071 = CYLINDRICAL_SURFACE ( 'NONE', #4816, 6.118999999999985562 ) ;
#19072 = CARTESIAN_POINT ( 'NONE',  ( 745.1792804349281596, -206.1908817542437191, -343.7566961878542884 ) ) ;
#19073 = CARTESIAN_POINT ( 'NONE',  ( 799.9999999999993179, 205.0000000000000568, 319.9999999999999432 ) ) ;
#19074 = CARTESIAN_POINT ( 'NONE',  ( 784.9999999999992042, 239.9999999999998863, -235.0000000000000000 ) ) ;
#19075 = CARTESIAN_POINT ( 'NONE',  ( 802.5472867521000353, -52.37269993606237506, -350.8726784830461156 ) ) ;
#19076 = CARTESIAN_POINT ( 'NONE',  ( 763.8424801807145741, -402.0090635724250205, 320.5453621957614700 ) ) ;
#19077 = EDGE_CURVE ( 'NONE', #5018, #7856, #16050, .T. ) ;
#19078 = CARTESIAN_POINT ( 'NONE',  ( 754.9967657858570647, -241.5436935675106440, -365.0032342141425943 ) ) ;
#19079 = PLANE ( 'NONE',  #33465 ) ;
#19080 = CARTESIAN_POINT ( 'NONE',  ( 771.2633955100217236, -23.90732993114773919, -363.4237431249939618 ) ) ;
#19081 = CARTESIAN_POINT ( 'NONE',  ( 766.4474001241216001, -187.0999726633346825, 307.3154664389482491 ) ) ;
#19082 = CARTESIAN_POINT ( 'NONE',  ( 764.3348316497523456, -142.7146871989599219, -308.6759233522265617 ) ) ;
#19083 = CARTESIAN_POINT ( 'NONE',  ( 782.5225473063381969, -142.2709662947837330, 375.2698199232970637 ) ) ;
#19084 = CARTESIAN_POINT ( 'NONE',  ( 796.7737145352015204, -380.6346026584192828, -370.7187646348536987 ) ) ;
#19085 = EDGE_CURVE ( 'NONE', #25624, #27436, #6956, .T. ) ;
#19086 = ADVANCED_FACE ( 'NONE', ( #17125 ), #27747, .F. ) ;
#19087 = CARTESIAN_POINT ( 'NONE',  ( 799.9999999999993179, -365.3551492539851893, -18.13243251470705886 ) ) ;
#19088 = FACE_OUTER_BOUND ( 'NONE', #40190, .T. ) ;
#19089 = CARTESIAN_POINT ( 'NONE',  ( 785.3141322388236176, -237.7255117493289163, 364.4286716492789537 ) ) ;
#19090 = CARTESIAN_POINT ( 'NONE',  ( 793.0897708529556667, -6.554518117880697048, 361.3366627262616362 ) ) ;
#19091 = CARTESIAN_POINT ( 'NONE',  ( 804.9363028652555840, -400.2709662947828519, -338.2165204200192079 ) ) ;
#19092 = CIRCLE ( 'NONE', #44159, 10.00000000000000888 ) ;
#19093 = CARTESIAN_POINT ( 'NONE',  ( 796.7737145352015204, -452.6346026584191691, -370.7187646348536987 ) ) ;
#19094 = LINE ( 'NONE', #8703, #6282 ) ;
#19095 = CARTESIAN_POINT ( 'NONE',  ( 746.7653713866222915, -17.26014174441486659, 351.0478386215610271 ) ) ;
#19096 = EDGE_LOOP ( 'NONE', ( #33253, #530, #14267, #24315 ) ) ;
#19097 = CARTESIAN_POINT ( 'NONE',  ( 760.5453621957607311, -237.0783235625960117, -323.8424801807151425 ) ) ;
#19098 = CARTESIAN_POINT ( 'NONE',  ( 781.8018195045266339, -22.27096629478410250, 365.1927285166406705 ) ) ;
#19099 = CARTESIAN_POINT ( 'NONE',  ( 747.3154664389472828, -211.9874144716869750, -326.4474001241230781 ) ) ;
#19100 = DIRECTION ( 'NONE',  ( 0.000000000000000000, -0.000000000000000000, -1.000000000000000000 ) ) ;
#19101 = CARTESIAN_POINT ( 'NONE',  ( 758.0141637701419768, -351.0783235625955854, 367.2620300519063790 ) ) ;
#19102 = ORIENTED_EDGE ( 'NONE', *, *, #35641, .T. ) ;
#19103 = CARTESIAN_POINT ( 'NONE',  ( 758.0580252608178853, -270.4527844766014937, 328.0187753319985404 ) ) ;
#19104 = CARTESIAN_POINT ( 'NONE',  ( 798.0661480581538854, -434.5328690171407970, 309.5768839229118043 ) ) ;
#19105 = CARTESIAN_POINT ( 'NONE',  ( 756.5762568750052424, -147.1800572038746395, -348.7366044899774238 ) ) ;
#19106 = CARTESIAN_POINT ( 'NONE',  ( 781.7834795799800531, -322.8164208402377540, 315.0636971347436202 ) ) ;
#19107 = CARTESIAN_POINT ( 'NONE',  ( 751.6929314249748586, -78.99823902205662307, -318.8095938919659034 ) ) ;
#19108 = CARTESIAN_POINT ( 'NONE',  ( 797.8594530101009923, -85.54369356751118403, -322.1405469898982119 ) ) ;
#19109 = ORIENTED_EDGE ( 'NONE', *, *, #25259, .F. ) ;
#19110 = CARTESIAN_POINT ( 'NONE',  ( 772.4468031744293057, -9.827245390607961539, -363.8651313633793620 ) ) ;
#19111 = ORIENTED_EDGE ( 'NONE', *, *, #21005, .F. ) ;
#19112 = CARTESIAN_POINT ( 'NONE',  ( 804.1105419155481968, -315.8272453906070609, -347.6308680596136469 ) ) ;
#19114 = CARTESIAN_POINT ( 'NONE',  ( 804.6971507214547046, -363.2817908451523294, 344.0799538623459739 ) ) ;
#19113 = CARTESIAN_POINT ( 'NONE',  ( 803.6646147819161570, -41.90732993114767169, 348.8264449731210561 ) ) ;
#19117 = CARTESIAN_POINT ( 'NONE',  ( 815.0009284576459549, -318.3510508353230080, 338.7629533639073429 ) ) ;
#19116 = DIRECTION ( 'NONE',  ( 0.000000000000000000, 0.6755902076156505842, 0.7372773368101327440 ) ) ;
#19115 = CARTESIAN_POINT ( 'NONE',  ( 800.9747183278959710, -420.9982390220555999, 311.9810565676471583 ) ) ;
#19118 = CARTESIAN_POINT ( 'NONE',  ( 746.7653713866222915, -89.26014174441463922, 351.0478386215610271 ) ) ;
#19119 = CARTESIAN_POINT ( 'NONE',  ( 757.0176451133909268, -325.0999726633342561, -349.9200121543848354 ) ) ;
#19120 = CARTESIAN_POINT ( 'NONE',  ( 803.6646147819161570, -281.9073299311468759, -348.8264449731210561 ) ) ;
#19121 = CARTESIAN_POINT ( 'NONE',  ( 804.6798772138708955, -159.7255117493291436, -334.6312213355107019 ) ) ;
#19122 = AXIS2_PLACEMENT_3D ( 'NONE', #21739, #32830, #33067 ) ;
#19123 = CARTESIAN_POINT ( 'NONE',  ( 782.5225473063381969, -430.2709662947827383, 375.2698199232970637 ) ) ;
#19125 = FACE_OUTER_BOUND ( 'NONE', #6869, .T. ) ;
#19124 = FACE_OUTER_BOUND ( 'NONE', #26747, .T. ) ;
#19126 = EDGE_CURVE ( 'NONE', #25632, #30441, #30132, .T. ) ;
#19127 = CARTESIAN_POINT ( 'NONE',  ( 778.7629533639073998, -128.7363362996984790, -375.0009284576466371 ) ) ;
#19128 = CARTESIAN_POINT ( 'NONE',  ( 914.9999999999992042, -431.4567479753239354, -350.0000000000000000 ) ) ;
#19129 = DIRECTION ( 'NONE',  ( -1.000000000000000000, -5.551115123125783688E-16, 0.000000000000000000 ) ) ;
#19130 = CARTESIAN_POINT ( 'NONE',  ( 802.9823548866075953, -289.0999726633343698, 330.0799878456151077 ) ) ;
#19131 = ORIENTED_EDGE ( 'NONE', *, *, #3316, .T. ) ;
#19132 = CARTESIAN_POINT ( 'NONE',  ( 814.2001403089898304, -137.3618753856928265, -347.4397851343538264 ) ) ;
#19133 = CARTESIAN_POINT ( 'NONE',  ( 701.1634899080286232, 239.9999999999999432, -199.9999999999990337 ) ) ;
#19134 = CARTESIAN_POINT ( 'NONE',  ( 745.5313806188320314, -87.28179084515316788, 333.7943932421247268 ) ) ;
#19135 = CARTESIAN_POINT ( 'NONE',  ( 805.0032342141412300, -277.5436935675105019, -314.9967657858571783 ) ) ;
#19136 = CARTESIAN_POINT ( 'NONE',  ( 744.7301800767020268, -436.8164208402372992, -337.4774526936615189 ) ) ;
#19137 = CARTESIAN_POINT ( 'NONE',  ( 754.8072714833581358, -100.8164208402383792, 338.1981804954720587 ) ) ;
#19138 = EDGE_LOOP ( 'NONE', ( #35677, #31592 ) ) ;
#19139 = CARTESIAN_POINT ( 'NONE',  ( 752.4576283171824116, -333.0783235625956991, -317.7880784355627952 ) ) ;
#19140 = CARTESIAN_POINT ( 'NONE',  ( 811.0346526505616112, -86.63460265842023489, -323.0537975583477532 ) ) ;
#19141 = CARTESIAN_POINT ( 'NONE',  ( 798.5707757039680246, -5.463609026971610660, 356.7845633553585003 ) ) ;
#19142 = CARTESIAN_POINT ( 'NONE',  ( 747.2067596250078623, -363.1800572038739006, -352.2312462859687230 ) ) ;
#19143 = DIRECTION ( 'NONE',  ( -0.000000000000000000, 1.000000000000000000, -0.000000000000000000 ) ) ;
#19144 = CARTESIAN_POINT ( 'NONE',  ( 804.9511171171677688, -389.8055962898682765, 335.8780910478229202 ) ) ;
#19145 = ORIENTED_EDGE ( 'NONE', *, *, #20363, .F. ) ;
#19146 = CARTESIAN_POINT ( 'NONE',  ( 795.9930595647434757, -75.07832356259649487, 320.7433823573372820 ) ) ;
#19147 = CARTESIAN_POINT ( 'NONE',  ( 788.7631598425961101, -121.4419599262327267, -305.7194118038759143 ) ) ;
#19148 = FACE_OUTER_BOUND ( 'NONE', #29946, .T. ) ;
#19149 = CARTESIAN_POINT ( 'NONE',  ( 771.2368401574024119, -229.4419599262323572, 374.2805881961240857 ) ) ;
#19150 = CARTESIAN_POINT ( 'NONE',  ( 771.2633955100217236, -47.90732993114767169, 363.4237431249939618 ) ) ;
#19151 = AXIS2_PLACEMENT_3D ( 'NONE', #41435, #16728, #17415 ) ;
#19152 = CARTESIAN_POINT ( 'NONE',  ( 769.1273215169530886, -238.7146871989596661, -317.4527132478988847 ) ) ;
#19153 = CARTESIAN_POINT ( 'NONE',  ( 756.5762568750052424, -219.1800572038744122, 348.7366044899774238 ) ) ;
#19154 = CARTESIAN_POINT ( 'NONE',  ( 796.9462024416508257, 11.54721552339760038, -308.9653473494370246 ) ) ;
#19155 = CARTESIAN_POINT ( 'NONE',  ( 798.0661480581538854, -74.53286901714196233, -309.5768839229118043 ) ) ;
#19156 = DIRECTION ( 'NONE',  ( -1.000000000000000000, -0.000000000000000000, 0.000000000000000000 ) ) ;
#19157 = ORIENTED_EDGE ( 'NONE', *, *, #32264, .T. ) ;
#19158 = ORIENTED_EDGE ( 'NONE', *, *, #23218, .T. ) ;
#19159 = CARTESIAN_POINT ( 'NONE',  ( 748.6759233522253680, -376.3726999360614514, -324.3348316497537098 ) ) ;
#19160 = CARTESIAN_POINT ( 'NONE',  ( 778.1981804954714335, -226.2709662947834204, -314.8072714833589885 ) ) ;
#19161 = CARTESIAN_POINT ( 'NONE',  ( 777.4774526936600978, -322.2709662947830793, 304.7301800767028226 ) ) ;
#19162 = CARTESIAN_POINT ( 'NONE',  ( 771.2368401574024119, -37.44195992623299674, 374.2805881961240857 ) ) ;
#19163 = CARTESIAN_POINT ( 'NONE',  ( 796.1575198192839480, -222.0090635724254184, -359.4546378042384163 ) ) ;
#19164 = CARTESIAN_POINT ( 'NONE',  ( 792.1044303154645831, -180.4527844766017211, -317.8323909638837677 ) ) ;
#19165 = CARTESIAN_POINT ( 'NONE',  ( 804.4286716492782716, -401.3618753856920307, -345.3141322388244703 ) ) ;
#19166 = EDGE_LOOP ( 'NONE', ( #9498, #3754, #11831, #13009 ) ) ;
#19167 = CARTESIAN_POINT ( 'NONE',  ( 781.7834795799800531, -226.8164208402380098, 315.0636971347436202 ) ) ;
#19168 = CARTESIAN_POINT ( 'NONE',  ( 804.9363028652555840, -112.2709662947838325, -338.2165204200192079 ) ) ;
#19169 = ORIENTED_EDGE ( 'NONE', *, *, #10363, .T. ) ;
#19170 = CARTESIAN_POINT ( 'NONE',  ( 782.5225473063381969, -334.2709662947829656, 375.2698199232970637 ) ) ;
#19171 = DIRECTION ( 'NONE',  ( 0.000000000000000000, -1.000000000000000000, 1.672022627447525240E-16 ) ) ;
#19172 = DIRECTION ( 'NONE',  ( 0.000000000000000000, 0.000000000000000000, -1.000000000000000000 ) ) ;
#19173 = DIRECTION ( 'NONE',  ( -0.000000000000000000, 1.000000000000000000, -0.000000000000000000 ) ) ;
#19174 = CARTESIAN_POINT ( 'NONE',  ( 757.4527132478984868, -208.3726999360619061, 329.1273215169538844 ) ) ;
#19175 = CARTESIAN_POINT ( 'NONE',  ( 785.3141322388236176, -93.72551174932934259, 364.4286716492789537 ) ) ;
#19176 = VERTEX_POINT ( 'NONE', #45305 ) ;
#19177 = CARTESIAN_POINT ( 'NONE',  ( 744.6391490659812007, -398.7363362996976548, -338.7502325331110455 ) ) ;
#19178 = CARTESIAN_POINT ( 'NONE',  ( 810.7187646348534145, -42.45278447660223264, -356.7737145352016341 ) ) ;
#19179 = CARTESIAN_POINT ( 'NONE',  ( 754.9735926884551418, -234.3510508353232638, 340.5236548041000333 ) ) ;
#19180 = CARTESIAN_POINT ( 'NONE',  ( 754.8072714833581358, -412.8164208402372992, -338.1981804954720587 ) ) ;
#19181 = CARTESIAN_POINT ( 'NONE',  ( 801.9419747391806368, -18.45278447660230725, -351.9812246680014027 ) ) ;
#19182 = DIRECTION ( 'NONE',  ( -0.000000000000000000, 1.000000000000000000, -0.000000000000000000 ) ) ;
#19183 = CARTESIAN_POINT ( 'NONE',  ( 804.8461984189677878, -266.1908817542435486, -336.9566956441385628 ) ) ;
#19184 = CARTESIAN_POINT ( 'NONE',  ( 801.1904061080336987, -164.0891481129655176, -368.3070685750235498 ) ) ;
#19185 = CARTESIAN_POINT ( 'NONE',  ( 808.0189434323515343, -38.08914811296587999, 319.0252816721025511 ) ) ;
#19186 = CARTESIAN_POINT ( 'NONE',  ( 805.0032342141412300, -133.5436935675110135, 314.9967657858571783 ) ) ;
#19187 = LINE ( 'NONE', #26341, #19557 ) ;
#19188 = FILL_AREA_STYLE ('',( #1620 ) ) ;
#19189 = LINE ( 'NONE', #15048, #43444 ) ;
#19190 = CARTESIAN_POINT ( 'NONE',  ( 814.5518280994195948, -351.7255117493284047, 332.4837098697145734 ) ) ;
#19191 = CARTESIAN_POINT ( 'NONE',  ( 768.0187753319979720, -320.6346026584195670, -318.0580252608186242 ) ) ;
#19192 = CARTESIAN_POINT ( 'NONE',  ( 804.4286716492782716, -449.3618753856918602, 345.3141322388244703 ) ) ;
#19193 = CARTESIAN_POINT ( 'NONE',  ( 754.3581564841646241, -89.46360902697134065, -316.1443688327762516 ) ) ;
#19194 = CARTESIAN_POINT ( 'NONE',  ( 776.9566956441375396, -108.8965053807782084, -364.8461984189686405 ) ) ;
#19195 = CARTESIAN_POINT ( 'NONE',  ( 761.9338519418445230, -134.5328690171417350, 370.4231160770881957 ) ) ;
#19196 = CARTESIAN_POINT ( 'NONE',  ( 804.6798772138710092, -447.7255117493281205, 334.6312213355106451 ) ) ;
#19197 = CARTESIAN_POINT ( 'NONE',  ( 781.7834795799800531, -34.81642084023861372, -315.0636971347436202 ) ) ;
#19198 = CARTESIAN_POINT ( 'NONE',  ( 769.1273215169530886, -142.7146871989599219, -317.4527132478988847 ) ) ;
#19199 = CARTESIAN_POINT ( 'NONE',  ( 762.1405469898971887, -121.5436935675110419, -357.8594530101015607 ) ) ;
#19200 = CARTESIAN_POINT ( 'NONE',  ( 771.2633955100217236, -119.9073299311474443, 363.4237431249939618 ) ) ;
#19201 = CARTESIAN_POINT ( 'NONE',  ( 802.7791456095903868, -436.7146871989589272, -329.0155153010375102 ) ) ;
#19203 = CARTESIAN_POINT ( 'NONE',  ( 801.9419747391806368, -258.4527844766016074, 351.9812246680014027 ) ) ;
#19202 = CARTESIAN_POINT ( 'NONE',  ( 755.5713283507202505, -269.3618753856924286, 334.6858677611754729 ) ) ;
#19204 = CARTESIAN_POINT ( 'NONE',  ( 784.4999999999993179, -513.1383975375929367, -349.9999999999999432 ) ) ;
#19205 = EDGE_LOOP ( 'NONE', ( #958, #43430, #13636, #3562 ) ) ;
#19206 = CARTESIAN_POINT ( 'NONE',  ( 779.4709603349208464, 23.64894916467591912, 314.7162404726379918 ) ) ;
#19207 = CARTESIAN_POINT ( 'NONE',  ( 744.6391490659812007, -278.7363362996980527, -338.7502325331110455 ) ) ;
#19208 = ORIENTED_EDGE ( 'NONE', *, *, #36564, .T. ) ;
#19209 = DIRECTION ( 'NONE',  ( 1.000000000000000000, 0.000000000000000000, 0.000000000000000000 ) ) ;
#19210 = CARTESIAN_POINT ( 'NONE',  ( 754.9967657858570647, -169.5436935675108998, 365.0032342141425943 ) ) ;
#19211 = CARTESIAN_POINT ( 'NONE',  ( 799.2566176426618085, -288.0090635724252479, 324.0069404352559559 ) ) ;
#19212 = CARTESIAN_POINT ( 'NONE',  ( 805.0264073115434940, -390.3510508353227237, 339.4763451958999099 ) ) ;
#19213 = ORIENTED_EDGE ( 'NONE', *, *, #39584, .F. ) ;
#19214 = CARTESIAN_POINT ( 'NONE',  ( 769.9779781133707957, -67.09997266333506616, -316.7813123517150871 ) ) ;
#19215 = CARTESIAN_POINT ( 'NONE',  ( 801.9419747391806368, -282.4527844766014937, -351.9812246680014027 ) ) ;
#19216 = ORIENTED_EDGE ( 'NONE', *, *, #4150, .F. ) ;
#19217 = CARTESIAN_POINT ( 'NONE',  ( 767.8955696845333705, -408.4527844766009252, -362.1676090361162323 ) ) ;
#19218 = CARTESIAN_POINT ( 'NONE',  ( 757.8323909638827445, -98.63460265842024910, -352.1044303154654358 ) ) ;
#19219 = CARTESIAN_POINT ( 'NONE',  ( 773.3843516231979720, -277.4419599262322436, 364.4086373105754433 ) ) ;
#19220 = CYLINDRICAL_SURFACE ( 'NONE', #41799, 10.00000000000000888 ) ;
#19221 = DIRECTION ( 'NONE',  ( 0.000000000000000000, 0.000000000000000000, -1.000000000000000000 ) ) ;
#19222 = CARTESIAN_POINT ( 'NONE',  ( 745.5313806188320314, -15.28179084515340058, -333.7943932421247268 ) ) ;
#19223 = DIRECTION ( 'NONE',  ( 0.000000000000000000, 0.000000000000000000, -1.000000000000000000 ) ) ;
#19224 = ORIENTED_EDGE ( 'NONE', *, *, #43262, .F. ) ;
#19225 = CARTESIAN_POINT ( 'NONE',  ( 760.0363995740630116, -322.9181544815161260, -368.7758568127991907 ) ) ;
#19226 = CARTESIAN_POINT ( 'NONE',  ( 815.3608509340175488, -194.7363362996982517, 341.2497674668889545 ) ) ;
#19228 = CARTESIAN_POINT ( 'NONE',  ( 794.9819416627830151, -300.9982390220559409, -319.9864689768909898 ) ) ;
#19227 = CARTESIAN_POINT ( 'NONE',  ( 799.9999999999993179, 205.0000000000000568, 350.0000000000000000 ) ) ;
#19229 = DIRECTION ( 'NONE',  ( -0.000000000000000000, -0.000000000000000000, 1.000000000000000000 ) ) ;
#19230 = CARTESIAN_POINT ( 'NONE',  ( 799.2566176426618085, -168.0090635724256458, -324.0069404352559559 ) ) ;
#19231 = CARTESIAN_POINT ( 'NONE',  ( 812.7932403749906598, -15.18005720387504631, 327.7687537140311633 ) ) ;
#19232 = CARTESIAN_POINT ( 'NONE',  ( 746.4999999999993179, -365.3551492539851893, -28.13243251470704109 ) ) ;
#19233 = CARTESIAN_POINT ( 'NONE',  ( 772.4837098697145166, -359.3618753856921444, -374.5518280994205611 ) ) ;
#19234 = CARTESIAN_POINT ( 'NONE',  ( 767.9999999999992042, 205.0000000000000568, 339.9999999999999432 ) ) ;
#19235 = CARTESIAN_POINT ( 'NONE',  ( 754.8072714833581358, -52.81642084023856398, 338.1981804954720587 ) ) ;
#19236 = CARTESIAN_POINT ( 'NONE',  ( 749.5768839229115201, -300.5545181178797520, 358.0661480581553064 ) ) ;
#19237 = CARTESIAN_POINT ( 'NONE',  ( 745.7998596910086917, -245.3618753856925139, 332.5602148656461168 ) ) ;
#19238 = CARTESIAN_POINT ( 'NONE',  ( 813.2346286133761168, -437.2601417444135450, -328.9521613784389160 ) ) ;
#19239 = FACE_OUTER_BOUND ( 'NONE', #20391, .T. ) ;
#19240 = DIRECTION ( 'NONE',  ( -0.000000000000000000, 0.000000000000000000, 1.000000000000000000 ) ) ;
#19241 = CARTESIAN_POINT ( 'NONE',  ( 781.7834795799800531, -346.8164208402376971, 315.0636971347436202 ) ) ;
#19242 = CARTESIAN_POINT ( 'NONE',  ( 758.4439275373578084, -108.5545181178803915, 353.2243759319684386 ) ) ;
#19243 = CARTESIAN_POINT ( 'NONE',  ( 754.8983024940795303, -18.89650538077849617, -336.9254006560228163 ) ) ;
#19244 = CARTESIAN_POINT ( 'NONE',  ( 939.9999999999993179, -426.1357934546398383, -350.0000000000000000 ) ) ;
#19245 = CARTESIAN_POINT ( 'NONE',  ( 879.9999999999992042, 259.9999999999998863, -219.9999999999999716 ) ) ;
#19246 = CARTESIAN_POINT ( 'NONE',  ( 805.9055244015594326, -123.6237781080508569, 315.8990559732753240 ) ) ;
#19247 = CARTESIAN_POINT ( 'NONE',  ( 768.0187753319979720, -392.6346026584193396, 318.0580252608186242 ) ) ;
#19248 = ORIENTED_EDGE ( 'NONE', *, *, #12079, .T. ) ;
#19249 = CARTESIAN_POINT ( 'NONE',  ( 799.4546378042377910, -345.0783235625956991, -356.1575198192848006 ) ) ;
#19250 = CARTESIAN_POINT ( 'NONE',  ( 788.8264449731200330, -141.1800572038746395, 363.6646147819171233 ) ) ;
#19251 = CARTESIAN_POINT ( 'NONE',  ( 808.7758568127978833, -316.1692326535048210, -320.0363995740631822 ) ) ;
#19252 = CARTESIAN_POINT ( 'NONE',  ( 792.0613484971601110, -458.0032201311295807, 367.4685979341032294 ) ) ;
#19253 = EDGE_LOOP ( 'NONE', ( #1527, #7244, #20300, #7482 ) ) ;
#19254 = CARTESIAN_POINT ( 'NONE',  ( 800.2193346964447755, -354.9982390220557704, 355.1360043628815788 ) ) ;
#19255 = VERTEX_POINT ( 'NONE', #12578 ) ;
#19256 = CARTESIAN_POINT ( 'NONE',  ( 51.16348990802859475, 260.0000000000000568, -199.9999999999945146 ) ) ;
#19257 = EDGE_CURVE ( 'NONE', #10891, #32443, #13665, .T. ) ;
#19258 = CARTESIAN_POINT ( 'NONE',  ( 751.9810565676468741, -194.0891481129654039, -360.9747183278973921 ) ) ;
#19259 = CARTESIAN_POINT ( 'NONE',  ( 754.9967657858570647, -73.54369356751121245, 365.0032342141425943 ) ) ;
#19260 = EDGE_LOOP ( 'NONE', ( #33404, #25154 ) ) ;
#19261 = CARTESIAN_POINT ( 'NONE',  ( 797.6776695296629214, -187.5436935675108430, -357.6776695296636603 ) ) ;
#19262 = ORIENTED_EDGE ( 'NONE', *, *, #426, .F. ) ;
#19263 = CARTESIAN_POINT ( 'NONE',  ( 775.8780910478218402, -441.2817908451521021, -364.9511171171680530 ) ) ;
#19264 = CARTESIAN_POINT ( 'NONE',  ( 782.5225473063381969, -262.2709662947831930, 375.2698199232970637 ) ) ;
#19265 = CARTESIAN_POINT ( 'NONE',  ( 790.8726784830453198, -154.7146871989598935, 362.5472867521010585 ) ) ;
#19267 = LINE ( 'NONE', #33356, #7851 ) ;
#19266 = CARTESIAN_POINT ( 'NONE',  ( -66.63011601220125613, -365.3551492539851893, -28.13243251470704109 ) ) ;
#19268 = ADVANCED_FACE ( 'NONE', ( #9110 ), #24270, .F. ) ;
#19269 = ORIENTED_EDGE ( 'NONE', *, *, #27224, .F. ) ;
#19270 = CARTESIAN_POINT ( 'NONE',  ( 804.1105419155481968, -411.8272453906067199, -347.6308680596136469 ) ) ;
#19271 = CYLINDRICAL_SURFACE ( 'NONE', #10080, 6.118999999999985562 ) ;
#19272 = CARTESIAN_POINT ( 'NONE',  ( 795.8262568251477660, -190.3726999360619629, -308.3538107759623585 ) ) ;
#19273 = AXIS2_PLACEMENT_3D ( 'NONE', #40489, #19229, #12314 ) ;
#19274 = CARTESIAN_POINT ( 'NONE',  ( 757.7880784355613741, -66.00906357242595845, 312.4576283171834916 ) ) ;
#19276 = CARTESIAN_POINT ( 'NONE',  ( 762.3223304703356007, -175.5436935675108998, -322.3223304703362828 ) ) ;
#19275 = CARTESIAN_POINT ( 'NONE',  ( -858.8365100919713768, 260.0000000000002274, -197.2499999999882903 ) ) ;
#19277 = CARTESIAN_POINT ( 'NONE',  ( 766.7756240680305382, -350.5328690171411381, -361.5560724626415663 ) ) ;
#19278 = CARTESIAN_POINT ( 'NONE',  ( -338.8365100919713200, 256.5000000000001137, -199.9999999999917861 ) ) ;
#19279 = CARTESIAN_POINT ( 'NONE',  ( 747.6481478633932056, -229.0999726633345404, -353.4146539503763620 ) ) ;
#19280 = CARTESIAN_POINT ( 'NONE',  ( 773.4999999999993179, -512.9681489794448908, -339.9999999999999432 ) ) ;
#19281 = CARTESIAN_POINT ( 'NONE',  ( 779.9999999999992042, 16.45630643248849267, -339.9999999999999432 ) ) ;
#19282 = CARTESIAN_POINT ( 'NONE',  ( 755.5913626894240451, -37.64542720878968396, -346.6156483768012890 ) ) ;
#19283 = CARTESIAN_POINT ( 'NONE',  ( 784.1219089521767955, -405.2817908451522158, 315.0488828828318333 ) ) ;
#19284 = CARTESIAN_POINT ( 'NONE',  ( 776.2046728542105711, -356.1908817542432075, 304.8212110874238761 ) ) ;
#19285 = CARTESIAN_POINT ( 'NONE',  ( 782.4968714119720516, -226.8164208402380098, -305.0891759886411023 ) ) ;
#19286 = CARTESIAN_POINT ( 'NONE',  ( 759.0159684113467620, -232.9181544815163249, 325.8855110935213020 ) ) ;
#19287 = LINE ( 'NONE', #33373, #30530 ) ;
#19288 = CARTESIAN_POINT ( 'NONE',  ( 799.9999999999993179, 205.0000000000000568, 339.9999999999999432 ) ) ;
#19289 = CARTESIAN_POINT ( 'NONE',  ( 800.2193346964447755, -42.99823902205675807, -355.1360043628815788 ) ) ;
#19290 = CARTESIAN_POINT ( 'NONE',  ( 814.4686193811664907, -195.2817908451528410, 346.2056067578752732 ) ) ;
#19291 = EDGE_CURVE ( 'NONE', #39949, #33570, #34897, .T. ) ;
#19292 = CARTESIAN_POINT ( 'NONE',  ( 813.2346286133761168, -149.2601417444144261, -328.9521613784389160 ) ) ;
#19293 = CARTESIAN_POINT ( 'NONE',  ( 749.2812353651451076, -150.4527844766018916, 323.2262854647983090 ) ) ;
#19294 = CARTESIAN_POINT ( 'NONE',  ( 796.9462024416508257, -372.4527844766010958, -308.9653473494370246 ) ) ;
#19295 = PLANE ( 'NONE',  #37946 ) ;
#19296 = EDGE_CURVE ( 'NONE', #21713, #30422, #13498, .T. ) ;
#19297 = CARTESIAN_POINT ( 'NONE',  ( 756.5762568750052424, -243.1800572038743269, 348.7366044899774238 ) ) ;
#19298 = CARTESIAN_POINT ( 'NONE',  ( 758.4439275373578084, -36.55451811788061178, 353.2243759319684386 ) ) ;
#19299 = CARTESIAN_POINT ( 'NONE',  ( 755.0636971347428243, -388.2709662947829656, -341.7834795799807353 ) ) ;
#19300 = DIRECTION ( 'NONE',  ( 1.000000000000000000, 0.000000000000000000, -0.000000000000000000 ) ) ;
#19301 = CARTESIAN_POINT ( 'NONE',  ( 811.0346526505616112, -446.6346026584189985, -323.0537975583477532 ) ) ;
#19302 = DIRECTION ( 'NONE',  ( 0.000000000000000000, 3.700743415417198493E-16, -1.000000000000000000 ) ) ;
#19304 = CARTESIAN_POINT ( 'NONE',  ( 803.6646147819161570, -305.9073299311467622, 348.8264449731210561 ) ) ;
#19303 = CARTESIAN_POINT ( 'NONE',  ( 756.1348686366196716, -89.26014174441463922, 347.5531968255698416 ) ) ;
#19305 = ORIENTED_EDGE ( 'NONE', *, *, #40995, .F. ) ;
#19306 = CARTESIAN_POINT ( 'NONE',  ( 789.9200121543843807, -217.9874144716870035, -317.0176451133914384 ) ) ;
#19307 = CARTESIAN_POINT ( 'NONE',  ( 756.5762568750052424, -51.18005720387493085, 348.7366044899774238 ) ) ;
#19308=STYLED_ITEM('',(#45758),#17697);
#19309 = CARTESIAN_POINT ( 'NONE',  ( 776.2433038121456548, -228.8965053807778816, -374.8207195650711014 ) ) ;
#19310 = DIRECTION ( 'NONE',  ( -0.000000000000000000, 1.000000000000000000, -0.000000000000000000 ) ) ;
#19311 = CARTESIAN_POINT ( 'NONE',  ( 759.8311093483677041, -358.1692326535047641, 310.9282345327691814 ) ) ;
#19312 = ORIENTED_EDGE ( 'NONE', *, *, #38068, .F. ) ;
#19313 = CARTESIAN_POINT ( 'NONE',  ( 805.9055244015594326, -435.6237781080499190, 315.8990559732753240 ) ) ;
#19314 = ADVANCED_FACE ( 'NONE', ( #2244, #36904, #19575 ), #28904, .T. ) ;
#19315 = CARTESIAN_POINT ( 'NONE',  ( 805.0264073115434940, -30.35105083532391390, -339.4763451958999099 ) ) ;
#19316 = CARTESIAN_POINT ( 'NONE',  ( 805.1927285166397041, -328.8164208402375834, 341.8018195045277707 ) ) ;
#19317 = EDGE_CURVE ( 'NONE', #45456, #6536, #9953, .T. ) ;
#19318 = CARTESIAN_POINT ( 'NONE',  ( 812.7932403749906598, -87.18005720387481006, -327.7687537140311633 ) ) ;
#19319 = CARTESIAN_POINT ( 'NONE',  ( 771.2633955100217236, -71.90732993114760063, -363.4237431249939618 ) ) ;
#19320 = EDGE_LOOP ( 'NONE', ( #1206, #11379, #10232, #44196 ) ) ;
#19321 = CARTESIAN_POINT ( 'NONE',  ( 763.8424801807145741, 5.990936427573807954, -320.5453621957614700 ) ) ;
#19322 = CARTESIAN_POINT ( 'NONE',  ( 780.5236548040995785, -332.7363362996979390, -314.9735926884559944 ) ) ;
#19324 = CARTESIAN_POINT ( 'NONE',  ( 793.9708237608222134, -358.9181544815160123, 319.2295555964448681 ) ) ;
#19323 = CARTESIAN_POINT ( 'NONE',  ( 792.1044303154645831, -108.4527844766019911, 317.8323909638837677 ) ) ;
#19325 = EDGE_CURVE ( 'NONE', #15262, #2064, #40606, .T. ) ;
#19328 = CARTESIAN_POINT ( 'NONE',  ( 791.1614460488616487, -323.2601417444138860, 373.5763878283158874 ) ) ;
#19327 = CARTESIAN_POINT ( 'NONE',  ( 998.9999999999992042, -600.0000000000001137, 360.0000000000000000 ) ) ;
#19326 = CARTESIAN_POINT ( 'NONE',  ( 745.7998596910086917, -413.3618753856920307, 332.5602148656461168 ) ) ;
#19329 = ADVANCED_FACE ( 'NONE', ( #23026, #12645 ), #37119, .T. ) ;
#19330 = CARTESIAN_POINT ( 'NONE',  ( 776.2433038121456548, -108.8965053807782084, 374.8207195650711014 ) ) ;
#19331 = CARTESIAN_POINT ( 'NONE',  ( 804.8461984189677878, -338.1908817542433212, -336.9566956441385628 ) ) ;
#19332 = CARTESIAN_POINT ( 'NONE',  ( 795.1360043628807261, -332.0891481129649492, -360.2193346964456282 ) ) ;
#19333 = CARTESIAN_POINT ( 'NONE',  ( 765.0180583372156207, -144.9982390220564525, -360.0135310231089534 ) ) ;
#19334 = CARTESIAN_POINT ( 'NONE',  ( 805.0032342141412300, -421.5436935675101040, 314.9967657858571783 ) ) ;
#19336 = CARTESIAN_POINT ( 'NONE',  ( 914.9999999999992042, -426.1357934546398383, 350.0000000000000000 ) ) ;
#19335 = DIRECTION ( 'NONE',  ( -0.000000000000000000, -0.000000000000000000, 1.000000000000000000 ) ) ;
#19337 = CARTESIAN_POINT ( 'NONE',  ( 793.5525998758768083, -127.0999726633348672, -372.6845335610516941 ) ) ;
#19338 = DIRECTION ( 'NONE',  ( 0.000000000000000000, 0.3826834323650836756, 0.9238795325112892920 ) ) ;
#19339 = DIRECTION ( 'NONE',  ( -0.000000000000000000, -0.000000000000000000, 1.000000000000000000 ) ) ;
#19340 = CARTESIAN_POINT ( 'NONE',  ( 804.8461984189677878, -290.1908817542434349, 336.9566956441385628 ) ) ;
#19341 = VERTEX_POINT ( 'NONE', #21735 ) ;
#19342 = AXIS2_PLACEMENT_3D ( 'NONE', #39432, #25090, #21632 ) ;
#19343 = CARTESIAN_POINT ( 'NONE',  ( 767.7687537140311633, -143.9073299311473590, -372.7932403749916830 ) ) ;
#19344 = EDGE_CURVE ( 'NONE', #12174, #16670, #15852, .T. ) ;
#19345 = DIRECTION ( 'NONE',  ( -1.000000000000000000, -0.000000000000000000, 0.000000000000000000 ) ) ;
#19346 = CARTESIAN_POINT ( 'NONE',  ( 804.1009440267234822, -71.46360902697141171, 314.0944755984392600 ) ) ;
#19347 = ADVANCED_FACE ( 'NONE', ( #44289 ), #8517, .T. ) ;
#19348 = CARTESIAN_POINT ( 'NONE',  ( 767.6429770376289525, -273.1800572038742985, -306.8695393053162093 ) ) ;
#19349 = CARTESIAN_POINT ( 'NONE',  ( 796.9462024416508257, -444.4527844766009821, -308.9653473494370246 ) ) ;
#19350 = CARTESIAN_POINT ( 'NONE',  ( 778.2165204200184689, -142.8164208402382656, 364.9363028652563230 ) ) ;
#19351 = ORIENTED_EDGE ( 'NONE', *, *, #43879, .F. ) ;
#19352 = CARTESIAN_POINT ( 'NONE',  ( 744.8212110874229666, -330.8965053807774552, -336.2046728542121627 ) ) ;
#19353 = CARTESIAN_POINT ( 'NONE',  ( 763.0537975583475827, -72.45278447660213317, -371.0346526505627480 ) ) ;
#19354 = CARTESIAN_POINT ( 'NONE',  ( 790.9844846989617508, -22.37269993606246743, 317.2208543904092721 ) ) ;
#19355 = CARTESIAN_POINT ( 'NONE',  ( 744.7301800767019131, -340.8164208402376971, -337.4774526936615757 ) ) ;
#19356 = CARTESIAN_POINT ( 'NONE',  ( 791.7608162188021197, 240.0000000000000853, 320.0000000000000000 ) ) ;
#19357 = CARTESIAN_POINT ( 'NONE',  ( 796.7845633553578182, -393.6237781080500326, 358.5707757039688204 ) ) ;
#19358 = ORIENTED_EDGE ( 'NONE', *, *, #39941, .F. ) ;
#19359 = CARTESIAN_POINT ( 'NONE',  ( 800.7704444035546203, -76.16923265350557415, 326.0291762391768771 ) ) ;
#19360 = CARTESIAN_POINT ( 'NONE',  ( 762.3223304703356007, -223.5436935675107577, -322.3223304703362828 ) ) ;
#19361 = VECTOR ( 'NONE', #37350, 1000.000000000000000 ) ;
#19362 = CARTESIAN_POINT ( 'NONE',  ( 795.6651683502461765, -130.7146871989599504, -371.3240766477733814 ) ) ;
#19363 = FILL_AREA_STYLE_COLOUR ( '', #25552 ) ;
#19364 = CARTESIAN_POINT ( 'NONE',  ( 811.6461892240364477, -244.7146871989596093, 324.1737431748509835 ) ) ;
#19365 = CARTESIAN_POINT ( 'NONE',  ( 771.2633955100217236, -95.90732993114751537, 363.4237431249939618 ) ) ;
#19366 = ORIENTED_EDGE ( 'NONE', *, *, #43078, .F. ) ;
#19367 = EDGE_CURVE ( 'NONE', #33185, #18651, #18155, .T. ) ;
#19368 = CARTESIAN_POINT ( 'NONE',  ( 787.6308680596127942, -227.2601417444141987, -364.1105419155492768 ) ) ;
#19369 = CARTESIAN_POINT ( 'NONE',  ( 757.8323909638827445, -242.6346026584197659, 352.1044303154654358 ) ) ;
#19370 = EDGE_CURVE ( 'NONE', #28770, #19677, #22542, .T. ) ;
#19371 = CARTESIAN_POINT ( 'NONE',  ( 805.0032342141412300, 10.45630643248850866, -314.9967657858571783 ) ) ;
#19372 = CARTESIAN_POINT ( 'NONE',  ( 813.2346286133761168, -77.26014174441466764, -328.9521613784389160 ) ) ;
#19373 = DIRECTION ( 'NONE',  ( 4.147566128926370535E-16, 1.000000000000000000, -0.000000000000000000 ) ) ;
#19374 = ORIENTED_EDGE ( 'NONE', *, *, #18482, .F. ) ;
#19375 = ORIENTED_EDGE ( 'NONE', *, *, #38536, .T. ) ;
#19376 = CARTESIAN_POINT ( 'NONE',  ( 746.4236121716829757, -375.8272453906069472, -328.8385539511384650 ) ) ;
#19377 = CARTESIAN_POINT ( 'NONE',  ( 782.5225473063383106, -334.2709662947830793, 375.2698199232970637 ) ) ;
#19378 = CARTESIAN_POINT ( 'NONE',  ( 798.0661480581538854, -26.53286901714210799, 309.5768839229118043 ) ) ;
#19379 = CARTESIAN_POINT ( 'NONE',  ( 755.5913626894240451, -205.6454272087891297, -346.6156483768012890 ) ) ;
#19380 = CARTESIAN_POINT ( 'NONE',  ( 781.7834795799800531, -202.8164208402380950, -315.0636971347436202 ) ) ;
#19381 = CARTESIAN_POINT ( 'NONE',  ( 764.8639956371174549, -392.0891481129647786, -319.7806653035542581 ) ) ;
#19382 = VERTEX_POINT ( 'NONE', #3161 ) ;
#19383 = CARTESIAN_POINT ( 'NONE',  ( 788.7366044899766848, -203.9073299311471885, 316.5762568750059813 ) ) ;
#19384 = CARTESIAN_POINT ( 'NONE',  ( 785.3141322388236176, -93.72551174932934259, -364.4286716492789537 ) ) ;
#19385 = ORIENTED_EDGE ( 'NONE', *, *, #28721, .T. ) ;
#19386 = CARTESIAN_POINT ( 'NONE',  ( 749.2812353651451076, -318.4527844766014368, 323.2262854647983090 ) ) ;
#19387 = DIRECTION ( 'NONE',  ( -0.000000000000000000, 1.000000000000000000, -0.000000000000000000 ) ) ;
#19388 = CARTESIAN_POINT ( 'NONE',  ( 831.1634899080286232, 239.9999999999999147, -202.7499999999998295 ) ) ;
#19389 = FACE_OUTER_BOUND ( 'NONE', #33303, .T. ) ;
#19390 = CARTESIAN_POINT ( 'NONE',  ( 790.0220218866281812, -175.0999726633346825, 363.2186876482849129 ) ) ;
#19391 = CARTESIAN_POINT ( 'NONE',  ( 767.8955696845333705, -72.45278447660213317, 362.1676090361162323 ) ) ;
#19392 = ORIENTED_EDGE ( 'NONE', *, *, #20155, .F. ) ;
#19393 = CARTESIAN_POINT ( 'NONE',  ( 799.9636004259356241, -454.9181544815156713, -311.2241431872006956 ) ) ;
#19394 = AXIS2_PLACEMENT_3D ( 'NONE', #21399, #32007, #28309 ) ;
#19395 = CARTESIAN_POINT ( 'NONE',  ( 745.7998596910086917, -29.36187538569318178, -332.5602148656461168 ) ) ;
#19396 = PRODUCT_DEFINITION_FORMATION_WITH_SPECIFIED_SOURCE ( 'ANY', '', #28487, .NOT_KNOWN. ) ;
#19397 = CARTESIAN_POINT ( 'NONE',  ( 786.6156483768007774, -241.4419599262322720, 315.5913626894246136 ) ) ;
#19398 = CARTESIAN_POINT ( 'NONE',  ( 756.3353852180819104, -389.9073299311465348, -331.1735550268788302 ) ) ;
#19399 = CARTESIAN_POINT ( 'NONE',  ( 781.8018195045267476, -22.27096629478410605, -365.1927285166407273 ) ) ;
#19400 = CARTESIAN_POINT ( 'NONE',  ( 814.2001403089898304, -425.3618753856919170, 347.4397851343538264 ) ) ;
#19401 = FACE_OUTER_BOUND ( 'NONE', #41530, .T. ) ;
#19402 = CARTESIAN_POINT ( 'NONE',  ( 763.8424801807145741, -282.0090635724253048, -320.5453621957614700 ) ) ;
#19403 = CARTESIAN_POINT ( 'NONE',  ( 813.1304606946830518, -161.9073299311472454, -352.3570229623690580 ) ) ;
#19404 = CARTESIAN_POINT ( 'NONE',  ( 747.2067596250078623, -51.18005720387493085, 352.2312462859687230 ) ) ;
#19405 = CARTESIAN_POINT ( 'NONE',  ( 782.5225473063381969, -142.2709662947837330, 375.2698199232970637 ) ) ;
#19406 = CARTESIAN_POINT ( 'NONE',  ( 701.1634899080286232, 239.9999999999999147, -199.9999999999990337 ) ) ;
#19407 = DIRECTION ( 'NONE',  ( 0.000000000000000000, 0.000000000000000000, 1.000000000000000000 ) ) ;
#19408 = CARTESIAN_POINT ( 'NONE',  ( 989.9999999999992042, 249.9999999999998863, -350.0000000000000000 ) ) ;
#19409 = CARTESIAN_POINT ( 'NONE',  ( 808.0189434323515343, -374.0891481129647786, 319.0252816721025511 ) ) ;
#19410 = CARTESIAN_POINT ( 'NONE',  ( 767.8955696845333705, -360.4527844766010958, -362.1676090361162323 ) ) ;
#19411 = CARTESIAN_POINT ( 'NONE',  ( 803.2186876482843445, 16.01258552831230375, 350.0220218866286928 ) ) ;
#19412 = CARTESIAN_POINT ( 'NONE',  ( 812.3518521366052028, -97.09997266333496668, -326.5853460496235243 ) ) ;
#19413 = CARTESIAN_POINT ( 'NONE',  ( 754.8983024940795303, -114.8965053807782226, -336.9254006560228163 ) ) ;
#19414 = CARTESIAN_POINT ( 'NONE',  ( 747.3154664389472828, -139.9874144716872024, 326.4474001241230781 ) ) ;
#19415 = CARTESIAN_POINT ( 'NONE',  ( 791.9812246680005501, -428.6346026584192259, 361.9419747391813189 ) ) ;
#19416 = CARTESIAN_POINT ( 'NONE',  ( 762.3223304703356007, -31.54369356751135456, -322.3223304703362828 ) ) ;
#19417 = CARTESIAN_POINT ( 'NONE',  ( 779.4709603349208464, -120.3510508353236048, -314.7162404726379918 ) ) ;
#19418 = CARTESIAN_POINT ( 'NONE',  ( 778.1981804954714335, -130.2709662947837899, -314.8072714833589885 ) ) ;
#19419 = CARTESIAN_POINT ( 'NONE',  ( 759.7806653035534055, -126.9982390220565094, 324.8639956371180801 ) ) ;
#19420 = CARTESIAN_POINT ( 'NONE',  ( 755.8398074228967971, -427.4419599262317888, -333.4516893846970333 ) ) ;
#19421 = CARTESIAN_POINT ( 'NONE',  ( 774.6858677611749044, -273.7255117493288026, 315.5713283507209894 ) ) ;
#19422 = AXIS2_PLACEMENT_3D ( 'NONE', #40391, #1559, #20026 ) ;
#19423 = DIRECTION ( 'NONE',  ( 0.000000000000000000, 0.7372773368101331881, -0.6755902076156503622 ) ) ;
#19424 = ORIENTED_EDGE ( 'NONE', *, *, #20676, .F. ) ;
#19425 = CARTESIAN_POINT ( 'NONE',  ( 756.1348686366196716, 6.739858255585061464, 347.5531968255698416 ) ) ;
#19426 = VECTOR ( 'NONE', #19847, 1000.000000000000000 ) ;
#19427 = CARTESIAN_POINT ( 'NONE',  ( 748.6759233522253680, -256.3726999360617924, -324.3348316497537098 ) ) ;
#19428 = ORIENTED_EDGE ( 'NONE', *, *, #19574, .T. ) ;
#19429 = CARTESIAN_POINT ( 'NONE',  ( 800.9747183278959710, -204.9982390220562820, 311.9810565676471583 ) ) ;
#19430 = CARTESIAN_POINT ( 'NONE',  ( 776.9254006560222479, -308.1908817542434349, 314.8983024940802125 ) ) ;
#19431 = CARTESIAN_POINT ( 'NONE',  ( 772.3691319403857278, -407.2601417444137155, 315.8894580844506663 ) ) ;
#19432 = ORIENTED_EDGE ( 'NONE', *, *, #19626, .T. ) ;
#19433 = CARTESIAN_POINT ( 'NONE',  ( 757.0176451133909268, -109.0999726633349241, -349.9200121543848354 ) ) ;
#19434 = CARTESIAN_POINT ( 'NONE',  ( 797.6776695296629214, -283.5436935675105019, -357.6776695296636603 ) ) ;
#19435 = ORIENTED_EDGE ( 'NONE', *, *, #18568, .F. ) ;
#19436 = CARTESIAN_POINT ( 'NONE',  ( 755.3201227861273992, -435.7255117493282341, -345.3687786644892981 ) ) ;
#19437 = CARTESIAN_POINT ( 'NONE',  ( 774.6312213355099630, -95.36187538569294020, -364.6798772138717482 ) ) ;
#19438 = CARTESIAN_POINT ( 'NONE',  ( 804.1601925771018387, -295.4419599262320730, 346.5483106153029098 ) ) ;
#19439 = FACE_BOUND ( 'NONE', #41607, .T. ) ;
#19440 = DIRECTION ( 'NONE',  ( -1.880165489482579047E-16, -1.000000000000000000, -0.000000000000000000 ) ) ;
#19441 = CARTESIAN_POINT ( 'NONE',  ( 768.0187753319979720, 15.36539734157940629, 318.0580252608186242 ) ) ;
#19442 = VERTEX_POINT ( 'NONE', #35028 ) ;
#19443 = CARTESIAN_POINT ( 'NONE',  ( 745.1792804349281596, -326.1908817542433781, -343.7566961878542884 ) ) ;
#19444 = CARTESIAN_POINT ( 'NONE',  ( 799.9636004259356241, -214.9181544815164386, 311.2241431872006956 ) ) ;
#19446 = CARTESIAN_POINT ( 'NONE',  ( 797.8594530101008786, -301.5436935675105588, -322.1405469898980982 ) ) ;
#19445 = DIRECTION ( 'NONE',  ( -0.000000000000000000, 1.000000000000000000, -0.000000000000000000 ) ) ;
#19447 = SURFACE_SIDE_STYLE ('',( #12080 ) ) ;
#19448 = CARTESIAN_POINT ( 'NONE',  ( 793.0897708529556667, -150.5545181178802352, -361.3366627262616362 ) ) ;
#19449 = CARTESIAN_POINT ( 'NONE',  ( 755.2512626584698410, -55.54369356751127640, 315.2512626584710915 ) ) ;
#19450 = AXIS2_PLACEMENT_3D ( 'NONE', #37062, #12589, #26667 ) ;
#19451 = DIRECTION ( 'NONE',  ( -0.000000000000000000, -0.000000000000000000, 1.000000000000000000 ) ) ;
#19452 = CARTESIAN_POINT ( 'NONE',  ( 800.9747183278959710, -396.9982390220556567, -311.9810565676471583 ) ) ;
#19453 = AXIS2_PLACEMENT_3D ( 'NONE', #30362, #1958, #16058 ) ;
#19454 =( NAMED_UNIT ( * ) SI_UNIT ( $, .STERADIAN. ) SOLID_ANGLE_UNIT ( ) );
#19455 = CARTESIAN_POINT ( 'NONE',  ( 792.1044303154645831, -36.45278447660223975, 317.8323909638837677 ) ) ;
#19456 = CARTESIAN_POINT ( 'NONE',  ( 754.3581564841646241, -305.4636090269706870, 316.1443688327762516 ) ) ;
#19457 = CARTESIAN_POINT ( 'NONE',  ( 796.7737145352015204, -260.6346026584197375, 370.7187646348536987 ) ) ;
#19458 = CARTESIAN_POINT ( 'NONE',  ( 745.0891759886404770, -28.27096629478409540, -342.4968714119734159 ) ) ;
#19459 = CYLINDRICAL_SURFACE ( 'NONE', #4065, 10.00000000000000888 ) ;
#19460 = DIRECTION ( 'NONE',  ( 1.000000000000000000, 2.313994520913686024E-32, -2.750100768424433609E-32 ) ) ;
#19461 = CARTESIAN_POINT ( 'NONE',  ( 788.7366044899766848, -371.9073299311465917, 316.5762568750059813 ) ) ;
#19462 = CARTESIAN_POINT ( 'NONE',  ( 798.5707757039680246, -125.4636090269712412, 356.7845633553585003 ) ) ;
#19463 = CARTESIAN_POINT ( 'NONE',  ( 787.6308680596127942, -11.26014174441488258, -364.1105419155492768 ) ) ;
#19464 = LINE ( 'NONE', #12543, #31383 ) ;
#19465 = VECTOR ( 'NONE', #33313, 1000.000000000000000 ) ;
#19466 = DIRECTION ( 'NONE',  ( -0.000000000000000000, 1.000000000000000000, -0.000000000000000000 ) ) ;
#19467 = CARTESIAN_POINT ( 'NONE',  ( 765.0180583372156207, -408.9982390220556567, 360.0135310231089534 ) ) ;
#19468 = ORIENTED_EDGE ( 'NONE', *, *, #19642, .T. ) ;
#19469 = CARTESIAN_POINT ( 'NONE',  ( 802.7791456095903868, -340.7146871989592114, -329.0155153010375102 ) ) ;
#19471 = CARTESIAN_POINT ( 'NONE',  ( 785.3687786644885591, -155.3618753856927697, 315.3201227861280813 ) ) ;
#19470 = CARTESIAN_POINT ( 'NONE',  ( 756.5762568750052424, -171.1800572038745543, 348.7366044899774238 ) ) ;
#19472 = UNCERTAINTY_MEASURE_WITH_UNIT (LENGTH_MEASURE( 1.000000000000000082E-05 ), #1202, 'distance_accuracy_value', 'NONE');
#19473 = CARTESIAN_POINT ( 'NONE',  ( 814.8230680027162407, -341.8055962898683333, -333.7305795820267917 ) ) ;
#19474 = CARTESIAN_POINT ( 'NONE',  ( 769.9999999999992042, 205.0000000000000568, -339.9999999999999432 ) ) ;
#19475 = ORIENTED_EDGE ( 'NONE', *, *, #35991, .T. ) ;
#19476 = CARTESIAN_POINT ( 'NONE',  ( 804.9363028652555840, -352.2709662947830225, 338.2165204200192079 ) ) ;
#19477 = EDGE_LOOP ( 'NONE', ( #37500, #13218, #32764, #35395 ) ) ;
#19478 = CARTESIAN_POINT ( 'NONE',  ( 782.5225473063381969, -190.2709662947835909, -375.2698199232970637 ) ) ;
#19479 = B_SPLINE_CURVE_WITH_KNOTS ( 'NONE', 3,
 ( #5467, #41048, #30189, #37109 ),
 .UNSPECIFIED., .F., .F.,
 ( 4, 4 ),
 ( 0.03659475354221209537, 0.03709560045499031566 ),
 .UNSPECIFIED. ) ;
#19480 = CARTESIAN_POINT ( 'NONE',  ( 745.0891759886404770, -124.2709662947837899, 342.4968714119734159 ) ) ;
#19481 = ORIENTED_EDGE ( 'NONE', *, *, #13445, .F. ) ;
#19482 = CARTESIAN_POINT ( 'NONE',  ( 762.1405469898973024, -193.5436935675108714, -357.8594530101016176 ) ) ;
#19483 = AXIS2_PLACEMENT_3D ( 'NONE', #7659, #22404, #39552 ) ;
#19484 = ORIENTED_EDGE ( 'NONE', *, *, #15993, .T. ) ;
#19485 = CARTESIAN_POINT ( 'NONE',  ( 766.9102291470427417, -450.5545181178793541, -318.6633372737382501 ) ) ;
#19486 = CARTESIAN_POINT ( 'NONE',  ( 811.0346526505616112, -254.6346026584196238, 323.0537975583477532 ) ) ;
#19487 = CARTESIAN_POINT ( 'NONE',  ( 786.6156483768007774, -145.4419599262326699, 315.5913626894246136 ) ) ;
#19489 = DIRECTION ( 'NONE',  ( -1.000000000000000000, -0.000000000000000000, -0.000000000000000000 ) ) ;
#19488 = PLANE ( 'NONE',  #12990 ) ;
#19490 = ORIENTED_EDGE ( 'NONE', *, *, #22946, .F. ) ;
#19491 = CARTESIAN_POINT ( 'NONE',  ( 783.0745993439762742, -416.1908817542430938, -365.1016975059196739 ) ) ;
#19492 = DIRECTION ( 'NONE',  ( 0.000000000000000000, -0.000000000000000000, 1.000000000000000000 ) ) ;
#19493 = EDGE_LOOP ( 'NONE', ( #6072, #16530, #35913, #5857 ) ) ;
#19494 = CARTESIAN_POINT ( 'NONE',  ( 771.3260364891663130, -211.6454272087891582, -306.0683387631859773 ) ) ;
#19495 = CARTESIAN_POINT ( 'NONE',  ( 807.2620300519052989, -96.00906357242585898, 318.0141637701419768 ) ) ;
#19496 = VECTOR ( 'NONE', #18271, 1000.000000000000000 ) ;
#19498 = CARTESIAN_POINT ( 'NONE',  ( 758.0580252608178853, -198.4527844766017495, -328.0187753319985404 ) ) ;
#19497 = CARTESIAN_POINT ( 'NONE',  ( 911.9749999999993406, 219.9999999999998863, -360.0000000000000000 ) ) ;
#19499 = CARTESIAN_POINT ( 'NONE',  ( 789.9200121543843807, -361.9874144716864635, -317.0176451133914384 ) ) ;
#19500 = DIRECTION ( 'NONE',  ( 1.000000000000000000, 0.000000000000000000, 0.000000000000000000 ) ) ;
#19501 = CARTESIAN_POINT ( 'NONE',  ( 793.5525998758768083, -223.0999726633346256, -372.6845335610516941 ) ) ;
#19502 = CARTESIAN_POINT ( 'NONE',  ( 791.4716058693660443, -452.9681489794448339, 367.7200696026887954 ) ) ;
#19503 = DIRECTION ( 'NONE',  ( -0.000000000000000000, 1.000000000000000000, -0.000000000000000000 ) ) ;
#19504 = CARTESIAN_POINT ( 'NONE',  ( 754.7162404726377645, -62.73633629969871350, -339.4709603349214717 ) ) ;
#19505 = CARTESIAN_POINT ( 'NONE',  ( 760.7433823573367135, -420.0090635724249069, 355.9930595647440441 ) ) ;
#19506 = CARTESIAN_POINT ( 'NONE',  ( 809.0717654672305343, -364.9181544815158986, 360.1688906516309885 ) ) ;
#19507 = CARTESIAN_POINT ( 'NONE',  ( 747.2067596250078623, -243.1800572038743269, -352.2312462859687230 ) ) ;
#19508 = LINE ( 'NONE', #1718, #14330 ) ;
#19509 = CARTESIAN_POINT ( 'NONE',  ( 959.5497976682736407, 239.9999999999998863, -2132.806278688367456 ) ) ;
#19510 = CARTESIAN_POINT ( 'NONE',  ( 768.0187753319979720, -32.63460265842044095, -318.0580252608186242 ) ) ;
#19511 = CARTESIAN_POINT ( 'NONE',  ( 793.5525998758768083, -175.0999726633346825, 372.6845335610516941 ) ) ;
#19512 = CARTESIAN_POINT ( 'NONE',  ( 803.8556311672234642, -129.6237781080508853, -365.6418435158340117 ) ) ;
#19513 = CARTESIAN_POINT ( 'NONE',  ( 811.0346526505616112, -158.6346026584199933, 323.0537975583477532 ) ) ;
#19514 = CARTESIAN_POINT ( 'NONE',  ( 759.0252816721024374, -384.9982390220556567, -368.0189434323527280 ) ) ;
#19515 = LINE ( 'NONE', #22529, #18040 ) ;
#19516 = CIRCLE ( 'NONE', #15162, 7.999999999999896083 ) ;
#19517 = CARTESIAN_POINT ( 'NONE',  ( 804.9363028652555840, -256.2709662947834204, 338.2165204200192079 ) ) ;
#19518 = PRESENTATION_LAYER_ASSIGNMENT (  '', '', ( #43147 ) ) ;
#19519 = CARTESIAN_POINT ( 'NONE',  ( 772.4468031744293057, -33.82724539060788516, 363.8651313633793620 ) ) ;
#19520 = CARTESIAN_POINT ( 'NONE',  ( 755.5713283507202505, -389.3618753856919739, -334.6858677611754729 ) ) ;
#19521 = AXIS2_PLACEMENT_3D ( 'NONE', #11640, #4479, #18793 ) ;
#19522 = CARTESIAN_POINT ( 'NONE',  ( 768.9521613784389729, -9.827245390607961539, -373.2346286133773106 ) ) ;
#19523 = CARTESIAN_POINT ( 'NONE',  ( 355.8971257818259915, 290.0000000000001137, -244.9999999999999716 ) ) ;
#19524 = CARTESIAN_POINT ( 'NONE',  ( 763.2154366446407039, -93.62377810805098477, 321.4292242960311228 ) ) ;
#19525 = VERTEX_POINT ( 'NONE', #10102 ) ;
#19526 = ADVANCED_FACE ( 'NONE', ( #27416 ), #24396, .T. ) ;
#19527 = CARTESIAN_POINT ( 'NONE',  ( 804.9511171171677688, -221.8055962898687881, -335.8780910478229202 ) ) ;
#19528 = CARTESIAN_POINT ( 'NONE',  ( 755.0636971347428243, -76.27096629478394618, 341.7834795799807353 ) ) ;
#19529 = CARTESIAN_POINT ( 'NONE',  ( 758.0141637701419768, -231.0783235625960401, -367.2620300519063790 ) ) ;
#19530 = CARTESIAN_POINT ( 'NONE',  ( 441.1634899080286232, 259.9999999999999432, -206.1189999999972144 ) ) ;
#19531 = CARTESIAN_POINT ( 'NONE',  ( 808.7758568127978833, -364.1692326535046504, 320.0363995740631822 ) ) ;
#19532 = EDGE_LOOP ( 'NONE', ( #3308, #15478, #25696, #35993, #44471, #32801, #43967, #37037 ) ) ;
#19533 = AXIS2_PLACEMENT_3D ( 'NONE', #168, #14040, #21190 ) ;
#19534 = CARTESIAN_POINT ( 'NONE',  ( 771.2368401574024119, -421.4419599262317888, 374.2805881961240857 ) ) ;
#19535 = CARTESIAN_POINT ( 'NONE',  ( 758.6633372737375112, -20.53286901714212931, -326.9102291470432533 ) ) ;
#19536 = CARTESIAN_POINT ( 'NONE',  ( 762.1405469898971887, -169.5436935675108430, -357.8594530101015607 ) ) ;
#19537 = CARTESIAN_POINT ( 'NONE',  ( 800.0135310231082713, -374.0891481129647786, 325.0180583372163028 ) ) ;
#19538 = VECTOR ( 'NONE', #40283, 1000.000000000000000 ) ;
#19539 = CARTESIAN_POINT ( 'NONE',  ( 805.0032342141412300, -85.54369356751118403, -314.9967657858571783 ) ) ;
#19540 = CARTESIAN_POINT ( 'NONE',  ( 758.0580252608178853, -78.45278447660211896, -328.0187753319985404 ) ) ;
#19541 = VERTEX_POINT ( 'NONE', #13117 ) ;
#19542 = CARTESIAN_POINT ( 'NONE',  ( 793.0897708529556667, -6.554518117880697048, -361.3366627262616362 ) ) ;
#19543 = VERTEX_POINT ( 'NONE', #17251 ) ;
#19544 = CARTESIAN_POINT ( 'NONE',  ( 786.5483106153019435, -367.6454272087886466, -364.1601925771022366 ) ) ;
#19546 = CARTESIAN_POINT ( 'NONE',  ( 786.5483106153019435, -391.6454272087885897, 364.1601925771022366 ) ) ;
#19545 = CARTESIAN_POINT ( 'NONE',  ( 800.2193346964447755, -90.99823902205663728, 355.1360043628815788 ) ) ;
#19549 = CARTESIAN_POINT ( 'NONE',  ( 810.1134526219336749, -320.5328690171411949, 357.8822607201570349 ) ) ;
#19548 = PLANE ( 'NONE',  #24733 ) ;
#19547 = CARTESIAN_POINT ( 'NONE',  ( 751.6929314249750860, -438.9982390220554294, 318.8095938919659034 ) ) ;
#19550 = CIRCLE ( 'NONE', #23234, 10.00000000000000888 ) ;
#19551 = CARTESIAN_POINT ( 'NONE',  ( 751.2241431872005251, -112.1692326535054889, 359.9636004259367610 ) ) ;
#19552 = CARTESIAN_POINT ( 'NONE',  ( 773.4516893846965786, -331.6454272087888171, -315.8398074228977066 ) ) ;
#19553 = CARTESIAN_POINT ( 'NONE',  ( 785.3141322388236176, -309.7255117493287457, -364.4286716492789537 ) ) ;
#19554 = CARTESIAN_POINT ( 'NONE',  ( 805.1927285166397041, -136.8164208402382371, -341.8018195045277707 ) ) ;
#19555 = VECTOR ( 'NONE', #26789, 1000.000000000000000 ) ;
#19556 = CARTESIAN_POINT ( 'NONE',  ( 745.7194118038753459, -13.64542720878976390, 348.7631598425976449 ) ) ;
#19557 = VECTOR ( 'NONE', #26558, 1000.000000000000000 ) ;
#19559 = PLANE ( 'NONE',  #1243 ) ;
#19558 = CARTESIAN_POINT ( 'NONE',  ( 786.4999999999993179, -513.1383975375929367, -369.9999999999999432 ) ) ;
#19560 = CARTESIAN_POINT ( 'NONE',  ( 793.2243759319678702, -266.5328690171413655, -318.4439275373583200 ) ) ;
#19561 = CARTESIAN_POINT ( 'NONE',  ( 745.5313806188320314, -135.2817908451530116, -333.7943932421247268 ) ) ;
#19562 = CARTESIAN_POINT ( 'NONE',  ( -858.8365100919713768, 260.0000000000002274, -199.9999999999881481 ) ) ;
#19563 = DIRECTION ( 'NONE',  ( 1.000000000000000000, 0.000000000000000000, 0.000000000000000000 ) ) ;
#19564 = CARTESIAN_POINT ( 'NONE',  ( 780.5236548040995785, -284.7363362996979390, 314.9735926884559944 ) ) ;
#19565 = ORIENTED_EDGE ( 'NONE', *, *, #7216, .T. ) ;
#19566 = CARTESIAN_POINT ( 'NONE',  ( 762.1177392798416577, -282.5545181178798657, 309.8865473780659272 ) ) ;
#19567 = VECTOR ( 'NONE', #26553, 1000.000000000000000 ) ;
#19568 = CARTESIAN_POINT ( 'NONE',  ( 777.4774526936600978, -154.2709662947836762, -304.7301800767028226 ) ) ;
#19569 = DIRECTION ( 'NONE',  ( -0.000000000000000000, 1.000000000000000000, -0.000000000000000000 ) ) ;
#19570 = AXIS2_PLACEMENT_3D ( 'NONE', #4101, #32272, #11713 ) ;
#19571 = CARTESIAN_POINT ( 'NONE',  ( 807.2620300519052989, -72.00906357242594424, 318.0141637701419768 ) ) ;
#19572 = CARTESIAN_POINT ( 'NONE',  ( 808.0189434323515343, -254.0891481129652334, -319.0252816721025511 ) ) ;
#19573 = VECTOR ( 'NONE', #11655, 999.9999999999998863 ) ;
#19574 = EDGE_CURVE ( 'NONE', #33292, #14459, #7067, .T. ) ;
#19575 = FACE_OUTER_BOUND ( 'NONE', #7829, .T. ) ;
#19576 = CARTESIAN_POINT ( 'NONE',  ( 791.9812246680005501, -164.6346026584200217, 361.9419747391813189 ) ) ;
#19577 = VERTEX_POINT ( 'NONE', #38055 ) ;
#19578 = CARTESIAN_POINT ( 'NONE',  ( 744.9990715423526808, -354.3510508353228943, -341.2370466360926002 ) ) ;
#19579 = CARTESIAN_POINT ( 'NONE',  ( 772.4837098697144029, -95.36187538569294020, -374.5518280994205611 ) ) ;
#19580 = CARTESIAN_POINT ( 'NONE',  ( 793.9708237608222134, -22.91815448151701062, 319.2295555964448681 ) ) ;
#19581 = CARTESIAN_POINT ( 'NONE',  ( 759.0252816721024374, -336.9982390220558273, -368.0189434323527280 ) ) ;
#19582 = CARTESIAN_POINT ( 'NONE',  ( 919.9999999999993179, 154.9999999999998863, 350.0000000000000000 ) ) ;
#19583 = CARTESIAN_POINT ( 'NONE',  ( 805.1016975059191054, -414.8965053807771710, 343.0745993439771837 ) ) ;
#19584 = ORIENTED_EDGE ( 'NONE', *, *, #14562, .T. ) ;
#19585 = ADVANCED_FACE ( 'NONE', ( #41059 ), #5939, .F. ) ;
#19586 = CARTESIAN_POINT ( 'NONE',  ( 759.8311093483677041, -118.1692326535054463, -310.9282345327691814 ) ) ;
#19587 = CARTESIAN_POINT ( 'NONE',  ( -37.63011601220122770, -513.1383975375929367, -367.9999999999999432 ) ) ;
#19588 = CARTESIAN_POINT ( 'NONE',  ( 803.8556311672234642, -225.6237781080506011, 365.6418435158340117 ) ) ;
#19589 = CARTESIAN_POINT ( 'NONE',  ( 800.0135310231082713, -86.08914811296573077, 325.0180583372163028 ) ) ;
#19590 = VERTEX_POINT ( 'NONE', #20705 ) ;
#19591 = CARTESIAN_POINT ( 'NONE',  ( 796.7845633553578182, -9.623778108051251223, -358.5707757039688204 ) ) ;
#19592 = CARTESIAN_POINT ( 'NONE',  ( 765.0180583372156207, -264.9982390220561115, 360.0135310231089534 ) ) ;
#19593 = AXIS2_PLACEMENT_3D ( 'NONE', #17016, #6838, #41736 ) ;
#19594 = CARTESIAN_POINT ( 'NONE',  ( 748.3538107759620743, -424.7146871989589840, -355.8262568251490165 ) ) ;
#19595 = DIRECTION ( 'NONE',  ( 0.000000000000000000, 0.000000000000000000, 1.000000000000000000 ) ) ;
#19596 = EDGE_CURVE ( 'NONE', #16659, #22935, #24017, .T. ) ;
#19597 = ORIENTED_EDGE ( 'NONE', *, *, #23222, .F. ) ;
#19598 = ORIENTED_EDGE ( 'NONE', *, *, #12322, .F. ) ;
#19599 = CARTESIAN_POINT ( 'NONE',  ( 783.7953271457878373, -392.1908817542432075, -375.1787889125761239 ) ) ;
#19600 = VECTOR ( 'NONE', #36350, 1000.000000000000114 ) ;
#19601 = EDGE_CURVE ( 'NONE', #38191, #3542, #37749, .T. ) ;
#19602 = CARTESIAN_POINT ( 'NONE',  ( 792.1044303154645831, -228.4527844766015789, -317.8323909638837677 ) ) ;
#19604 = CARTESIAN_POINT ( 'NONE',  ( 795.6651683502461765, -226.7146871989596661, 371.3240766477733814 ) ) ;
#19603 = CARTESIAN_POINT ( 'NONE',  ( 805.0032342141413437, -325.5436935675104451, 314.9967657858572352 ) ) ;
#19605 = CARTESIAN_POINT ( 'NONE',  ( 798.0661480581538854, -50.53286901714203339, 309.5768839229118043 ) ) ;
#19606 = CARTESIAN_POINT ( 'NONE',  ( 793.9708237608222134, -214.9181544815164386, -319.2295555964448681 ) ) ;
#19607 = CARTESIAN_POINT ( 'NONE',  ( 805.1927285166397041, -208.8164208402380666, -341.8018195045277707 ) ) ;
#19608 = CARTESIAN_POINT ( 'NONE',  ( 768.0187753319979720, -416.6346026584192259, -318.0580252608186242 ) ) ;
#19609 = VERTEX_POINT ( 'NONE', #6851 ) ;
#19610 = CARTESIAN_POINT ( 'NONE',  ( 802.1676090361156639, -206.6346026584198512, 327.8955696845344505 ) ) ;
#19611 = CARTESIAN_POINT ( 'NONE',  ( 759.7806653035534055, -102.9982390220565520, -324.8639956371180801 ) ) ;
#19612 = ORIENTED_EDGE ( 'NONE', *, *, #9941, .F. ) ;
#19613 = CARTESIAN_POINT ( 'NONE',  ( 814.5518280994195948, -327.7255117493285184, 332.4837098697145734 ) ) ;
#19614 = DIRECTION ( 'NONE',  ( -0.000000000000000000, -0.000000000000000000, 1.000000000000000000 ) ) ;
#19615 = DIRECTION ( 'NONE',  ( 0.000000000000000000, -1.000000000000000000, 0.000000000000000000 ) ) ;
#19616 = CYLINDRICAL_SURFACE ( 'NONE', #38521, 10.00000000000000888 ) ;
#19617 = CARTESIAN_POINT ( 'NONE',  ( 790.9844846989617508, -190.3726999360619629, 317.2208543904092721 ) ) ;
#19618 = CARTESIAN_POINT ( 'NONE',  ( 795.1360043628807261, -68.08914811296575920, 360.2193346964456282 ) ) ;
#19619 = ORIENTED_EDGE ( 'NONE', *, *, #15065, .F. ) ;
#19620 = CARTESIAN_POINT ( 'NONE',  ( 755.8990559732751535, -443.4636090269702322, -365.9055244015606831 ) ) ;
#19621 = CARTESIAN_POINT ( 'NONE',  ( 787.4397851343537695, -21.72551174932956641, -374.2001403089903988 ) ) ;
#19622 = CARTESIAN_POINT ( 'NONE',  ( 805.0264073115434940, -246.3510508353232638, 339.4763451958999099 ) ) ;
#19623 = CIRCLE ( 'NONE', #38073, 30.00000000000008171 ) ;
#19624 = CARTESIAN_POINT ( 'NONE',  ( 791.9812246680005501, -380.6346026584192828, -361.9419747391813189 ) ) ;
#19625 = CARTESIAN_POINT ( 'NONE',  ( 802.1676090361155502, -14.63460265842049779, -327.8955696845344505 ) ) ;
#19626 = EDGE_CURVE ( 'NONE', #16198, #41554, #27197, .T. ) ;
#19627 = CARTESIAN_POINT ( 'NONE',  ( 772.5602148656447525, -441.7255117493282910, 305.7998596910095443 ) ) ;
#19628 = DIRECTION ( 'NONE',  ( 0.000000000000000000, 0.000000000000000000, 1.000000000000000000 ) ) ;
#19629 = CARTESIAN_POINT ( 'NONE',  ( 776.9254006560222479, -284.1908817542434917, -314.8983024940802125 ) ) ;
#19630 = CARTESIAN_POINT ( 'NONE',  ( 745.0891759886404770, -148.2709662947837330, -342.4968714119734159 ) ) ;
#19631 = EDGE_CURVE ( 'NONE', #22578, #25515, #23485, .T. ) ;
#19632 = CARTESIAN_POINT ( 'NONE',  ( 814.2001403089898304, -89.36187538569299704, 347.4397851343538264 ) ) ;
#19633 = CARTESIAN_POINT ( 'NONE',  ( 814.5518280994195948, -135.7255117493291152, 332.4837098697145734 ) ) ;
#19634 = CARTESIAN_POINT ( 'NONE',  ( 781.4876528434626834, 16.45630643248849267, -313.8857452882203347 ) ) ;
#19635 = DIRECTION ( 'NONE',  ( 0.000000000000000000, 0.000000000000000000, 1.000000000000000000 ) ) ;
#19636 = VECTOR ( 'NONE', #37599, 999.9999999999998863 ) ;
#19637 = DIRECTION ( 'NONE',  ( 0.000000000000000000, 0.000000000000000000, 1.000000000000000000 ) ) ;
#19638 = CARTESIAN_POINT ( 'NONE',  ( 745.4481719005789273, -363.7255117493284047, 347.5162901302853129 ) ) ;
#19639 = CARTESIAN_POINT ( 'NONE',  ( 796.7737145352015204, 3.365397341579444479, 370.7187646348536987 ) ) ;
#19640 = CARTESIAN_POINT ( 'NONE',  ( 762.1405469898971887, -361.5436935675103882, -357.8594530101015607 ) ) ;
#19641 = VECTOR ( 'NONE', #24213, 1000.000000000000000 ) ;
#19642 = EDGE_CURVE ( 'NONE', #11789, #14175, #20931, .T. ) ;
#19643 = CARTESIAN_POINT ( 'NONE',  ( 791.9812246680005501, -452.6346026584191691, 361.9419747391813189 ) ) ;
#19644 = CARTESIAN_POINT ( 'NONE',  ( 752.7379699480933368, -108.0090635724258448, -361.9858362298580232 ) ) ;
#19645 = CARTESIAN_POINT ( 'NONE',  ( 758.6633372737375112, -164.5328690171416781, -326.9102291470432533 ) ) ;
#19646 = CARTESIAN_POINT ( 'NONE',  ( 815.1787889125755555, -150.8965053807781089, 343.7953271457877804 ) ) ;
#19647 = CARTESIAN_POINT ( 'NONE',  ( 791.9812246680005501, 3.365397341579444479, 361.9419747391813189 ) ) ;
#19648 = CARTESIAN_POINT ( 'NONE',  ( 798.0661480581538854, -170.5328690171416781, 309.5768839229118043 ) ) ;
#19649 = CARTESIAN_POINT ( 'NONE',  ( 785.3141322388236176, -21.72551174932956641, -364.4286716492789537 ) ) ;
#19650 = CARTESIAN_POINT ( 'NONE',  ( 784.0799538623451781, -179.8055962898688733, -364.6971507214555572 ) ) ;
#19651 = CARTESIAN_POINT ( 'NONE',  ( 762.1405469898971887, -145.5436935675109851, 357.8594530101015607 ) ) ;
#19652 = CARTESIAN_POINT ( 'NONE',  ( 755.0488828828309806, -425.8055962898680491, -344.1219089521771934 ) ) ;
#19654 = CARTESIAN_POINT ( 'NONE',  ( 801.9419747391806368, -282.4527844766014937, 351.9812246680014027 ) ) ;
#19653 = CARTESIAN_POINT ( 'NONE',  ( 797.6776695296629214, -283.5436935675105019, 357.6776695296636603 ) ) ;
#19655 = LINE ( 'NONE', #12717, #5726 ) ;
#19656 = ORIENTED_EDGE ( 'NONE', *, *, #27209, .T. ) ;
#19657 = CARTESIAN_POINT ( 'NONE',  ( 789.5670355615794733, -453.0432664090020012, 363.0970091259334822 ) ) ;
#19658 = CARTESIAN_POINT ( 'NONE',  ( 747.6481478633932056, -277.0999726633344267, -353.4146539503763620 ) ) ;
#19659 = VERTEX_POINT ( 'NONE', #37817 ) ;
#19660 = VECTOR ( 'NONE', #19846, 1000.000000000000000 ) ;
#19661 = CARTESIAN_POINT ( 'NONE',  ( 751.6929314249750860, -222.9982390220561683, 318.8095938919659034 ) ) ;
#19662 = CARTESIAN_POINT ( 'NONE',  ( 802.5472867521000353, -316.3726999360615082, 350.8726784830461156 ) ) ;
#19663 = CARTESIAN_POINT ( 'NONE',  ( 770.0799878456142551, -397.9874144716864066, 362.9823548866085616 ) ) ;
#19664 = ORIENTED_EDGE ( 'NONE', *, *, #13394, .T. ) ;
#19665 = CARTESIAN_POINT ( 'NONE',  ( 786.5483106153019435, -103.6454272087894850, -364.1601925771022366 ) ) ;
#19666 = CARTESIAN_POINT ( 'NONE',  ( 801.9419747391806368, -114.4527844766020053, -351.9812246680014027 ) ) ;
#19667 = CARTESIAN_POINT ( 'NONE',  ( 797.8594530101009923, -277.5436935675105588, -322.1405469898982119 ) ) ;
#19668 = ORIENTED_EDGE ( 'NONE', *, *, #15648, .T. ) ;
#19669 = CARTESIAN_POINT ( 'NONE',  ( 797.8594530101008786, -421.5436935675101040, -322.1405469898980982 ) ) ;
#19670 = CARTESIAN_POINT ( 'NONE',  ( 756.5762568750052424, -75.18005720387485269, -348.7366044899774238 ) ) ;
#19671 = CIRCLE ( 'NONE', #6432, 2.749999999999808153 ) ;
#19672 = CARTESIAN_POINT ( 'NONE',  ( 756.1348686366196716, -305.2601417444139429, 347.5531968255698416 ) ) ;
#19673 = FACE_OUTER_BOUND ( 'NONE', #12915, .T. ) ;
#19674 = DIRECTION ( 'NONE',  ( -0.000000000000000000, -1.110223024625155554E-15, 1.000000000000000000 ) ) ;
#19675 = VECTOR ( 'NONE', #9850, 1000.000000000000000 ) ;
#19676 = CARTESIAN_POINT ( 'NONE',  ( 989.9999999999992042, 249.9999999999998863, 360.0000000000000000 ) ) ;
#19677 = VERTEX_POINT ( 'NONE', #17498 ) ;
#19678 = CARTESIAN_POINT ( 'NONE',  ( 773.7305795820266212, -345.2817908451523863, -374.8230680027170365 ) ) ;
#19679 = CARTESIAN_POINT ( 'NONE',  ( 771.3260364891663130, -211.6454272087891582, 306.0683387631859773 ) ) ;
#19681 = CARTESIAN_POINT ( 'NONE',  ( 771.1735550268778070, -297.1800572038740711, -316.3353852180827630 ) ) ;
#19680 = FACE_BOUND ( 'NONE', #30172, .T. ) ;
#19682 = EDGE_CURVE ( 'NONE', #23400, #16465, #12877, .T. ) ;
#19683 = LINE ( 'NONE', #4919, #3054 ) ;
#19684 = CARTESIAN_POINT ( 'NONE',  ( 761.4292242960306112, -185.4636090269710280, -323.2154366446414429 ) ) ;
#19685 = CARTESIAN_POINT ( 'NONE',  ( 767.6429770376289525, -33.18005720387498769, 306.8695393053162093 ) ) ;
#19686 = CARTESIAN_POINT ( 'NONE',  ( -521.6730038022808458, 240.0000000000001705, 350.0000000000000000 ) ) ;
#19687 = CARTESIAN_POINT ( 'NONE',  ( 792.3570229623691148, -381.1800572038739006, -373.1304606946836770 ) ) ;
#19688 = PRESENTATION_STYLE_ASSIGNMENT (( #22694 ) ) ;
#19689 = CARTESIAN_POINT ( 'NONE',  ( 785.3687786644884454, -35.36187538569316047, 315.3201227861279676 ) ) ;
#19690 = AXIS2_PLACEMENT_3D ( 'NONE', #442, #28845, #4148 ) ;
#19691 = CARTESIAN_POINT ( 'NONE',  ( 744.6391490659812007, -326.7363362996979390, 338.7502325331110455 ) ) ;
#19692 = CARTESIAN_POINT ( 'NONE',  ( 754.9967657858570647, -241.5436935675106156, 365.0032342141425374 ) ) ;
#19693 = CARTESIAN_POINT ( 'NONE',  ( 777.4774526936600978, -10.27096629478414691, -304.7301800767027657 ) ) ;
#19694 = AXIS2_PLACEMENT_3D ( 'NONE', #4363, #26029, #36676 ) ;
#19695 = ADVANCED_FACE ( 'NONE', ( #37585 ), #6412, .F. ) ;
#19696 = CARTESIAN_POINT ( 'NONE',  ( 800.2193346964447755, -234.9982390220561683, -355.1360043628815788 ) ) ;
#19697 = LINE ( 'NONE', #30306, #339 ) ;
#19698 = CARTESIAN_POINT ( 'NONE',  ( 754.8072714833581358, -364.8164208402374697, 338.1981804954720587 ) ) ;
#19699 = CARTESIAN_POINT ( 'NONE',  ( 759.0159684113467620, -136.9181544815166376, 325.8855110935213020 ) ) ;
#19700 = CARTESIAN_POINT ( 'NONE',  ( 769.1273215169530886, -22.71468719896029853, -317.4527132478988847 ) ) ;
#19701 = CARTESIAN_POINT ( 'NONE',  ( 759.9864689768902508, -386.0891481129647786, 354.9819416627836404 ) ) ;
#19702 = AXIS2_PLACEMENT_3D ( 'NONE', #39853, #4283, #24823 ) ;
#19703 = CARTESIAN_POINT ( 'NONE',  ( 767.9999999999992042, 205.0000000000000568, -350.0000000000000000 ) ) ;
#19704 = CARTESIAN_POINT ( 'NONE',  ( 914.9999999999992042, 99.99999999999984368, -360.0000000000000000 ) ) ;
#19705 = CARTESIAN_POINT ( 'NONE',  ( 813.2346286133761168, -125.2601417444145255, 328.9521613784389160 ) ) ;
#19706 = CARTESIAN_POINT ( 'NONE',  ( 800.0135310231082713, -398.0891481129647218, 325.0180583372163028 ) ) ;
#19707 = EDGE_LOOP ( 'NONE', ( #16088, #42794, #21819, #4241 ) ) ;
#19708 = CARTESIAN_POINT ( 'NONE',  ( 785.3141322388236176, -45.72551174932949181, -364.4286716492789537 ) ) ;
#19709 = CIRCLE ( 'NONE', #10858, 7.999999999999896083 ) ;
#19710 = CARTESIAN_POINT ( 'NONE',  ( 766.7756240680305382, -326.5328690171411381, -361.5560724626415663 ) ) ;
#19712 = CARTESIAN_POINT ( 'NONE',  ( 767.8955696845334842, -144.4527844766018632, 362.1676090361161755 ) ) ;
#19711 = CARTESIAN_POINT ( 'NONE',  ( 797.8594530101008786, -181.5436935675108145, 322.1405469898980982 ) ) ;
#19713 = CARTESIAN_POINT ( 'NONE',  ( 807.5423716828161105, -369.0783235625956422, -362.2119215644372048 ) ) ;
#19714 = CARTESIAN_POINT ( 'NONE',  ( 919.9999999999993179, 219.9999999999998863, 360.0000000000000000 ) ) ;
#19715 = EDGE_LOOP ( 'NONE', ( #17871, #354, #25476, #38717 ) ) ;
#19716 = CARTESIAN_POINT ( 'NONE',  ( 797.6776695296629214, -355.5436935675103882, 357.6776695296636603 ) ) ;
#19717 = ORIENTED_EDGE ( 'NONE', *, *, #45675, .F. ) ;
#19718 = CARTESIAN_POINT ( 'NONE',  ( 746.8695393053150156, -197.9073299311472169, -327.6429770376306010 ) ) ;
#19719 = CARTESIAN_POINT ( 'NONE',  ( 814.2001403089898304, -113.3618753856929260, 347.4397851343538264 ) ) ;
#19720 = ORIENTED_EDGE ( 'NONE', *, *, #7197, .F. ) ;
#19721 = CARTESIAN_POINT ( 'NONE',  ( 771.1735550268780344, -177.1800572038744974, -316.3353852180828198 ) ) ;
#19722 = ORIENTED_EDGE ( 'NONE', *, *, #2930, .T. ) ;
#19723 = CARTESIAN_POINT ( 'NONE',  ( 795.1360043628807261, -332.0891481129649492, -360.2193346964456282 ) ) ;
#19724 = CARTESIAN_POINT ( 'NONE',  ( 759.0159684113467620, -448.9181544815156144, -325.8855110935213020 ) ) ;
#19725 = CARTESIAN_POINT ( 'NONE',  ( 808.3070685750230950, -258.9982390220561115, 361.1904061080339261 ) ) ;
#19726 = CARTESIAN_POINT ( 'NONE',  ( 763.2154366446407039, -189.6237781080507148, 321.4292242960311228 ) ) ;
#19728 = DIRECTION ( 'NONE',  ( 0.000000000000000000, 0.000000000000000000, 1.000000000000000000 ) ) ;
#19727 = CARTESIAN_POINT ( 'NONE',  ( 779.9999999999992042, 16.45630643248849267, -370.0000000000000568 ) ) ;
#19729 = CARTESIAN_POINT ( 'NONE',  ( -789.9999999999992042, 205.0000000000000568, -339.9999999999999432 ) ) ;
#19730 = EDGE_LOOP ( 'NONE', ( #39388, #29439, #15694, #38516, #22168, #22496 ) ) ;
#19731 = CARTESIAN_POINT ( 'NONE',  ( 802.5472867521000353, -412.3726999360612808, -350.8726784830461156 ) ) ;
#19732 = LINE ( 'NONE', #20410, #412 ) ;
#19733 = CARTESIAN_POINT ( 'NONE',  ( -338.8365100919713200, 260.0000000000001137, -208.0249999999917918 ) ) ;
#19734 = VERTEX_POINT ( 'NONE', #6166 ) ;
#19735 = CARTESIAN_POINT ( 'NONE',  ( 805.6418435158337843, -221.4636090269709428, -363.8556311672236916 ) ) ;
#19736 = CARTESIAN_POINT ( 'NONE',  ( 804.1009440267234822, -95.46360902697132644, 314.0944755984392600 ) ) ;
#19737 = VECTOR ( 'NONE', #23097, 1000.000000000000114 ) ;
#19739 = CARTESIAN_POINT ( 'NONE',  ( 771.2633955100217236, -191.9073299311471885, -363.4237431249939618 ) ) ;
#19738 = PLANE ( 'NONE',  #9394 ) ;
#19740 = CARTESIAN_POINT ( 'NONE',  ( 803.2186876482843445, -367.9874144716865203, -350.0220218866286928 ) ) ;
#19741 = DIRECTION ( 'NONE',  ( 1.000000000000000000, 0.000000000000000000, 0.000000000000000000 ) ) ;
#19742 = CARTESIAN_POINT ( 'NONE',  ( 778.7629533639073998, -224.7363362996982232, -375.0009284576466371 ) ) ;
#19743 = DIRECTION ( 'NONE',  ( -0.000000000000000000, 1.000000000000000000, -0.000000000000000000 ) ) ;
#19744 = LINE ( 'NONE', #6339, #26766 ) ;
#19745 = CARTESIAN_POINT ( 'NONE',  ( 805.2837595273609850, -98.73633629969859271, -340.5290396650784714 ) ) ;
#19746 = CARTESIAN_POINT ( 'NONE',  ( 773.4516893846965786, -427.6454272087885897, 315.8398074228977066 ) ) ;
#19747 = CARTESIAN_POINT ( 'NONE',  ( -338.8365100919713200, 260.0000000000001137, -206.1189999999917859 ) ) ;
#19748 = CARTESIAN_POINT ( 'NONE',  ( 805.1016975059191054, -414.8965053807771710, -343.0745993439771837 ) ) ;
#19749 = CARTESIAN_POINT ( 'NONE',  ( 808.3070685750232087, -282.9982390220559409, -361.1904061080339829 ) ) ;
#19750 = FACE_OUTER_BOUND ( 'NONE', #24909, .T. ) ;
#19751 = CARTESIAN_POINT ( 'NONE',  ( -37.63011601220122770, -857.0166862835568509, -63.94525337997358605 ) ) ;
#19752 = CARTESIAN_POINT ( 'NONE',  ( 794.9819416627830151, -60.99823902205671544, -319.9864689768909898 ) ) ;
#19753 = CARTESIAN_POINT ( 'NONE',  ( 815.3608509340175488, -218.7363362996982232, 341.2497674668889545 ) ) ;
#19754 = CARTESIAN_POINT ( 'NONE',  ( 788.7631598425961101, -169.4419599262325562, -305.7194118038759143 ) ) ;
#19755 = CARTESIAN_POINT ( 'NONE',  ( 767.7687537140311633, -167.9073299311473022, 372.7932403749916830 ) ) ;
#19756 = CARTESIAN_POINT ( 'NONE',  ( 808.0189434323515343, -422.0891481129647218, -319.0252816721025511 ) ) ;
#19757 = DIRECTION ( 'NONE',  ( -0.000000000000000000, 1.000000000000000000, -0.000000000000000000 ) ) ;
#19758 = CARTESIAN_POINT ( 'NONE',  ( 758.0580252608178853, -246.4527844766016074, 328.0187753319985404 ) ) ;
#19759 = CARTESIAN_POINT ( 'NONE',  ( 804.4086373105744769, -73.64542720878957027, 333.3843516231986541 ) ) ;
#19760 = CARTESIAN_POINT ( 'NONE',  ( 803.4237431249931660, -375.1800572038739574, -331.2633955100225194 ) ) ;
#19761 = LINE ( 'NONE', #40563, #41682 ) ;
#19762 = CARTESIAN_POINT ( 'NONE',  ( 795.8262568251477660, -46.37269993606239638, -308.3538107759623585 ) ) ;
#19763 = CARTESIAN_POINT ( 'NONE',  ( 759.9999999999992042, -462.9681489794448339, -309.9999999999998863 ) ) ;
#19764 = CARTESIAN_POINT ( 'NONE',  ( 789.9200121543843807, -73.98741447168741558, 317.0176451133914384 ) ) ;
#19765 = ORIENTED_EDGE ( 'NONE', *, *, #18482, .T. ) ;
#19766 = CARTESIAN_POINT ( 'NONE',  ( 784.0799538623451781, -227.8055962898687596, -364.6971507214555572 ) ) ;
#19767 = CARTESIAN_POINT ( 'NONE',  ( 755.3201227861273992, -123.7255117493292147, -345.3687786644892981 ) ) ;
#19768 = CARTESIAN_POINT ( 'NONE',  ( 785.3687786644884454, -59.36187538569306810, 315.3201227861279676 ) ) ;
#19769 = CARTESIAN_POINT ( 'NONE',  ( 781.2497674668890113, -252.3510508353232353, -375.3608509340180603 ) ) ;
#19770 = CARTESIAN_POINT ( 'NONE',  ( 571.1634899080285095, 229.9999999999999432, -197.2499999999982947 ) ) ;
#19771 = CARTESIAN_POINT ( 'NONE',  ( 778.7502325331095108, -384.3510508353227806, 304.6391490659818828 ) ) ;
#19772 = ORIENTED_EDGE ( 'NONE', *, *, #39475, .F. ) ;
#19773 = CIRCLE ( 'NONE', #6515, 8.024999999999948841 ) ;
#19774 = CARTESIAN_POINT ( 'NONE',  ( 810.1134526219336749, -440.5328690171407970, 357.8822607201570349 ) ) ;
#19775 = CARTESIAN_POINT ( 'NONE',  ( 779.4709603349208464, -24.35105083532392811, -314.7162404726379918 ) ) ;
#19776 = CARTESIAN_POINT ( 'NONE',  ( 781.8018195045266339, -166.2709662947835909, -365.1927285166406705 ) ) ;
#19777 = CARTESIAN_POINT ( 'NONE',  ( 781.7834795799800531, -370.8164208402375834, 315.0636971347436202 ) ) ;
#19778 = CARTESIAN_POINT ( 'NONE',  ( 777.4774526936600978, -82.27096629478388934, -304.7301800767027657 ) ) ;
#19779 = CARTESIAN_POINT ( 'NONE',  ( 771.1735550268780344, -57.18005720387490243, -316.3353852180828198 ) ) ;
#19780 = CARTESIAN_POINT ( 'NONE',  ( 793.9708237608222134, 1.081845518482914104, -319.2295555964448681 ) ) ;
#19781 = VERTEX_POINT ( 'NONE', #16580 ) ;
#19782 = CARTESIAN_POINT ( 'NONE',  ( 804.8461984189677878, -338.1908817542433212, -336.9566956441385628 ) ) ;
#19784 = CARTESIAN_POINT ( 'NONE',  ( 796.9571628226829034, -407.4636090269703459, 321.2382568024804641 ) ) ;
#19783 = CARTESIAN_POINT ( 'NONE',  ( 771.1735550268778070, -81.18005720387481006, 316.3353852180827630 ) ) ;
#19785 = CARTESIAN_POINT ( 'NONE',  ( 755.8398074228967971, -91.44195992623282621, 333.4516893846970333 ) ) ;
#19788 = CARTESIAN_POINT ( 'NONE',  ( 786.2056067578752163, -323.8055962898684470, 374.4686193811670023 ) ) ;
#19787 = DIRECTION ( 'NONE',  ( -0.000000000000000000, 0.000000000000000000, 1.000000000000000000 ) ) ;
#19786 = CARTESIAN_POINT ( 'NONE',  ( 815.2698199232962679, -424.8164208402373561, 342.5225473063383674 ) ) ;
#19789 = CARTESIAN_POINT ( 'NONE',  ( 778.7502325331095108, -120.3510508353236048, 304.6391490659818828 ) ) ;
#19790 = CARTESIAN_POINT ( 'NONE',  ( 802.5472867521000353, -316.3726999360615082, -350.8726784830461156 ) ) ;
#19791 = CARTESIAN_POINT ( 'NONE',  ( 759.9864689768902508, -314.0891481129650629, -354.9819416627836404 ) ) ;
#19792 = CARTESIAN_POINT ( 'NONE',  ( 813.5763878283155464, -147.8272453906075157, -351.1614460488615350 ) ) ;
#19793 = CARTESIAN_POINT ( 'NONE',  ( 804.1009440267234822, 0.5363909730283709099, 314.0944755984392600 ) ) ;
#19795 = DIRECTION ( 'NONE',  ( 0.000000000000000000, -0.3826834323650838976, -0.9238795325112892920 ) ) ;
#19794 = DIRECTION ( 'NONE',  ( -0.000000000000000000, 1.000000000000000000, -0.000000000000000000 ) ) ;
#19796 = CARTESIAN_POINT ( 'NONE',  ( 781.2370466360911223, -116.7363362996985217, -304.9990715423533629 ) ) ;
#19797 = CARTESIAN_POINT ( 'NONE',  ( 701.1634899080286232, 239.9999999999999432, -197.2499999999991758 ) ) ;
#19798 = CARTESIAN_POINT ( 'NONE',  ( 911.9749999999993406, 219.9999999999998863, -360.0000000000000000 ) ) ;
#19799 = CARTESIAN_POINT ( 'NONE',  ( 787.5531968255692163, -333.8272453906070041, 316.1348686366205811 ) ) ;
#19800 = CARTESIAN_POINT ( 'NONE',  ( 791.9812246680005501, -188.6346026584199365, 361.9419747391813189 ) ) ;
#19801 = VERTEX_POINT ( 'NONE', #44760 ) ;
#19802 = CARTESIAN_POINT ( 'NONE',  ( 783.7953271457878373, -320.1908817542434349, 375.1787889125761239 ) ) ;
#19803 = CARTESIAN_POINT ( 'NONE',  ( 782.5225473063383106, -166.2709662947836478, -375.2698199232970637 ) ) ;
#19804 = CARTESIAN_POINT ( 'NONE',  ( 799.9999999999993179, -462.9681489794448339, 370.0000000000000568 ) ) ;
#19805 = AXIS2_PLACEMENT_3D ( 'NONE', #20370, #8458, #40097 ) ;
#19806 = CARTESIAN_POINT ( 'NONE',  ( 760.0363995740630116, -106.9181544815167371, 368.7758568127991907 ) ) ;
#19807 = CARTESIAN_POINT ( 'NONE',  ( 767.6429770376289525, -297.1800572038740711, -306.8695393053162093 ) ) ;
#19808 = CARTESIAN_POINT ( 'NONE',  ( 804.7487373415286811, -451.5436935675099903, -364.7487373415288516 ) ) ;
#19809 = CARTESIAN_POINT ( 'NONE',  ( 778.2165204200184689, -166.8164208402382087, 364.9363028652563230 ) ) ;
#19810 = VERTEX_POINT ( 'NONE', #20256 ) ;
#19811 = CARTESIAN_POINT ( 'NONE',  ( 781.2370466360911223, -404.7363362996975980, 304.9990715423533629 ) ) ;
#19812 = CARTESIAN_POINT ( 'NONE',  ( 788.7631598425961101, -337.4419599262319593, -305.7194118038759143 ) ) ;
#19813 = CARTESIAN_POINT ( 'NONE',  ( 814.2001403089898304, -89.36187538569299704, -347.4397851343538264 ) ) ;
#19814 = CARTESIAN_POINT ( 'NONE',  ( 766.0291762391763086, -58.91815448151690759, 360.7704444035551319 ) ) ;
#19815 = CARTESIAN_POINT ( 'NONE',  ( 792.3570229623688874, -381.1800572038737869, -373.1304606946836202 ) ) ;
#19816 = FACE_BOUND ( 'NONE', #32471, .T. ) ;
#19817 = CARTESIAN_POINT ( 'NONE',  ( 763.2154366446407039, -429.6237781080499190, 321.4292242960311228 ) ) ;
#19818 = EDGE_LOOP ( 'NONE', ( #15655, #7929, #20228, #44052 ) ) ;
#19819 = CARTESIAN_POINT ( 'NONE',  ( 803.8651313633788504, -77.26014174441466764, 332.4468031744301015 ) ) ;
#19820 = CARTESIAN_POINT ( 'NONE',  ( 764.3348316497523456, -118.7146871989600072, -308.6759233522265617 ) ) ;
#19821 = CARTESIAN_POINT ( 'NONE',  ( -773.4999999999993179, -110.5936016518799221, 750.6326042729449455 ) ) ;
#19822 = CARTESIAN_POINT ( 'NONE',  ( 786.2056067578752163, -275.8055962898685038, 374.4686193811670023 ) ) ;
#19823 = CARTESIAN_POINT ( 'NONE',  ( 778.1981804954715471, -82.27096629478390355, 314.8072714833591021 ) ) ;
#19824 = VERTEX_POINT ( 'NONE', #2940 ) ;
#19825 = CARTESIAN_POINT ( 'NONE',  ( 763.2154366446407039, 2.376221891948710585, -321.4292242960311228 ) ) ;
#19826 = CARTESIAN_POINT ( 'NONE',  ( 785.3141322388236176, -285.7255117493286889, 364.4286716492789537 ) ) ;
#19827 = CARTESIAN_POINT ( 'NONE',  ( 747.3154664389472828, -427.9874144716862929, -326.4474001241230781 ) ) ;
#19828 = PLANE ( 'NONE',  #1782 ) ;
#19829 = ORIENTED_EDGE ( 'NONE', *, *, #3269, .T. ) ;
#19830 = EDGE_LOOP ( 'NONE', ( #43125, #36485, #15697, #31500 ) ) ;
#19831 = CARTESIAN_POINT ( 'NONE',  ( 752.7379699480933368, -372.0090635724250205, -361.9858362298580232 ) ) ;
#19832 = CIRCLE ( 'NONE', #31609, 10.00000000000000888 ) ;
#19833 = CARTESIAN_POINT ( 'NONE',  ( 804.9363028652555840, -232.2709662947834488, -338.2165204200192079 ) ) ;
#19835 = CARTESIAN_POINT ( 'NONE',  ( 814.8230680027162407, -221.8055962898687881, 333.7305795820267917 ) ) ;
#19834 = CARTESIAN_POINT ( 'NONE',  ( 747.2067596250078623, -315.1800572038740711, 352.2312462859687230 ) ) ;
#19836 = EDGE_CURVE ( 'NONE', #5018, #2958, #37007, .T. ) ;
#19837 = CARTESIAN_POINT ( 'NONE',  ( 755.3028492785439312, -207.2817908451527842, -335.9200461376539693 ) ) ;
#19838 = CARTESIAN_POINT ( 'NONE',  ( 797.6776695296629214, -235.5436935675107293, -357.6776695296636603 ) ) ;
#19839 = CARTESIAN_POINT ( 'NONE',  ( 794.9819416627830151, -420.9982390220555999, -319.9864689768909898 ) ) ;
#19840 = EDGE_LOOP ( 'NONE', ( #38297, #37461, #40719, #34430 ) ) ;
#19841 = CARTESIAN_POINT ( 'NONE',  ( 756.5762568750052424, -195.1800572038744974, 348.7366044899774238 ) ) ;
#19842 = CARTESIAN_POINT ( 'NONE',  ( 803.4237431249931660, -111.1800572038747532, -331.2633955100225194 ) ) ;
#19843 = ORIENTED_EDGE ( 'NONE', *, *, #11308, .F. ) ;
#19844 = CARTESIAN_POINT ( 'NONE',  ( 815.2698199232961542, -352.8164208402374129, 342.5225473063383106 ) ) ;
#19845 = PLANE ( 'NONE',  #8583 ) ;
#19846 = DIRECTION ( 'NONE',  ( -0.000000000000000000, 1.000000000000000000, -0.000000000000000000 ) ) ;
#19847 = DIRECTION ( 'NONE',  ( 1.000000000000000000, -1.880165489482579047E-16, 0.000000000000000000 ) ) ;
#19848 = EDGE_CURVE ( 'NONE', #31800, #27295, #27052, .T. ) ;
#19849 = CARTESIAN_POINT ( 'NONE',  ( 790.0220218866281812, -223.0999726633346256, 363.2186876482849129 ) ) ;
#19850 = ADVANCED_FACE ( 'NONE', ( #27641 ), #35262, .F. ) ;
#19851 = CARTESIAN_POINT ( 'NONE',  ( 804.4286716492782716, -89.36187538569299704, 345.3141322388244703 ) ) ;
#19852 = ORIENTED_EDGE ( 'NONE', *, *, #35972, .F. ) ;
#19853 = CARTESIAN_POINT ( 'NONE',  ( 802.2119215644370342, -438.0090635724247932, -367.5423716828165084 ) ) ;
#19854 = CARTESIAN_POINT ( 'NONE',  ( 748.9653473494365699, -50.63460265842038410, -356.9462024416520762 ) ) ;
#19855 = CARTESIAN_POINT ( 'NONE',  ( 784.0799538623451781, -251.8055962898686744, 364.6971507214555572 ) ) ;
#19856 = CARTESIAN_POINT ( 'NONE',  ( 781.8018195045266339, -430.2709662947827383, -365.1927285166406705 ) ) ;
#19857 = CARTESIAN_POINT ( 'NONE',  ( 754.8072714833583632, -28.81642084023863504, -338.1981804954721156 ) ) ;
#19858 = CARTESIAN_POINT ( 'NONE',  ( 748.9653473494363425, -434.6346026584190554, 356.9462024416521331 ) ) ;
#19859 = DIRECTION ( 'NONE',  ( 0.000000000000000000, 0.7071067811865474617, 0.7071067811865474617 ) ) ;
#19860 = CARTESIAN_POINT ( 'NONE',  ( 775.8780910478218402, -297.2817908451526137, -364.9511171171680530 ) ) ;
#19861 = CARTESIAN_POINT ( 'NONE',  ( 748.9653473494363425, -170.6346026584199649, -356.9462024416521331 ) ) ;
#19862 = CARTESIAN_POINT ( 'NONE',  ( 808.3070685750230950, -66.99823902205672255, 361.1904061080339261 ) ) ;
#19863 = CARTESIAN_POINT ( 'NONE',  ( 751.6929314249748586, -150.9982390220563957, 318.8095938919659034 ) ) ;
#19864 = CARTESIAN_POINT ( 'NONE',  ( 794.1255485493337574, 16.45630643248849978, -314.6638991903497526 ) ) ;
#19865 = DIRECTION ( 'NONE',  ( -0.000000000000000000, 1.000000000000000000, -0.000000000000000000 ) ) ;
#19866 = EDGE_CURVE ( 'NONE', #7749, #20164, #28320, .T. ) ;
#19867 = CARTESIAN_POINT ( 'NONE',  ( 788.7631598425961101, -241.4419599262322720, -305.7194118038759143 ) ) ;
#19868 = CIRCLE ( 'NONE', #35326, 2.749999999999919176 ) ;
#19869 = CARTESIAN_POINT ( 'NONE',  ( 807.2620300519052989, -408.0090635724249069, 318.0141637701419768 ) ) ;
#19870 = ADVANCED_FACE ( 'NONE', ( #17728 ), #391, .F. ) ;
#19871 = DIRECTION ( 'NONE',  ( -1.000000000000000000, 0.000000000000000000, 0.000000000000000000 ) ) ;
#19872 = CARTESIAN_POINT ( 'NONE',  ( 772.4837098697144029, -407.3618753856920307, 374.5518280994205611 ) ) ;
#19873 = CARTESIAN_POINT ( 'NONE',  ( 751.9810565676468741, -2.089148112965993231, 360.9747183278973921 ) ) ;
#19874 = CARTESIAN_POINT ( 'NONE',  ( 774.6858677611749044, -369.7255117493284615, -315.5713283507209894 ) ) ;
#19875 = CARTESIAN_POINT ( 'NONE',  ( 803.8651313633788504, -29.26014174441482751, 332.4468031744301015 ) ) ;
#19876 = ADVANCED_FACE ( 'NONE', ( #28573 ), #7555, .T. ) ;
#19877 = CARTESIAN_POINT ( 'NONE',  ( 781.2370466360911223, -116.7363362996985217, -304.9990715423533629 ) ) ;
#19878 = CARTESIAN_POINT ( 'NONE',  ( 755.0488828828309806, -137.8055962898690154, -344.1219089521771934 ) ) ;
#19879 = CARTESIAN_POINT ( 'NONE',  ( 807.5423716828161105, -177.0783235625961538, 362.2119215644372048 ) ) ;
#19880 = CARTESIAN_POINT ( 'NONE',  ( 771.1735550268780344, 14.81994279612486309, 316.3353852180828198 ) ) ;
#19881 = CARTESIAN_POINT ( 'NONE',  ( 788.7366044899766848, -59.90732993114762905, -316.5762568750059813 ) ) ;
#19882 = CARTESIAN_POINT ( 'NONE',  ( 804.1601925771018387, -151.4419599262326415, -346.5483106153029098 ) ) ;
#19883 = CARTESIAN_POINT ( 'NONE',  ( 778.1981804954714335, -178.2709662947835625, 314.8072714833589885 ) ) ;
#19884 = CARTESIAN_POINT ( 'NONE',  ( 788.7631598425961101, -1.441959926233096656, -305.7194118038759143 ) ) ;
#19885 = APPLICATION_CONTEXT ( 'automotive_design' ) ;
#19886 = CARTESIAN_POINT ( 'NONE',  ( 781.7834795799800531, -298.8164208402377540, 315.0636971347436202 ) ) ;
#19887 = CARTESIAN_POINT ( 'NONE',  ( 521.6730038022808458, 199.9999999999999147, -122.7905160835442615 ) ) ;
#19888 = ORIENTED_EDGE ( 'NONE', *, *, #34286, .F. ) ;
#19889 = CARTESIAN_POINT ( 'NONE',  ( 795.9930595647434757, -3.078323562596726681, 320.7433823573372820 ) ) ;
#19890 = CARTESIAN_POINT ( 'NONE',  ( 811.3240766477731540, -268.3726999360616787, -355.6651683502462902 ) ) ;
#19891 = EDGE_CURVE ( 'NONE', #3536, #30163, #16560, .T. ) ;
#19892 = ORIENTED_EDGE ( 'NONE', *, *, #43308, .T. ) ;
#19893 = APPLICATION_PROTOCOL_DEFINITION ( 'draft international standard', 'automotive_design', 1998, #34917 ) ;
#19894 = CARTESIAN_POINT ( 'NONE',  ( 782.4968714119720516, -226.8164208402380098, 305.0891759886411023 ) ) ;
#19895 = ADVANCED_FACE ( 'NONE', ( #7333 ), #38742, .F. ) ;
#19896 = CARTESIAN_POINT ( 'NONE',  ( 790.9844846989617508, -310.3726999360616219, 317.2208543904092721 ) ) ;
#19897 = CARTESIAN_POINT ( 'NONE',  ( 802.7791456095903868, -388.7146871989592114, 329.0155153010375102 ) ) ;
#19898 = ORIENTED_EDGE ( 'NONE', *, *, #8622, .F. ) ;
#19899 = CARTESIAN_POINT ( 'NONE',  ( 775.8780910478218402, -129.2817908451530400, -364.9511171171680530 ) ) ;
#19900 = CARTESIAN_POINT ( 'NONE',  ( 788.8264449731200330, -117.1800572038746964, -363.6646147819171233 ) ) ;
#19901 = CARTESIAN_POINT ( 'NONE',  ( 804.9363028652555840, -328.2709662947831362, -338.2165204200192079 ) ) ;
#19902 = ORIENTED_EDGE ( 'NONE', *, *, #34603, .T. ) ;
#19903 = CARTESIAN_POINT ( 'NONE',  ( 757.8323909638827445, -434.6346026584190554, -352.1044303154654358 ) ) ;
#19904 = CARTESIAN_POINT ( 'NONE',  ( 796.7845633553578182, -297.6237781080502600, 358.5707757039688204 ) ) ;
#19905 = CARTESIAN_POINT ( 'NONE',  ( 928.0249999999991815, 154.9999999999998863, -360.0000000000000000 ) ) ;
#19906 = CARTESIAN_POINT ( 'NONE',  ( -26.63011601220122060, -110.5936016518799221, 750.6326042729449455 ) ) ;
#19907 = EDGE_CURVE ( 'NONE', #17994, #10694, #14940, .T. ) ;
#19908 = CARTESIAN_POINT ( 'NONE',  ( 771.1735550268778070, 14.81994279612486309, 316.3353852180827630 ) ) ;
#19909 = ORIENTED_EDGE ( 'NONE', *, *, #28592, .T. ) ;
#19910 = CARTESIAN_POINT ( 'NONE',  ( 781.2370466360911223, -356.7363362996978253, -304.9990715423533629 ) ) ;
#19911 = CARTESIAN_POINT ( 'NONE',  ( 814.8207195650702488, -194.1908817542437475, 336.2433038121456548 ) ) ;
#19912 = CARTESIAN_POINT ( 'NONE',  ( 797.6776695296629214, -307.5436935675104451, -357.6776695296636603 ) ) ;
#19913 =( NAMED_UNIT ( * ) PLANE_ANGLE_UNIT ( ) SI_UNIT ( $, .RADIAN. ) );
#19914 = CARTESIAN_POINT ( 'NONE',  ( 772.4468031744293057, -201.8272453906073451, -363.8651313633793620 ) ) ;
#19915 = CARTESIAN_POINT ( 'NONE',  ( 782.4968714119720516, -34.81642084023861372, 305.0891759886411023 ) ) ;
#19916 = LINE ( 'NONE', #27079, #4161 ) ;
#19917 = CARTESIAN_POINT ( 'NONE',  ( 808.0189434323515343, -374.0891481129647786, -319.0252816721025511 ) ) ;
#19918 = CARTESIAN_POINT ( 'NONE',  ( 799.9999999999993179, -512.9681489794448908, -350.0000000000000000 ) ) ;
#19919 = CARTESIAN_POINT ( 'NONE',  ( 803.4237431249931660, -63.18005720387488822, 331.2633955100225194 ) ) ;
#19920 = CARTESIAN_POINT ( 'NONE',  ( 799.9636004259356241, -310.9181544815160123, 311.2241431872006956 ) ) ;
#19921 = EDGE_CURVE ( 'NONE', #7984, #30278, #35714, .T. ) ;
#19922 = CARTESIAN_POINT ( 'NONE',  ( 999.9999999999992042, -599.5857864376268935, -359.5857864376268935 ) ) ;
#19923 = CARTESIAN_POINT ( 'NONE',  ( 814.9108240113580450, -280.2709662947833067, 337.5031285880265273 ) ) ;
#19924 = CARTESIAN_POINT ( 'NONE',  ( 745.4481719005789273, -27.72551174932954510, -347.5162901302853129 ) ) ;
#19925 = CARTESIAN_POINT ( 'NONE',  ( 785.3687786644884454, -251.3618753856923149, -315.3201227861279676 ) ) ;
#19926 = DIRECTION ( 'NONE',  ( 0.000000000000000000, 0.000000000000000000, 1.000000000000000000 ) ) ;
#19927 = CARTESIAN_POINT ( 'NONE',  ( 804.9363028652555840, -376.2709662947829656, 338.2165204200192079 ) ) ;
#19928 = CARTESIAN_POINT ( 'NONE',  ( 804.4086373105744769, -121.6454272087894282, 333.3843516231986541 ) ) ;
#19929 = CARTESIAN_POINT ( 'NONE',  ( 787.6308680596127942, -59.26014174441473870, -364.1105419155492768 ) ) ;
#19930 = CARTESIAN_POINT ( 'NONE',  ( 747.3154664389472828, -43.98741447168752217, 326.4474001241230781 ) ) ;
#19931 = CARTESIAN_POINT ( 'NONE',  ( 762.3223304703356007, -367.5436935675102745, 322.3223304703362828 ) ) ;
#19932 = CARTESIAN_POINT ( 'NONE',  ( 794.9999999999993179, -365.3551492539851893, 28.13243251470704109 ) ) ;
#19933 = CARTESIAN_POINT ( 'NONE',  ( 989.9999999999992042, 50.81038600091411439, -210.0000000000000000 ) ) ;
#19934 = CARTESIAN_POINT ( 'NONE',  ( 788.7631598425961101, -145.4419599262326699, 305.7194118038759143 ) ) ;
#19935 = CARTESIAN_POINT ( 'NONE',  ( 778.1981804954714335, -442.2709662947826814, 314.8072714833589885 ) ) ;
#19936 = VERTEX_POINT ( 'NONE', #32265 ) ;
#19937 = CARTESIAN_POINT ( 'NONE',  ( 804.9511171171677688, -365.8055962898682765, -335.8780910478229202 ) ) ;
#19939 = CARTESIAN_POINT ( 'NONE',  ( 788.8264449731201466, -189.1800572038744690, 363.6646147819170665 ) ) ;
#19938 = CARTESIAN_POINT ( 'NONE',  ( 767.8955696845333705, -192.4527844766016926, 362.1676090361162323 ) ) ;
#19940 = CARTESIAN_POINT ( 'NONE',  ( 773.7943932421234194, -359.8055962898683333, -305.5313806188329409 ) ) ;
#19941 = DIRECTION ( 'NONE',  ( -0.000000000000000000, -0.000000000000000000, 1.000000000000000000 ) ) ;
#19942 = ORIENTED_EDGE ( 'NONE', *, *, #31883, .T. ) ;
#19943 = CARTESIAN_POINT ( 'NONE',  ( 788.7366044899766848, -395.9073299311465348, 316.5762568750059813 ) ) ;
#19944 = EDGE_CURVE ( 'NONE', #6307, #9644, #22079, .T. ) ;
#19945 = ORIENTED_EDGE ( 'NONE', *, *, #35429, .F. ) ;
#19946 = CARTESIAN_POINT ( 'NONE',  ( 815.2698199232961542, -208.8164208402380666, -342.5225473063383106 ) ) ;
#19947 = CARTESIAN_POINT ( 'NONE',  ( 808.0189434323515343, -134.0891481129655745, 319.0252816721025511 ) ) ;
#19948 = EDGE_CURVE ( 'NONE', #35726, #14468, #24643, .T. ) ;
#19949 = ORIENTED_EDGE ( 'NONE', *, *, #43665, .T. ) ;
#19950 = CARTESIAN_POINT ( 'NONE',  ( 803.4237431249931660, -207.1800572038744406, -331.2633955100225194 ) ) ;
#19951 = ORIENTED_EDGE ( 'NONE', *, *, #20048, .F. ) ;
#19952 = CARTESIAN_POINT ( 'NONE',  ( 785.3687786644884454, -323.3618753856923149, -315.3201227861279676 ) ) ;
#19953 = CARTESIAN_POINT ( 'NONE',  ( 797.8594530101008786, 10.45630643248850866, -322.1405469898980982 ) ) ;
#19954 = CARTESIAN_POINT ( 'NONE',  ( 808.0189434323515343, -254.0891481129652334, 319.0252816721025511 ) ) ;
#19955 = CARTESIAN_POINT ( 'NONE',  ( 805.1016975059191054, -198.8965053807779384, 343.0745993439771837 ) ) ;
#19956 = EDGE_CURVE ( 'NONE', #26579, #30556, #28799, .T. ) ;
#19958 = DIRECTION ( 'NONE',  ( 1.000000000000000000, 0.000000000000000000, 0.000000000000000000 ) ) ;
#19957 = DIRECTION ( 'NONE',  ( -1.000000000000000000, -0.000000000000000000, -0.000000000000000000 ) ) ;
#19959 = FACE_BOUND ( 'NONE', #22056, .T. ) ;
#19960 = VERTEX_POINT ( 'NONE', #21865 ) ;
#19961 = CARTESIAN_POINT ( 'NONE',  ( 785.3687786644884454, 12.63812461430668321, -315.3201227861279676 ) ) ;
#19962 = CARTESIAN_POINT ( 'NONE',  ( 786.4999999999993179, -512.9681489794448908, -352.0000000000000000 ) ) ;
#19963 = LINE ( 'NONE', #43746, #24809 ) ;
#19964 = ORIENTED_EDGE ( 'NONE', *, *, #19370, .T. ) ;
#19965 = CARTESIAN_POINT ( 'NONE',  ( 746.4236121716829757, -231.8272453906072315, -328.8385539511384650 ) ) ;
#19966 = CARTESIAN_POINT ( 'NONE',  ( 762.1177392798416577, -114.5545181178803631, 309.8865473780659272 ) ) ;
#19968 = CARTESIAN_POINT ( 'NONE',  ( 755.5713283507202505, -197.3618753856926560, -334.6858677611754729 ) ) ;
#19967 = LINE ( 'NONE', #16499, #33725 ) ;
#19969 = CARTESIAN_POINT ( 'NONE',  ( 793.2243759319678702, -362.5328690171410813, -318.4439275373583200 ) ) ;
#19970 = CARTESIAN_POINT ( 'NONE',  ( 804.1009440267234822, -215.4636090269709712, -314.0944755984392600 ) ) ;
#19971 = FACE_OUTER_BOUND ( 'NONE', #33893, .T. ) ;
#19972 = CARTESIAN_POINT ( 'NONE',  ( 775.8780910478218402, -81.28179084515319630, -364.9511171171680530 ) ) ;
#19973 = CARTESIAN_POINT ( 'NONE',  ( 802.9823548866075953, -433.0999726633339151, 330.0799878456151077 ) ) ;
#19974 = FACE_OUTER_BOUND ( 'NONE', #1533, .T. ) ;
#19975 = CARTESIAN_POINT ( 'NONE',  ( 756.1348686366196716, -425.2601417444136018, -347.5531968255698416 ) ) ;
#19976 = CARTESIAN_POINT ( 'NONE',  ( 808.0189434323515343, -278.0891481129651197, -319.0252816721025511 ) ) ;
#19977 = PLANE ( 'NONE',  #25459 ) ;
#19978 = DIRECTION ( 'NONE',  ( 0.000000000000000000, -1.000000000000000000, 0.000000000000000000 ) ) ;
#19979 = CARTESIAN_POINT ( 'NONE',  ( 781.7834795799800531, -34.81642084023861372, -315.0636971347436202 ) ) ;
#19980 = CARTESIAN_POINT ( 'NONE',  ( 793.5525998758768083, -199.0999726633346825, 372.6845335610516941 ) ) ;
#19981 = CARTESIAN_POINT ( 'NONE',  ( 810.1134526219336749, -152.5328690171416781, -357.8822607201570349 ) ) ;
#19982 = CARTESIAN_POINT ( 'NONE',  ( 758.8095938919642549, -200.0891481129653187, 311.6929314249763365 ) ) ;
#19983 = CARTESIAN_POINT ( 'NONE',  ( 745.7998596910086917, -413.3618753856920307, -332.5602148656461168 ) ) ;
#19984 = DIRECTION ( 'NONE',  ( -0.000000000000000000, -0.000000000000000000, 1.000000000000000000 ) ) ;
#19985 = CARTESIAN_POINT ( 'NONE',  ( 800.0135310231082713, -254.0891481129652334, 325.0180583372163028 ) ) ;
#19986 = CARTESIAN_POINT ( 'NONE',  ( 763.0428371773158460, -59.46360902697142592, 358.7617431975195359 ) ) ;
#19987 = CARTESIAN_POINT ( 'NONE',  ( 785.3687786644884454, -443.3618753856917465, -315.3201227861279676 ) ) ;
#19988 = DIRECTION ( 'NONE',  ( -0.000000000000000000, -0.000000000000000000, 1.000000000000000000 ) ) ;
#19989 = DIRECTION ( 'NONE',  ( 0.000000000000000000, 0.000000000000000000, 1.000000000000000000 ) ) ;
#19990 = CARTESIAN_POINT ( 'NONE',  ( 769.1273215169530886, -94.71468719896007826, 317.4527132478988847 ) ) ;
#19991 = ORIENTED_EDGE ( 'NONE', *, *, #31205, .F. ) ;
#19992 = CARTESIAN_POINT ( 'NONE',  ( 765.8855110935204493, -238.1692326535050768, -319.0159684113471599 ) ) ;
#19993 = CARTESIAN_POINT ( 'NONE',  ( 759.9864689768902508, -50.08914811296584446, 354.9819416627836404 ) ) ;
#19994 = CARTESIAN_POINT ( 'NONE',  ( 744.8212110874229666, -258.8965053807777963, -336.2046728542121627 ) ) ;
#19995 = CARTESIAN_POINT ( 'NONE',  ( 998.9999999999992042, 74.99999999999984368, 360.0000000000000000 ) ) ;
#19996 = CARTESIAN_POINT ( 'NONE',  ( 812.6845335610512393, -367.9874144716865203, 353.5525998758768651 ) ) ;
#19997 = EDGE_LOOP ( 'NONE', ( #37496, #28185, #40735, #21770 ) ) ;
#19998 = CARTESIAN_POINT ( 'NONE',  ( 755.2512626584698410, 16.45630643248849267, 315.2512626584710915 ) ) ;
#19999 = CARTESIAN_POINT ( 'NONE',  ( 781.8018195045266339, -190.2709662947835909, -365.1927285166406705 ) ) ;
#20000 = CARTESIAN_POINT ( 'NONE',  ( 767.8955696845333705, -384.4527844766011526, 362.1676090361162323 ) ) ;
#20001 = CARTESIAN_POINT ( 'NONE',  ( 748.9653473494363425, -122.6346026584201354, -356.9462024416521331 ) ) ;
#20002 = CARTESIAN_POINT ( 'NONE',  ( 802.1676090361155502, -62.63460265842032726, -327.8955696845344505 ) ) ;
#20003 = ORIENTED_EDGE ( 'NONE', *, *, #23281, .F. ) ;
#20004 = CARTESIAN_POINT ( 'NONE',  ( 804.1105419155481968, -51.82724539060782121, -347.6308680596136469 ) ) ;
#20005 = VERTEX_POINT ( 'NONE', #14495 ) ;
#20006 = CARTESIAN_POINT ( 'NONE',  ( 773.4516893846965786, -355.6454272087887603, -315.8398074228977066 ) ) ;
#20008 = CARTESIAN_POINT ( 'NONE',  ( 779.4763451958990572, -416.7363362996975980, 365.0264073115438919 ) ) ;
#20007 = CARTESIAN_POINT ( 'NONE',  ( 778.1981804954714335, -82.27096629478388934, 314.8072714833589885 ) ) ;
#20011 = CARTESIAN_POINT ( 'NONE',  ( 761.9338519418445230, -350.5328690171411381, 370.4231160770881957 ) ) ;
#20010 = LINE ( 'NONE', #41036, #34330 ) ;
#20009 = CARTESIAN_POINT ( 'NONE',  ( 814.9108240113580450, -424.2709662947829088, 337.5031285880265273 ) ) ;
#20012 = CARTESIAN_POINT ( 'NONE',  ( 779.4763451958990572, -320.7363362996979390, -365.0264073115438919 ) ) ;
#20013 = CARTESIAN_POINT ( 'NONE',  ( 800.2193346964447755, -330.9982390220558273, -355.1360043628815788 ) ) ;
#20014 = CARTESIAN_POINT ( 'NONE',  ( 815.3608509340175488, -122.7363362996985074, -341.2497674668889545 ) ) ;
#20015 = CARTESIAN_POINT ( 'NONE',  ( 814.2805881961230625, -1.645427208789804308, 331.2368401574024119 ) ) ;
#20017 = CARTESIAN_POINT ( 'NONE',  ( 784.4999999999993179, -544.8427095258973623, -369.9999999999999432 ) ) ;
#20016 = CARTESIAN_POINT ( 'NONE',  ( 781.3877698825695006, 18.31902617013176027, 309.9999999999999432 ) ) ;
#20018 = CARTESIAN_POINT ( 'NONE',  ( 802.7791456095903868, -268.7146871989595525, -329.0155153010375102 ) ) ;
#20019 = CARTESIAN_POINT ( 'NONE',  ( 797.8822607201568644, -102.5545181178804057, -370.1134526219340160 ) ) ;
#20020 = FACE_OUTER_BOUND ( 'NONE', #45347, .T. ) ;
#20021 = DIRECTION ( 'NONE',  ( 0.000000000000000000, 0.000000000000000000, 1.000000000000000000 ) ) ;
#20022 = CARTESIAN_POINT ( 'NONE',  ( 804.6971507214547046, -339.2817908451524431, 344.0799538623459739 ) ) ;
#20023 = ORIENTED_EDGE ( 'NONE', *, *, #14855, .T. ) ;
#20024 = CARTESIAN_POINT ( 'NONE',  ( 748.6759233522253680, -304.3726999360615082, 324.3348316497537098 ) ) ;
#20025 = CARTESIAN_POINT ( 'NONE',  ( 759.0252816721024374, -168.9982390220563673, -368.0189434323527280 ) ) ;
#20026 = DIRECTION ( 'NONE',  ( 0.000000000000000000, 0.000000000000000000, 1.000000000000000000 ) ) ;
#20027 = CARTESIAN_POINT ( 'NONE',  ( 762.1177392798416577, -114.5545181178803631, 309.8865473780659272 ) ) ;
#20028 = CARTESIAN_POINT ( 'NONE',  ( 804.7487373415286811, -307.5436935675104451, -364.7487373415288516 ) ) ;
#20029 = CARTESIAN_POINT ( 'NONE',  ( -919.9999999999993179, 219.9999999999998863, -360.0000000000000000 ) ) ;
#20030 = CARTESIAN_POINT ( 'NONE',  ( 804.4286716492782716, -161.3618753856927697, 345.3141322388244703 ) ) ;
#20031 = CIRCLE ( 'NONE', #28912, 10.00000000000000888 ) ;
#20032 = ORIENTED_EDGE ( 'NONE', *, *, #17246, .F. ) ;
#20033 = CARTESIAN_POINT ( 'NONE',  ( 788.6739635108323228, -415.6454272087885897, 373.9316612368139090 ) ) ;
#20034 = CARTESIAN_POINT ( 'NONE',  ( 749.8865473780648472, -356.5328690171410813, -322.1177392798429082 ) ) ;
#20035 = CARTESIAN_POINT ( 'NONE',  ( 810.7187646348534145, -114.4527844766020053, -356.7737145352016341 ) ) ;
#20036 = CARTESIAN_POINT ( 'NONE',  ( 804.6971507214547046, -51.28179084515328867, 344.0799538623459739 ) ) ;
#20037 = CARTESIAN_POINT ( 'NONE',  ( 782.4968714119720516, -394.8164208402374697, -305.0891759886411023 ) ) ;
#20038 = DIRECTION ( 'NONE',  ( 0.000000000000000000, 0.000000000000000000, 1.000000000000000000 ) ) ;
#20039 = CARTESIAN_POINT ( 'NONE',  ( 773.7943932421234194, 24.19440371013046231, 305.5313806188329409 ) ) ;
#20040 = ORIENTED_EDGE ( 'NONE', *, *, #42114, .T. ) ;
#20041 = CARTESIAN_POINT ( 'NONE',  ( 805.9055244015594326, -171.6237781080507432, -315.8990559732753240 ) ) ;
#20042 = FACE_OUTER_BOUND ( 'NONE', #18716, .T. ) ;
#20043 = CARTESIAN_POINT ( 'NONE',  ( 759.8311093483677041, -286.1692326535048778, 310.9282345327691814 ) ) ;
#20044 = CARTESIAN_POINT ( 'NONE',  ( 803.4237431249931660, -87.18005720387481006, 331.2633955100225194 ) ) ;
#20045 = EDGE_LOOP ( 'NONE', ( #10689, #23395, #7459, #36124 ) ) ;
#20046 = CARTESIAN_POINT ( 'NONE',  ( 755.3201227861273992, -267.7255117493286320, 345.3687786644892981 ) ) ;
#20047 = CARTESIAN_POINT ( 'NONE',  ( 763.2262854647970016, -8.634602658420517329, -309.2812353651462445 ) ) ;
#20048 = EDGE_CURVE ( 'NONE', #17925, #16350, #35954, .T. ) ;
#20049 = CARTESIAN_POINT ( 'NONE',  ( 793.1929000023510525, -451.7523979515906944, 372.2801657505705180 ) ) ;
#20050 = EDGE_LOOP ( 'NONE', ( #1322, #10647, #21639, #10936 ) ) ;
#20051 = ORIENTED_EDGE ( 'NONE', *, *, #37699, .T. ) ;
#20052 = CARTESIAN_POINT ( 'NONE',  ( 795.8262568251477660, -406.3726999360612808, -308.3538107759623585 ) ) ;
#20054 = CARTESIAN_POINT ( 'NONE',  ( 798.0661480581538854, -242.5328690171414507, 309.5768839229118043 ) ) ;
#20053 = CARTESIAN_POINT ( 'NONE',  ( 759.0252816721024374, -312.9982390220559409, 368.0189434323527280 ) ) ;
#20055 = CARTESIAN_POINT ( 'NONE',  ( 772.4468031744293057, -225.8272453906072599, -363.8651313633793620 ) ) ;
#20056 = CARTESIAN_POINT ( 'NONE',  ( 754.8072714833581358, -220.8164208402379529, -338.1981804954720587 ) ) ;
#20057 = CIRCLE ( 'NONE', #32646, 10.00000000000000888 ) ;
#20058 = CARTESIAN_POINT ( 'NONE',  ( 774.6312213355098493, -431.3618753856918602, -364.6798772138717482 ) ) ;
#20059 = CARTESIAN_POINT ( 'NONE',  ( 778.1981804954714335, -202.2709662947834772, 314.8072714833589885 ) ) ;
#20060 = CARTESIAN_POINT ( 'NONE',  ( 804.6798772138708955, -111.7255117493293000, -334.6312213355107019 ) ) ;
#20061 = ORIENTED_EDGE ( 'NONE', *, *, #22184, .F. ) ;
#20062 = CARTESIAN_POINT ( 'NONE',  ( 751.6929314249748586, -366.9982390220556567, 318.8095938919659034 ) ) ;
#20063 = DIRECTION ( 'NONE',  ( 0.000000000000000000, -1.000000000000000000, -1.672022627447525240E-16 ) ) ;
#20064 = CARTESIAN_POINT ( 'NONE',  ( 815.3608509340175488, -2.736336299698892027, -341.2497674668889545 ) ) ;
#20065 = CARTESIAN_POINT ( 'NONE',  ( 795.1616405723528942, 16.45630643248848912, 314.3282859078202591 ) ) ;
#20066 = CARTESIAN_POINT ( 'NONE',  ( 794.9999999999993179, -365.3551492539851893, -1.867567485292990437 ) ) ;
#20067 = CARTESIAN_POINT ( 'NONE',  ( 787.5531968255692163, -237.8272453906072599, 316.1348686366205811 ) ) ;
#20068 = CARTESIAN_POINT ( 'NONE',  ( 755.3201227861273992, -99.72551174932928575, 345.3687786644892981 ) ) ;
#20069 = EDGE_CURVE ( 'NONE', #39647, #2064, #161, .T. ) ;
#20070 = ORIENTED_EDGE ( 'NONE', *, *, #11760, .F. ) ;
#20071 = CARTESIAN_POINT ( 'NONE',  ( 781.2370466360911223, -452.7363362996975411, -304.9990715423533629 ) ) ;
#20072 = CARTESIAN_POINT ( 'NONE',  ( 758.8095938919644823, -56.08914811296581604, -311.6929314249762797 ) ) ;
#20073 = CARTESIAN_POINT ( 'NONE',  ( 801.3366627262608972, -248.5328690171414223, 353.0897708529566899 ) ) ;
#20074 = CARTESIAN_POINT ( 'NONE',  ( 794.9819416627830151, -420.9982390220555999, -319.9864689768909898 ) ) ;
#20075 = CARTESIAN_POINT ( 'NONE',  ( 794.9819416627830151, -36.99823902205679360, -319.9864689768909898 ) ) ;
#20076 = CARTESIAN_POINT ( 'NONE',  ( 754.3581564841646241, -17.46360902697157513, 316.1443688327762516 ) ) ;
#20077 = LINE ( 'NONE', #35478, #14413 ) ;
#20078 = CARTESIAN_POINT ( 'NONE',  ( 802.9823548866075953, -289.0999726633343698, -330.0799878456151077 ) ) ;
#20079 = CARTESIAN_POINT ( 'NONE',  ( 814.5518280994195948, -207.7255117493289447, -332.4837098697145734 ) ) ;
#20080 = CARTESIAN_POINT ( 'NONE',  ( 749.2812353651451076, -78.45278447660211896, 323.2262854647983090 ) ) ;
#20081 = CARTESIAN_POINT ( 'NONE',  ( 814.5518280994195948, -159.7255117493291436, 332.4837098697145734 ) ) ;
#20082 = AXIS2_PLACEMENT_3D ( 'NONE', #42017, #38785, #10593 ) ;
#20083 = LINE ( 'NONE', #27254, #21008 ) ;
#20084 = CARTESIAN_POINT ( 'NONE',  ( -200.7583438952258916, 294.6698570112193920, -274.9999999999999432 ) ) ;
#20085 = CARTESIAN_POINT ( 'NONE',  ( 815.1787889125755555, -222.8965053807778531, -343.7953271457877804 ) ) ;
#20086 = CARTESIAN_POINT ( 'NONE',  ( 797.8822607201568644, -414.5545181178795247, 370.1134526219340160 ) ) ;
#20087 = CARTESIAN_POINT ( 'NONE',  ( 745.4481719005789273, -267.7255117493286320, -347.5162901302853129 ) ) ;
#20088 = DIRECTION ( 'NONE',  ( 0.000000000000000000, 0.000000000000000000, 1.000000000000000000 ) ) ;
#20089 = CARTESIAN_POINT ( 'NONE',  ( 814.9108240113580450, -400.2709662947828519, 337.5031285880265273 ) ) ;
#20090 = CARTESIAN_POINT ( 'NONE',  ( 787.4397851343537695, 2.274488250670355871, 374.2001403089903988 ) ) ;
#20091 = CARTESIAN_POINT ( 'NONE',  ( 794.9819416627830151, -348.9982390220558273, -319.9864689768909898 ) ) ;
#20092 = CARTESIAN_POINT ( 'NONE',  ( 761.2382568024794409, -15.62377810805123524, 356.9571628226838129 ) ) ;
#20093 = CARTESIAN_POINT ( 'NONE',  ( 756.1443688327750579, -45.62377810805114109, -314.3581564841659315 ) ) ;
#20094 = CARTESIAN_POINT ( 'NONE',  ( 799.4546378042377910, -153.0783235625962675, -356.1575198192848006 ) ) ;
#20095 = CARTESIAN_POINT ( 'NONE',  ( 793.4146539503750546, -169.9874144716871172, 307.6481478633938877 ) ) ;
#20096 = DIRECTION ( 'NONE',  ( 0.000000000000000000, 0.000000000000000000, 1.000000000000000000 ) ) ;
#20097 = CARTESIAN_POINT ( 'NONE',  ( 795.6651683502461765, -178.7146871989598083, 371.3240766477733814 ) ) ;
#20098 = EDGE_LOOP ( 'NONE', ( #45171, #13951, #39803, #25945 ) ) ;
#20099 = CARTESIAN_POINT ( 'NONE',  ( 754.8072714833581358, -52.81642084023856398, -338.1981804954720587 ) ) ;
#20100 = CARTESIAN_POINT ( 'NONE',  ( 773.3843516231979720, -157.4419599262326130, -364.4086373105754433 ) ) ;
#20101 = CARTESIAN_POINT ( 'NONE',  ( 805.1927285166397041, -160.8164208402382371, 341.8018195045277707 ) ) ;
#20102 = EDGE_CURVE ( 'NONE', #40626, #42174, #22088, .T. ) ;
#20103 = CARTESIAN_POINT ( 'NONE',  ( 766.5853460496234675, -13.98741447168760033, -372.3518521366060554 ) ) ;
#20104 = CARTESIAN_POINT ( 'NONE',  ( 764.8639956371174549, -296.0891481129650629, 319.7806653035542581 ) ) ;
#20105 = DIRECTION ( 'NONE',  ( 0.000000000000000000, 0.000000000000000000, 1.000000000000000000 ) ) ;
#20106 = VERTEX_POINT ( 'NONE', #841 ) ;
#20107 = CARTESIAN_POINT ( 'NONE',  ( 775.9200461376533440, -23.80559628986938847, 315.3028492785443291 ) ) ;
#20108 = CARTESIAN_POINT ( 'NONE',  ( 804.1009440267234822, -287.4636090269708575, -314.0944755984392600 ) ) ;
#20109 = ORIENTED_EDGE ( 'NONE', *, *, #20182, .T. ) ;
#20110 = DIRECTION ( 'NONE',  ( 0.000000000000000000, 0.000000000000000000, 1.000000000000000000 ) ) ;
#20111 = EDGE_CURVE ( 'NONE', #21203, #4574, #12138, .T. ) ;
#20112 = CARTESIAN_POINT ( 'NONE',  ( 792.2312462859673587, -203.9073299311471885, 307.2067596250082602 ) ) ;
#20113 = CARTESIAN_POINT ( 'NONE',  ( 763.0428371773158460, -347.4636090269705733, 358.7617431975195359 ) ) ;
#20114 = CARTESIAN_POINT ( 'NONE',  ( 794.1144889064781864, -418.1692326535044799, 360.9840315886528401 ) ) ;
#20115 = ORIENTED_EDGE ( 'NONE', *, *, #30652, .T. ) ;
#20116 = CARTESIAN_POINT ( 'NONE',  ( 802.9823548866075953, -121.0999726633348956, -330.0799878456151077 ) ) ;
#20117 = CARTESIAN_POINT ( 'NONE',  ( 756.3353852180819104, -125.9073299311474159, -331.1735550268788302 ) ) ;
#20118 = CIRCLE ( 'NONE', #19394, 9.999999999999982236 ) ;
#20119 = CARTESIAN_POINT ( 'NONE',  ( 774.6858677611749044, -321.7255117493286320, -315.5713283507209894 ) ) ;
#20120 = ORIENTED_EDGE ( 'NONE', *, *, #28077, .T. ) ;
#20121 = CARTESIAN_POINT ( 'NONE',  ( 788.7366044899766848, -443.9073299311464780, -316.5762568750059813 ) ) ;
#20122 = CARTESIAN_POINT ( 'NONE',  ( 755.8398074228967971, -307.4419599262320730, 333.4516893846970333 ) ) ;
#20123 = FACE_OUTER_BOUND ( 'NONE', #22169, .T. ) ;
#20124 = CARTESIAN_POINT ( 'NONE',  ( 779.9999999999992042, 16.45630643248849267, -309.9999999999998863 ) ) ;
#20125 = CARTESIAN_POINT ( 'NONE',  ( 758.4439275373578084, -108.5545181178803915, 353.2243759319684386 ) ) ;
#20126 = CYLINDRICAL_SURFACE ( 'NONE', #5682, 6.118999999999985562 ) ;
#20127 = ORIENTED_EDGE ( 'NONE', *, *, #38295, .T. ) ;
#20128 = CARTESIAN_POINT ( 'NONE',  ( 745.7194118038753459, -349.6454272087887603, -348.7631598425976449 ) ) ;
#20129 = CARTESIAN_POINT ( 'NONE',  ( 795.8262568251477660, -190.3726999360619629, 308.3538107759623585 ) ) ;
#20130 = CARTESIAN_POINT ( 'NONE',  ( 765.0180583372156207, -312.9982390220559409, -360.0135310231089534 ) ) ;
#20131 = DIRECTION ( 'NONE',  ( 0.000000000000000000, 0.000000000000000000, 1.000000000000000000 ) ) ;
#20132 = CARTESIAN_POINT ( 'NONE',  ( 796.9571628226829034, -191.4636090269709996, -321.2382568024804641 ) ) ;
#20133 = CARTESIAN_POINT ( 'NONE',  ( 745.4481719005789273, -51.72551174932946338, 347.5162901302853129 ) ) ;
#20134 = CARTESIAN_POINT ( 'NONE',  ( 784.9999999999992042, 239.9999999999998863, -235.0000000000000000 ) ) ;
#20135 = CARTESIAN_POINT ( 'NONE',  ( 782.4968714119720516, -394.8164208402374697, -305.0891759886411023 ) ) ;
#20136 = PLANE ( 'NONE',  #14362 ) ;
#20137 = CARTESIAN_POINT ( 'NONE',  ( 755.8990559732751535, -323.4636090269706301, 365.9055244015606831 ) ) ;
#20138 = PLANE ( 'NONE',  #10987 ) ;
#20139 = CARTESIAN_POINT ( 'NONE',  ( 814.5518280994195948, -279.7255117493288026, 332.4837098697145734 ) ) ;
#20140 = CARTESIAN_POINT ( 'NONE',  ( 755.2512626584698410, -7.543693567511430942, -315.2512626584710915 ) ) ;
#20141 = CARTESIAN_POINT ( 'NONE',  ( 762.1405469898971887, -241.5436935675106156, -357.8594530101015607 ) ) ;
#20142 = EDGE_CURVE ( 'NONE', #39064, #21254, #45679, .T. ) ;
#20143 = DIRECTION ( 'NONE',  ( 0.000000000000000000, -0.3826834323650838976, -0.9238795325112892920 ) ) ;
#20144 = CARTESIAN_POINT ( 'NONE',  ( 762.1405469898971887, -385.5436935675102745, 357.8594530101015607 ) ) ;
#20145 = AXIS2_PLACEMENT_3D ( 'NONE', #3634, #6163, #20252 ) ;
#20146 = CARTESIAN_POINT ( 'NONE',  ( 804.4086373105744769, -169.6454272087892718, 333.3843516231986541 ) ) ;
#20147 = CARTESIAN_POINT ( 'NONE',  ( 764.0069404352550464, -39.07832356259662276, -359.2566176426627180 ) ) ;
#20148 = CARTESIAN_POINT ( 'NONE',  ( 801.9858362298568863, -75.07832356259649487, 312.7379699480935642 ) ) ;
#20149 = CARTESIAN_POINT ( 'NONE',  ( 781.8018195045267476, -358.2709662947830225, 365.1927285166407273 ) ) ;
#20150 = CARTESIAN_POINT ( 'NONE',  ( -190.7583438952258916, 294.6698570112193920, -274.9999999999999432 ) ) ;
#20151 = CARTESIAN_POINT ( 'NONE',  ( 794.9819416627830151, -420.9982390220555999, 319.9864689768909898 ) ) ;
#20152 = ORIENTED_EDGE ( 'NONE', *, *, #4945, .T. ) ;
#20153 = CARTESIAN_POINT ( 'NONE',  ( 762.1405469898971887, -49.54369356751129061, -357.8594530101015607 ) ) ;
#20154 = EDGE_CURVE ( 'NONE', #45239, #32411, #15111, .T. ) ;
#20155 = EDGE_CURVE ( 'NONE', #20268, #4067, #20989, .T. ) ;
#20156 = CARTESIAN_POINT ( 'NONE',  ( 773.3843516231979720, -349.4419599262320162, -364.4086373105754433 ) ) ;
#20158 = CARTESIAN_POINT ( 'NONE',  ( 791.9812246680005501, -188.6346026584199365, 361.9419747391813189 ) ) ;
#20157 = CARTESIAN_POINT ( 'NONE',  ( 755.3201227861273992, -195.7255117493289731, 345.3687786644892981 ) ) ;
#20159 = CARTESIAN_POINT ( 'NONE',  ( 761.9338519418445230, -374.5328690171410813, -370.4231160770881957 ) ) ;
#20160 = LINE ( 'NONE', #30796, #14624 ) ;
#20161 = VERTEX_POINT ( 'NONE', #33615 ) ;
#20162 = CARTESIAN_POINT ( 'NONE',  ( 801.9419747391806368, -378.4527844766011526, 351.9812246680014027 ) ) ;
#20163 = VECTOR ( 'NONE', #45403, 1000.000000000000000 ) ;
#20164 = VERTEX_POINT ( 'NONE', #4760 ) ;
#20165 = CARTESIAN_POINT ( 'NONE',  ( 763.2262854647970016, -224.6346026584198228, -309.2812353651462445 ) ) ;
#20166 = CARTESIAN_POINT ( 'NONE',  ( 748.9653473494365699, -122.6346026584201496, 356.9462024416520762 ) ) ;
#20167 = VERTEX_POINT ( 'NONE', #30148 ) ;
#20168 = CARTESIAN_POINT ( 'NONE',  ( 778.1981804954715471, -226.2709662947834488, -314.8072714833591021 ) ) ;
#20169 = ORIENTED_EDGE ( 'NONE', *, *, #3017, .F. ) ;
#20170 = ADVANCED_FACE ( 'NONE', ( #15173 ), #19295, .F. ) ;
#20171 = CARTESIAN_POINT ( 'NONE',  ( 804.1105419155481968, -459.8272453906066062, -347.6308680596136469 ) ) ;
#20172 = EDGE_CURVE ( 'NONE', #12019, #9099, #5207, .T. ) ;
#20173 = CARTESIAN_POINT ( 'NONE',  ( 755.2512626584698410, -271.5436935675106156, 315.2512626584710915 ) ) ;
#20174 = CARTESIAN_POINT ( 'NONE',  ( 776.9566956441375396, -204.8965053807779100, 364.8461984189686405 ) ) ;
#20176 = LINE ( 'NONE', #16952, #15235 ) ;
#20175 = DIRECTION ( 'NONE',  ( -0.000000000000000000, 1.000000000000000000, -0.000000000000000000 ) ) ;
#20177 = LINE ( 'NONE', #23853, #10307 ) ;
#20178 = VERTEX_POINT ( 'NONE', #40344 ) ;
#20179 = CARTESIAN_POINT ( 'NONE',  ( 804.9363028652555840, 7.729033705215793582, -338.2165204200192079 ) ) ;
#20180 = CYLINDRICAL_SURFACE ( 'NONE', #28428, 7.999999999999896083 ) ;
#20181 = DIRECTION ( 'NONE',  ( 1.000000000000000000, -4.147566128926363633E-16, 0.000000000000000000 ) ) ;
#20182 = EDGE_CURVE ( 'NONE', #12556, #38643, #45335, .T. ) ;
#20183 = ORIENTED_EDGE ( 'NONE', *, *, #23550, .F. ) ;
#20184 = CARTESIAN_POINT ( 'NONE',  ( 788.6739635108323228, -247.6454272087890160, -373.9316612368139090 ) ) ;
#20185 = CARTESIAN_POINT ( 'NONE',  ( 814.4686193811664907, -99.28179084515313946, 346.2056067578752732 ) ) ;
#20187 = CARTESIAN_POINT ( 'NONE',  ( 788.7366044899766848, -227.9073299311471033, -316.5762568750059813 ) ) ;
#20186 = DIRECTION ( 'NONE',  ( 0.000000000000000000, -0.3826834323650835645, -0.9238795325112892920 ) ) ;
#20188 = CARTESIAN_POINT ( 'NONE',  ( 764.0069404352550464, -351.0783235625955854, -359.2566176426627180 ) ) ;
#20189 = CARTESIAN_POINT ( 'NONE',  ( 749.5768839229115201, -252.5545181178799226, -358.0661480581553064 ) ) ;
#20190 = LINE ( 'NONE', #26444, #24472 ) ;
#20191 = LINE ( 'NONE', #1951, #2407 ) ;
#20192 = CARTESIAN_POINT ( 'NONE',  ( 800.9840315886518738, -76.91815448151683654, -354.1144889064786412 ) ) ;
#20193 = CARTESIAN_POINT ( 'NONE',  ( 755.8894580844503253, -447.8272453906067199, 332.3691319403863531 ) ) ;
#20194 = CARTESIAN_POINT ( 'NONE',  ( 805.6418435158337843, -365.4636090269705164, 363.8556311672236916 ) ) ;
#20195 = DIRECTION ( 'NONE',  ( 1.000000000000000000, 0.000000000000000000, 0.000000000000000000 ) ) ;
#20196 = CARTESIAN_POINT ( 'NONE',  ( 792.3570229623691148, -261.1800572038742416, -373.1304606946836770 ) ) ;
#20197 = CARTESIAN_POINT ( 'NONE',  ( 311.1634899080286232, 258.0939999999999941, -199.9999999999963336 ) ) ;
#20198 = DIRECTION ( 'NONE',  ( 0.000000000000000000, 1.000000000000000000, -0.000000000000000000 ) ) ;
#20199 = CARTESIAN_POINT ( 'NONE',  ( 797.8594530101008786, -37.54369356751132614, -322.1405469898980982 ) ) ;
#20200 = EDGE_CURVE ( 'NONE', #43685, #16782, #16556, .T. ) ;
#20201 = CARTESIAN_POINT ( 'NONE',  ( 797.8822607201568644, -198.5545181178800647, 370.1134526219340160 ) ) ;
#20202 = CARTESIAN_POINT ( 'NONE',  ( 807.5423716828161105, -177.0783235625961538, -362.2119215644372048 ) ) ;
#20203 = CARTESIAN_POINT ( 'NONE',  ( 751.6929314249748586, -174.9982390220563673, 318.8095938919659034 ) ) ;
#20204 = CARTESIAN_POINT ( 'NONE',  ( 767.6429770376289525, -417.1800572038736163, -306.8695393053162093 ) ) ;
#20205 = CARTESIAN_POINT ( 'NONE',  ( -786.4999999999993179, -544.8427095258973623, -369.9999999999999432 ) ) ;
#20206 = EDGE_CURVE ( 'NONE', #4574, #30680, #40770, .T. ) ;
#20207 = CARTESIAN_POINT ( 'NONE',  ( 755.5713283507202505, -293.3618753856923718, 334.6858677611754729 ) ) ;
#20208 = CARTESIAN_POINT ( 'NONE',  ( 790.9844846989617508, -70.37269993606230400, 317.2208543904092721 ) ) ;
#20209 = CARTESIAN_POINT ( 'NONE',  ( 756.3353852180819104, -437.9073299311463074, -331.1735550268788302 ) ) ;
#20210 = CARTESIAN_POINT ( 'NONE',  ( 115.7583438952258774, 290.0000000000001137, -320.0000000000000568 ) ) ;
#20211 = LINE ( 'NONE', #6805, #32840 ) ;
#20213 = CARTESIAN_POINT ( 'NONE',  ( 765.0180583372156207, -336.9982390220558273, 360.0135310231089534 ) ) ;
#20212 = CARTESIAN_POINT ( 'NONE',  ( 783.0433043558608688, -72.89650538077830788, 315.1538015810313027 ) ) ;
#20214 = EDGE_LOOP ( 'NONE', ( #15525, #21332, #22426, #1743 ) ) ;
#20215 = CARTESIAN_POINT ( 'NONE',  ( 803.8651313633788504, -269.2601417444139997, -332.4468031744301015 ) ) ;
#20216 = CARTESIAN_POINT ( 'NONE',  ( 800.2193346964447755, -42.99823902205675807, 355.1360043628815788 ) ) ;
#20217 = AXIS2_PLACEMENT_3D ( 'NONE', #28255, #17435, #45618 ) ;
#20218 = CARTESIAN_POINT ( 'NONE',  ( 808.7758568127978833, -268.1692326535049347, -320.0363995740631822 ) ) ;
#20219 = DIRECTION ( 'NONE',  ( 0.000000000000000000, 0.000000000000000000, 1.000000000000000000 ) ) ;
#20220 = CARTESIAN_POINT ( 'NONE',  ( 811.6461892240364477, -388.7146871989592114, 324.1737431748509835 ) ) ;
#20221 = ORIENTED_EDGE ( 'NONE', *, *, #20442, .F. ) ;
#20222 = CARTESIAN_POINT ( 'NONE',  ( 785.3687786644884454, -275.3618753856923149, 315.3201227861279676 ) ) ;
#20223 = CARTESIAN_POINT ( 'NONE',  ( 782.5225473063381969, 1.729033705215812011, 375.2698199232970637 ) ) ;
#20224 = CARTESIAN_POINT ( 'NONE',  ( 792.1044303154645831, -156.4527844766018916, -317.8323909638837677 ) ) ;
#20225 = CARTESIAN_POINT ( 'NONE',  ( 803.4237431249931660, -375.1800572038739574, 331.2633955100225194 ) ) ;
#20226 = CARTESIAN_POINT ( 'NONE',  ( 751.6929314249748586, -102.9982390220565520, -318.8095938919659034 ) ) ;
#20227 = CARTESIAN_POINT ( 'NONE',  ( 805.1927285166399315, -112.8164208402383650, -341.8018195045277707 ) ) ;
#20228 = ORIENTED_EDGE ( 'NONE', *, *, #11174, .F. ) ;
#20229 = CARTESIAN_POINT ( 'NONE',  ( 796.1575198192839480, -30.00906357242607925, -359.4546378042384163 ) ) ;
#20230 = CARTESIAN_POINT ( 'NONE',  ( 804.8461984189677878, -362.1908817542432644, -336.9566956441385628 ) ) ;
#20231 = VECTOR ( 'NONE', #35540, 1000.000000000000000 ) ;
#20233 = CARTESIAN_POINT ( 'NONE',  ( 800.9840315886518738, -388.9181544815158986, 354.1144889064786412 ) ) ;
#20232 = CARTESIAN_POINT ( 'NONE',  ( 785.3687786644884454, -107.3618753856928976, 315.3201227861279676 ) ) ;
#20236 = CARTESIAN_POINT ( 'NONE',  ( 798.0661480581538854, -362.5328690171410813, 309.5768839229118043 ) ) ;
#20235 = LINE ( 'NONE', #34323, #26225 ) ;
#20234 = CARTESIAN_POINT ( 'NONE',  ( 793.3938497862117174, -453.0432664090020580, 372.3358127763067955 ) ) ;
#20237 = AXIS2_PLACEMENT_3D ( 'NONE', #23435, #27590, #5666 ) ;
#20238 = CARTESIAN_POINT ( 'NONE',  ( 757.0176451133909268, -373.0999726633340856, -349.9200121543848354 ) ) ;
#20239 = CARTESIAN_POINT ( 'NONE',  ( 778.2165204200184689, -310.8164208402377540, -364.9363028652563230 ) ) ;
#20240 = CARTESIAN_POINT ( 'NONE',  ( 773.7305795820266212, -129.2817908451530400, -374.8230680027170365 ) ) ;
#20241 = CARTESIAN_POINT ( 'NONE',  ( 814.9108240113580450, -448.2709662947827951, 337.5031285880265273 ) ) ;
#20242 = FACE_OUTER_BOUND ( 'NONE', #41423, .T. ) ;
#20243 = CARTESIAN_POINT ( 'NONE',  ( 761.2382568024794409, -255.6237781080504874, -356.9571628226838129 ) ) ;
#20244 = CARTESIAN_POINT ( 'NONE',  ( 748.6759233522253680, -136.3726999360621051, -324.3348316497537098 ) ) ;
#20245 = FACE_OUTER_BOUND ( 'NONE', #29789, .T. ) ;
#20246 = FACE_OUTER_BOUND ( 'NONE', #3556, .T. ) ;
#20247 = CARTESIAN_POINT ( 'NONE',  ( 793.9708237608222134, -334.9181544815160692, 319.2295555964448681 ) ) ;
#20248 = ORIENTED_EDGE ( 'NONE', *, *, #33765, .F. ) ;
#20249 = CARTESIAN_POINT ( 'NONE',  ( 799.9636004259356241, -286.9181544815161828, 311.2241431872006956 ) ) ;
#20250 = VECTOR ( 'NONE', #5359, 1000.000000000000000 ) ;
#20251 = CARTESIAN_POINT ( 'NONE',  ( 810.7187646348534145, -186.4527844766017779, -356.7737145352016341 ) ) ;
#20252 = DIRECTION ( 'NONE',  ( 0.000000000000000000, 0.000000000000000000, 1.000000000000000000 ) ) ;
#20253 = AXIS2_PLACEMENT_3D ( 'NONE', #37003, #19451, #2345 ) ;
#20254 = CARTESIAN_POINT ( 'NONE',  ( 814.4686193811664907, -123.2817908451530542, 346.2056067578752732 ) ) ;
#20255 = CARTESIAN_POINT ( 'NONE',  ( 751.9810565676468741, -290.0891481129650629, -360.9747183278973921 ) ) ;
#20256 = CARTESIAN_POINT ( 'NONE',  ( -879.9999999999992042, 430.0000000000002842, -244.9999999999999716 ) ) ;
#20257 = DIRECTION ( 'NONE',  ( -0.000000000000000000, -0.000000000000000000, 1.000000000000000000 ) ) ;
#20258 = CARTESIAN_POINT ( 'NONE',  ( 757.8323909638827445, -146.6346026584200217, 352.1044303154654358 ) ) ;
#20259 = ORIENTED_EDGE ( 'NONE', *, *, #17939, .T. ) ;
#20260 = CARTESIAN_POINT ( 'NONE',  ( 745.1792804349281596, -422.1908817542430370, 343.7566961878542884 ) ) ;
#20261 = CARTESIAN_POINT ( 'NONE',  ( 744.8212110874229666, -378.8965053807772847, -336.2046728542121627 ) ) ;
#20262 = CARTESIAN_POINT ( 'NONE',  ( 805.0032342141412300, -109.5436935675110988, -314.9967657858571783 ) ) ;
#20263 = AXIS2_PLACEMENT_3D ( 'NONE', #42205, #31116, #31585 ) ;
#20264 = CARTESIAN_POINT ( 'NONE',  ( 790.9844846989617508, -46.37269993606239638, 317.2208543904092721 ) ) ;
#20265 = CARTESIAN_POINT ( 'NONE',  ( 746.8695393053150156, -389.9073299311465348, -327.6429770376306010 ) ) ;
#20266 = DIRECTION ( 'NONE',  ( 0.000000000000000000, -0.6755902076156505842, -0.7372773368101327440 ) ) ;
#20267 = CARTESIAN_POINT ( 'NONE',  ( 770.0799878456142551, -421.9874144716863498, 362.9823548866085616 ) ) ;
#20268 = VERTEX_POINT ( 'NONE', #26675 ) ;
#20269 = CARTESIAN_POINT ( 'NONE',  ( 767.8955696845333705, -264.4527844766016074, 362.1676090361162323 ) ) ;
#20270 = CARTESIAN_POINT ( 'NONE',  ( 795.6651683502461765, -154.7146871989598935, -371.3240766477733814 ) ) ;
#20271 = CARTESIAN_POINT ( 'NONE',  ( 784.9999999999992042, 205.0000000000000568, -265.0000000000000000 ) ) ;
#20272 = CARTESIAN_POINT ( 'NONE',  ( 783.7566961878529810, -288.8965053807775121, 305.1792804349288417 ) ) ;
#20273 = CARTESIAN_POINT ( 'NONE',  ( 756.5762568750052424, -99.18005720387478164, 348.7366044899774238 ) ) ;
#20274 = VERTEX_POINT ( 'NONE', #11917 ) ;
#20275 = CARTESIAN_POINT ( 'NONE',  ( 799.4546378042377910, -9.078323562596708030, -356.1575198192848006 ) ) ;
#20276 = CARTESIAN_POINT ( 'NONE',  ( 794.9819416627830151, -252.9982390220560831, 319.9864689768909898 ) ) ;
#20277 = CARTESIAN_POINT ( 'NONE',  ( 767.7687537140311633, 0.09267006885218045942, -372.7932403749916830 ) ) ;
#20278 = ORIENTED_EDGE ( 'NONE', *, *, #78, .F. ) ;
#20279 = EDGE_LOOP ( 'NONE', ( #36315, #16905, #41774, #8211 ) ) ;
#20280 = CARTESIAN_POINT ( 'NONE',  ( 802.1676090361156639, -182.6346026584199649, -327.8955696845344505 ) ) ;
#20281 = CARTESIAN_POINT ( 'NONE',  ( 760.0363995740630116, -394.9181544815158418, -368.7758568127991907 ) ) ;
#20282 = VECTOR ( 'NONE', #44863, 1000.000000000000000 ) ;
#20283 = CARTESIAN_POINT ( 'NONE',  ( 792.1044303154645831, -252.4527844766015789, -317.8323909638837677 ) ) ;
#20285 = CARTESIAN_POINT ( 'NONE',  ( 768.8385539511368734, -239.2601417444141987, 306.4236121716840557 ) ) ;
#20284 = CARTESIAN_POINT ( 'NONE',  ( 748.9653473494365699, -362.6346026584193964, 356.9462024416520762 ) ) ;
#20286 = CARTESIAN_POINT ( 'NONE',  ( 796.1575198192839480, -270.0090635724253048, -359.4546378042384163 ) ) ;
#20287 = CARTESIAN_POINT ( 'NONE',  ( 781.8018195045266339, -214.2709662947834488, -365.1927285166406705 ) ) ;
#20288 = CARTESIAN_POINT ( 'NONE',  ( 800.0135310231082713, -422.0891481129647218, -325.0180583372163028 ) ) ;
#20289 = CARTESIAN_POINT ( 'NONE',  ( 757.8323909638827445, -242.6346026584197659, 352.1044303154654358 ) ) ;
#20290 = VERTEX_POINT ( 'NONE', #15607 ) ;
#20291 = CARTESIAN_POINT ( 'NONE',  ( 805.0032342141412300, -349.5436935675102745, 314.9967657858571783 ) ) ;
#20292 = AXIS2_PLACEMENT_3D ( 'NONE', #14675, #28519, #28269 ) ;
#20293 = LINE ( 'NONE', #30010, #28486 ) ;
#20294 = CARTESIAN_POINT ( 'NONE',  ( 788.6739635108323228, -7.645427208789786100, -373.9316612368139090 ) ) ;
#20295 = CARTESIAN_POINT ( 'NONE',  ( 794.1255485493337574, 16.45630643248849978, 314.6638991903497526 ) ) ;
#20296 = CARTESIAN_POINT ( 'NONE',  ( -598.8365100919716042, 256.5000000000001705, -199.9999999999899671 ) ) ;
#20297 = VECTOR ( 'NONE', #44937, 1000.000000000000000 ) ;
#20298 = CARTESIAN_POINT ( 'NONE',  ( 805.2837595273609850, -242.7363362996980811, 340.5290396650784714 ) ) ;
#20299 = CARTESIAN_POINT ( 'NONE',  ( 778.1981804954714335, -130.2709662947837899, 314.8072714833589885 ) ) ;
#20300 = ORIENTED_EDGE ( 'NONE', *, *, #36217, .T. ) ;
#20301 = CARTESIAN_POINT ( 'NONE',  ( 762.1177392798416577, -450.5545181178793541, -309.8865473780659272 ) ) ;
#20302 = CARTESIAN_POINT ( 'NONE',  ( 805.0032342141413437, -61.54369356751124798, -314.9967657858572352 ) ) ;
#20303 = CARTESIAN_POINT ( 'NONE',  ( 758.6633372737375112, -260.5328690171413086, 326.9102291470432533 ) ) ;
#20304 = CARTESIAN_POINT ( 'NONE',  ( 804.4286716492782716, -425.3618753856919170, -345.3141322388244703 ) ) ;
#20305 = CARTESIAN_POINT ( 'NONE',  ( 767.8955696845334842, -48.45278447660221133, -362.1676090361161755 ) ) ;
#20306 = CARTESIAN_POINT ( 'NONE',  ( 807.2620300519052989, -0.009063572426172561425, 318.0141637701419768 ) ) ;
#20307 = CARTESIAN_POINT ( 'NONE',  ( -468.8365100919714337, 260.0000000000001705, -208.0249999999908823 ) ) ;
#20308 = CARTESIAN_POINT ( 'NONE',  ( 782.5225473063381969, -214.2709662947834488, -375.2698199232970637 ) ) ;
#20309 = CARTESIAN_POINT ( 'NONE',  ( 745.0891759886404770, -76.27096629478394618, 342.4968714119734159 ) ) ;
#20310 = DIRECTION ( 'NONE',  ( 0.000000000000000000, 0.000000000000000000, 1.000000000000000000 ) ) ;
#20311 = CIRCLE ( 'NONE', #30645, 9.999999999999982236 ) ;
#20312 = CARTESIAN_POINT ( 'NONE',  ( 799.9999999999993179, 205.0000000000000568, -360.0000000000000000 ) ) ;
#20313 = CARTESIAN_POINT ( 'NONE',  ( 748.3538107759620743, -280.7146871989594956, -355.8262568251490165 ) ) ;
#20314 = VECTOR ( 'NONE', #12406, 1000.000000000000000 ) ;
#20315 = CARTESIAN_POINT ( 'NONE',  ( 745.1792804349281596, -422.1908817542430370, 343.7566961878542884 ) ) ;
#20316 = CARTESIAN_POINT ( 'NONE',  ( 759.0252816721024374, -288.9982390220559978, -368.0189434323527280 ) ) ;
#20317 = CARTESIAN_POINT ( 'NONE',  ( -919.9999999999993179, 154.9999999999998863, 350.0000000000000000 ) ) ;
#20318 = CARTESIAN_POINT ( 'NONE',  ( 763.0537975583475827, -408.4527844766009252, 371.0346526505627480 ) ) ;
#20319 = CARTESIAN_POINT ( 'NONE',  ( 792.2312462859673587, -11.90732993114778182, 307.2067596250082602 ) ) ;
#20320 = CARTESIAN_POINT ( 'NONE',  ( 754.8072714833581358, -340.8164208402376971, -338.1981804954720587 ) ) ;
#20321 = CARTESIAN_POINT ( 'NONE',  ( 804.9511171171677688, -29.80559628986937781, 335.8780910478229202 ) ) ;
#20322 = CARTESIAN_POINT ( 'NONE',  ( 815.0009284576459549, -54.35105083532383219, -338.7629533639073429 ) ) ;
#20323 = CARTESIAN_POINT ( 'NONE',  ( 775.9200461376533440, -167.8055962898689586, -315.3028492785443291 ) ) ;
#20324 = CARTESIAN_POINT ( 'NONE',  ( 754.0944755984390895, -183.6237781080507148, 364.1009440267246760 ) ) ;
#20325 = CARTESIAN_POINT ( 'NONE',  ( 762.3223304703356007, 16.45630643248849267, 322.3223304703362828 ) ) ;
#20326 = VECTOR ( 'NONE', #36585, 1000.000000000000000 ) ;
#20327 = ORIENTED_EDGE ( 'NONE', *, *, #30611, .F. ) ;
#20328 = CARTESIAN_POINT ( 'NONE',  ( 755.0636971347428243, -76.27096629478394618, -341.7834795799807353 ) ) ;
#20329 = CARTESIAN_POINT ( 'NONE',  ( 755.0488828828309806, -161.8055962898689870, -344.1219089521771934 ) ) ;
#20330 = CARTESIAN_POINT ( 'NONE',  ( 774.6312213355099630, -167.3618753856927412, 364.6798772138717482 ) ) ;
#20331 = VECTOR ( 'NONE', #43527, 1000.000000000000000 ) ;
#20332 = PRODUCT_DEFINITION_SHAPE ( 'NONE', 'NONE',  #3610 ) ;
#20333 = CARTESIAN_POINT ( 'NONE',  ( 795.6651683502461765, 13.28531280103958423, -371.3240766477733814 ) ) ;
#20335 = CARTESIAN_POINT ( 'NONE',  ( 759.9864689768902508, -290.0891481129650629, 354.9819416627836404 ) ) ;
#20334 = CARTESIAN_POINT ( 'NONE',  ( 758.0580252608178853, -294.4527844766013800, 328.0187753319985404 ) ) ;
#20336 = DIRECTION ( 'NONE',  ( -0.000000000000000000, -1.000000000000000000, 0.000000000000000000 ) ) ;
#20337 = ORIENTED_EDGE ( 'NONE', *, *, #42169, .T. ) ;
#20338 = CARTESIAN_POINT ( 'NONE',  ( 800.7704444035546203, -28.16923265350574468, 326.0291762391768771 ) ) ;
#20339 = CARTESIAN_POINT ( 'NONE',  ( 793.5525998758768083, -295.0999726633343698, -372.6845335610516941 ) ) ;
#20340 = CONTEXT_DEPENDENT_SHAPE_REPRESENTATION ( #25487, #40979 ) ;
#20341 = CARTESIAN_POINT ( 'NONE',  ( 777.4774526936600978, -226.2709662947834488, 304.7301800767028226 ) ) ;
#20342 = CARTESIAN_POINT ( 'NONE',  ( 772.4468031744293057, -345.8272453906069472, 363.8651313633793620 ) ) ;
#20343 = CARTESIAN_POINT ( 'NONE',  ( 799.4546378042377910, -441.0783235625953580, 356.1575198192848006 ) ) ;
#20344 = CARTESIAN_POINT ( 'NONE',  ( 793.0897708529556667, -102.5545181178804057, -361.3366627262616362 ) ) ;
#20345 = CARTESIAN_POINT ( 'NONE',  ( 804.4286716492782716, -113.3618753856929260, -345.3141322388244703 ) ) ;
#20346 = CARTESIAN_POINT ( 'NONE',  ( 797.8594530101009923, -325.5436935675104451, -322.1405469898982119 ) ) ;
#20347 = EDGE_LOOP ( 'NONE', ( #5341, #19656, #30883, #24082 ) ) ;
#20348 = CARTESIAN_POINT ( 'NONE',  ( 771.1735550268778070, -417.1800572038736163, -316.3353852180827630 ) ) ;
#20349 = CARTESIAN_POINT ( 'NONE',  ( 804.9511171171677688, -293.8055962898685607, 335.8780910478229202 ) ) ;
#20350 = AXIS2_PLACEMENT_3D ( 'NONE', #16970, #13963, #27579 ) ;
#20351 = DIRECTION ( 'NONE',  ( 1.000000000000000000, 0.000000000000000000, -0.000000000000000000 ) ) ;
#20352 = CARTESIAN_POINT ( 'NONE',  ( 791.4716058693660443, -452.9681489794448339, -367.7200696026887954 ) ) ;
#20353 = CARTESIAN_POINT ( 'NONE',  ( 766.0291762391763086, -130.9181544815166660, 360.7704444035551319 ) ) ;
#20354 = CARTESIAN_POINT ( 'NONE',  ( 774.6858677611749044, 14.27448825067031812, 315.5713283507209894 ) ) ;
#20355 = ORIENTED_EDGE ( 'NONE', *, *, #17957, .T. ) ;
#20356 = CARTESIAN_POINT ( 'NONE',  ( 804.1009440267234822, -335.4636090269705733, -314.0944755984392600 ) ) ;
#20357 = CARTESIAN_POINT ( 'NONE',  ( 786.2694204179717872, -237.2817908451526421, 305.1769319972829067 ) ) ;
#20358 = CIRCLE ( 'NONE', #5621, 2.749999999999891642 ) ;
#20359 = CARTESIAN_POINT ( 'NONE',  ( 792.1044303154645831, -324.4527844766013231, -317.8323909638837677 ) ) ;
#20360 = SHAPE_REPRESENTATION ( 'Moving Blade Support Base', ( #26858 ), #41617 ) ;
#20361 = LINE ( 'NONE', #34683, #14140 ) ;
#20362 = CARTESIAN_POINT ( 'NONE',  ( 793.0897708529556667, -198.5545181178800647, -361.3366627262616362 ) ) ;
#20363 = EDGE_CURVE ( 'NONE', #29759, #10815, #8232, .T. ) ;
#20364 = CIRCLE ( 'NONE', #27753, 6.118999999999985562 ) ;
#20365 = CARTESIAN_POINT ( 'NONE',  ( 745.0891759886404770, -52.27096629478401724, 342.4968714119734159 ) ) ;
#20366 = DIRECTION ( 'NONE',  ( -1.000000000000000000, 0.000000000000000000, 0.000000000000000000 ) ) ;
#20367 = CARTESIAN_POINT ( 'NONE',  ( 814.9108240113580450, -376.2709662947829656, -337.5031285880265273 ) ) ;
#20368 = CARTESIAN_POINT ( 'NONE',  ( 441.1634899080286232, 229.9999999999999716, -199.9999999999972431 ) ) ;
#20369 = CARTESIAN_POINT ( 'NONE',  ( 805.6418435158337843, -317.4636090269706301, 363.8556311672236916 ) ) ;
#20370 = CARTESIAN_POINT ( 'NONE',  ( 759.9999999999992042, -512.9681489794448908, -339.9999999999999432 ) ) ;
#20371 = CARTESIAN_POINT ( 'NONE',  ( 777.5031285880264704, -286.8164208402378677, 374.9108240113588408 ) ) ;
#20372 = CARTESIAN_POINT ( 'NONE',  ( 763.2262854647970016, -8.634602658420517329, -309.2812353651462445 ) ) ;
#20373 = CARTESIAN_POINT ( 'NONE',  ( 781.8018195045266339, -238.2709662947833920, -365.1927285166406705 ) ) ;
#20374 = CARTESIAN_POINT ( 'NONE',  ( 784.9999999999992042, 205.0000000000000568, -235.0000000000000284 ) ) ;
#20375 = CARTESIAN_POINT ( 'NONE',  ( 764.8639956371174549, -392.0891481129648355, 319.7806653035542013 ) ) ;
#20376 = CARTESIAN_POINT ( 'NONE',  ( 796.1575198192839480, -150.0090635724257027, 359.4546378042384163 ) ) ;
#20377 = CARTESIAN_POINT ( 'NONE',  ( 755.8398074228967971, -43.44195992623296831, -333.4516893846970333 ) ) ;
#20378 = CARTESIAN_POINT ( 'NONE',  ( 801.9858362298568863, -51.07832356259657303, 312.7379699480935642 ) ) ;
#20379 = CARTESIAN_POINT ( 'NONE',  ( 774.6312213355098493, -359.3618753856921444, 364.6798772138717482 ) ) ;
#20380 = PLANE ( 'NONE',  #21792 ) ;
#20381 = CARTESIAN_POINT ( 'NONE',  ( 803.6646147819161570, -425.9073299311463074, 348.8264449731210561 ) ) ;
#20382 = EDGE_LOOP ( 'NONE', ( #7304, #3868, #5039, #26637, #22272, #3880 ) ) ;
#20383 = CARTESIAN_POINT ( 'NONE',  ( 755.5713283507202505, -77.36187538569302546, -334.6858677611754729 ) ) ;
#20384 = AXIS2_PLACEMENT_3D ( 'NONE', #8437, #40535, #22740 ) ;
#20385 = CARTESIAN_POINT ( 'NONE',  ( 763.2154366446407039, -357.6237781080501463, -321.4292242960311228 ) ) ;
#20387 = CARTESIAN_POINT ( 'NONE',  ( 768.0187753319979720, -200.6346026584199365, 318.0580252608186242 ) ) ;
#20386 = CARTESIAN_POINT ( 'NONE',  ( 804.9363028652555840, -208.2709662947835341, 338.2165204200192079 ) ) ;
#20388 = AXIS2_PLACEMENT_3D ( 'NONE', #29306, #18669, #15219 ) ;
#20389 = CARTESIAN_POINT ( 'NONE',  ( 745.1769319972822814, -377.8055962898682765, -346.2694204179732083 ) ) ;
#20390 = FACE_OUTER_BOUND ( 'NONE', #11611, .T. ) ;
#20391 = EDGE_LOOP ( 'NONE', ( #34246, #30979, #44511, #4969 ) ) ;
#20392 = CARTESIAN_POINT ( 'NONE',  ( 778.1981804954714335, -394.2709662947827951, 314.8072714833589885 ) ) ;
#20393 = EDGE_LOOP ( 'NONE', ( #16598, #9559 ) ) ;
#20394 =( LENGTH_UNIT ( ) NAMED_UNIT ( * ) SI_UNIT ( .MILLI., .METRE. ) );
#20395 = VECTOR ( 'NONE', #11057, 1000.000000000000000 ) ;
#20396 = CARTESIAN_POINT ( 'NONE',  ( 814.9108240113580450, -232.2709662947834488, -337.5031285880265273 ) ) ;
#20397 = CARTESIAN_POINT ( 'NONE',  ( 772.5602148656447525, -129.7255117493292289, 305.7998596910095443 ) ) ;
#20398 = ORIENTED_EDGE ( 'NONE', *, *, #5139, .F. ) ;
#20399 = CARTESIAN_POINT ( 'NONE',  ( 792.1044303154646968, -228.4527844766016074, -317.8323909638837677 ) ) ;
#20400 = ORIENTED_EDGE ( 'NONE', *, *, #41017, .F. ) ;
#20401 = CARTESIAN_POINT ( 'NONE',  ( 756.3353852180819104, -341.9073299311465917, -331.1735550268788302 ) ) ;
#20402 = CARTESIAN_POINT ( 'NONE',  ( 800.2193346964447755, 5.001760977943074948, -355.1360043628815788 ) ) ;
#20403 = CARTESIAN_POINT ( 'NONE',  ( 754.8983024940795303, -186.8965053807779668, 336.9254006560228163 ) ) ;
#20405 = CARTESIAN_POINT ( 'NONE',  ( 441.1634899080286232, 259.9999999999999432, -199.9999999999972431 ) ) ;
#20404 = DIRECTION ( 'NONE',  ( 1.000000000000000000, -0.000000000000000000, -0.000000000000000000 ) ) ;
#20406 = CARTESIAN_POINT ( 'NONE',  ( 799.9999999999993179, 205.0000000000000568, 339.9999999999999432 ) ) ;
#20407 = EDGE_CURVE ( 'NONE', #38193, #4037, #23195, .T. ) ;
#20408 = EDGE_LOOP ( 'NONE', ( #299, #31697, #8294, #4237 ) ) ;
#20409 = CARTESIAN_POINT ( 'NONE',  ( 804.8461984189677878, -458.1908817542429802, -336.9566956441385628 ) ) ;
#20410 = CARTESIAN_POINT ( 'NONE',  ( 784.9999999999992042, 205.0000000000000568, -235.0000000000000000 ) ) ;
#20411 = DIRECTION ( 'NONE',  ( -0.000000000000000000, 1.000000000000000000, -0.000000000000000000 ) ) ;
#20412 = ORIENTED_EDGE ( 'NONE', *, *, #38242, .T. ) ;
#20413 = CARTESIAN_POINT ( 'NONE',  ( 764.1737431748507561, -250.3726999360618208, -371.6461892240376415 ) ) ;
#20414 = CARTESIAN_POINT ( 'NONE',  ( 802.2119215644370342, -102.0090635724258448, 367.5423716828165084 ) ) ;
#20415 = AXIS2_PLACEMENT_3D ( 'NONE', #5584, #15994, #23801 ) ;
#20417 = CARTESIAN_POINT ( 'NONE',  ( 803.6646147819161570, -209.9073299311470748, -348.8264449731210561 ) ) ;
#20416 = CARTESIAN_POINT ( 'NONE',  ( 454.7528517110262101, 239.9999999999999716, 350.0000000000000000 ) ) ;
#20418 = CARTESIAN_POINT ( 'NONE',  ( 800.7704444035546203, -412.1692326535045936, -326.0291762391768771 ) ) ;
#20419 = CARTESIAN_POINT ( 'NONE',  ( 815.3608509340175488, -242.7363362996980811, -341.2497674668889545 ) ) ;
#20420 = SURFACE_STYLE_USAGE ( .BOTH. , #27353 ) ;
#20421 = LINE ( 'NONE', #44918, #31915 ) ;
#20422 = CARTESIAN_POINT ( 'NONE',  ( 804.8461984189677878, -74.19088175424410281, -336.9566956441385628 ) ) ;
#20423 = VECTOR ( 'NONE', #15875, 1000.000000000000000 ) ;
#20424 = EDGE_CURVE ( 'NONE', #9048, #40061, #32718, .T. ) ;
#20425 = CARTESIAN_POINT ( 'NONE',  ( 766.9102291470427417, -450.5545181178793541, 318.6633372737382501 ) ) ;
#20426 = CARTESIAN_POINT ( 'NONE',  ( 793.5525998758768083, -367.0999726633342561, 372.6845335610516941 ) ) ;
#20427 = DIRECTION ( 'NONE',  ( 0.000000000000000000, 0.7372773368101421809, -0.6755902076156404812 ) ) ;
#20428 = CARTESIAN_POINT ( 'NONE',  ( 775.9200461376533440, -431.8055962898681059, -315.3028492785443291 ) ) ;
#20429 = CARTESIAN_POINT ( 'NONE',  ( 751.9810565676468741, -290.0891481129650629, -360.9747183278973921 ) ) ;
#20430 = FACE_OUTER_BOUND ( 'NONE', #11550, .T. ) ;
#20431 = CARTESIAN_POINT ( 'NONE',  ( -37.63011601220122770, -544.8427095258973623, -369.9999999999999432 ) ) ;
#20432 = CARTESIAN_POINT ( 'NONE',  ( 792.1044303154645831, -84.45278447660206211, -317.8323909638837677 ) ) ;
#20433 = VECTOR ( 'NONE', #23115, 1000.000000000000000 ) ;
#20434 = CARTESIAN_POINT ( 'NONE',  ( 799.9636004259356241, -214.9181544815164386, 311.2241431872006956 ) ) ;
#20435 = CARTESIAN_POINT ( 'NONE',  ( 761.9338519418445230, -158.5328690171417065, -370.4231160770881957 ) ) ;
#20436 = CARTESIAN_POINT ( 'NONE',  ( 787.5162901302840055, -203.3618753856925991, 305.4481719005792684 ) ) ;
#20437 = CARTESIAN_POINT ( 'NONE',  ( 815.2698199232961542, -400.8164208402373561, -342.5225473063383106 ) ) ;
#20438 = VECTOR ( 'NONE', #29008, 1000.000000000000000 ) ;
#20439 = DIRECTION ( 'NONE',  ( 0.000000000000000000, 0.000000000000000000, -1.000000000000000000 ) ) ;
#20440 = CARTESIAN_POINT ( 'NONE',  ( 802.1676090361156639, -302.6346026584196238, 327.8955696845344505 ) ) ;
#20441 = CARTESIAN_POINT ( 'NONE',  ( 761.4292242960306112, -65.46360902697142592, 323.2154366446414429 ) ) ;
#20442 = EDGE_CURVE ( 'NONE', #24791, #39264, #19515, .T. ) ;
#20443 = CARTESIAN_POINT ( 'NONE',  ( 759.7806653035534055, -438.9982390220553157, -324.8639956371180801 ) ) ;
#20444 = CARTESIAN_POINT ( 'NONE',  ( 879.9999999999992042, 239.9999999999998863, -244.9999999999999716 ) ) ;
#20446 = EDGE_CURVE ( 'NONE', #24418, #17108, #8457, .T. ) ;
#20445 = CARTESIAN_POINT ( 'NONE',  ( 879.9999999999990905, 479.9999999999998863, 199.9999999999999716 ) ) ;
#20448 = CARTESIAN_POINT ( 'NONE',  ( 797.8594530101008786, -325.5436935675105019, 322.1405469898980982 ) ) ;
#20447 = CARTESIAN_POINT ( 'NONE',  ( 754.9735926884551418, -114.3510508353236617, 340.5236548041000333 ) ) ;
#20449 = ORIENTED_EDGE ( 'NONE', *, *, #40670, .F. ) ;
#20450 = CARTESIAN_POINT ( 'NONE',  ( 787.6308680596127942, -275.2601417444140566, -364.1105419155492768 ) ) ;
#20451 = CARTESIAN_POINT ( 'NONE',  ( 788.7366044899766848, -131.9073299311473875, -316.5762568750059813 ) ) ;
#20452 = CARTESIAN_POINT ( 'NONE',  ( 759.7806653035534055, -78.99823902205662307, 324.8639956371180801 ) ) ;
#20453 = CARTESIAN_POINT ( 'NONE',  ( 745.1769319972822814, -257.8055962898686744, -346.2694204179732083 ) ) ;
#20454 = CARTESIAN_POINT ( 'NONE',  ( -829.9999999999992042, 430.0000000000002842, -244.9999999999995168 ) ) ;
#20455 = CARTESIAN_POINT ( 'NONE',  ( 771.2368401574024119, -397.4419599262317320, 374.2805881961240857 ) ) ;
#20456 = VERTEX_POINT ( 'NONE', #9128 ) ;
#20457 = VECTOR ( 'NONE', #33834, 1000.000000000000000 ) ;
#20458 = CARTESIAN_POINT ( 'NONE',  ( 771.1735550268778070, -273.1800572038742985, 316.3353852180827630 ) ) ;
#20459 = CARTESIAN_POINT ( 'NONE',  ( 773.3843516231979720, -61.44195992623291147, -364.4086373105754433 ) ) ;
#20460 = CARTESIAN_POINT ( 'NONE',  ( 788.7366044899766848, -155.9073299311473306, -316.5762568750059813 ) ) ;
#20461 = CARTESIAN_POINT ( 'NONE',  ( 785.3141322388236176, -357.7255117493285184, 364.4286716492789537 ) ) ;
#20462 = CARTESIAN_POINT ( 'NONE',  ( 777.4774526936600978, -106.2709662947838467, -304.7301800767027657 ) ) ;
#20463 = CARTESIAN_POINT ( 'NONE',  ( 778.2165204200184689, -118.8164208402383508, -364.9363028652563230 ) ) ;
#20464 = VERTEX_POINT ( 'NONE', #39890 ) ;
#20465 = CARTESIAN_POINT ( 'NONE',  ( 799.2566176426618085, -48.00906357242602951, -324.0069404352559559 ) ) ;
#20466 = VECTOR ( 'NONE', #4951, 1000.000000000000000 ) ;
#20467 = CARTESIAN_POINT ( 'NONE',  ( 790.0220218866281812, -367.0999726633342561, -363.2186876482849129 ) ) ;
#20468 = EDGE_CURVE ( 'NONE', #30216, #11266, #6217, .T. ) ;
#20470 = CARTESIAN_POINT ( 'NONE',  ( 802.5472867521000353, -412.3726999360612808, 350.8726784830461156 ) ) ;
#20469 = CARTESIAN_POINT ( 'NONE',  ( 803.6646147819161570, -137.9073299311473875, 348.8264449731210561 ) ) ;
#20471 = CARTESIAN_POINT ( 'NONE',  ( 754.8983024940795303, -90.89650538077827946, 336.9254006560228163 ) ) ;
#20474 = CARTESIAN_POINT ( 'NONE',  ( 783.7566961878529810, -360.8965053807773984, 305.1792804349288417 ) ) ;
#20473 = DIRECTION ( 'NONE',  ( 0.000000000000000000, -1.000000000000000000, 0.000000000000000000 ) ) ;
#20472 = CARTESIAN_POINT ( 'NONE',  ( 796.7737145352015204, -452.6346026584191691, 370.7187646348536987 ) ) ;
#20475 = EDGE_CURVE ( 'NONE', #37268, #28399, #22301, .T. ) ;
#20476 = CARTESIAN_POINT ( 'NONE',  ( 752.4576283171824116, -117.0783235625963528, 317.7880784355627952 ) ) ;
#20477 = CARTESIAN_POINT ( 'NONE',  ( 755.1538015810308480, -374.1908817542432075, -343.0433043558613804 ) ) ;
#20478 = CARTESIAN_POINT ( 'NONE',  ( 759.9864689768902508, -362.0891481129648923, -354.9819416627836404 ) ) ;
#20479 = CARTESIAN_POINT ( 'NONE',  ( 766.4474001241216001, -139.0999726633348530, -307.3154664389482491 ) ) ;
#20480 = CARTESIAN_POINT ( 'NONE',  ( 781.2370466360911223, 3.263663700301089765, 304.9990715423533629 ) ) ;
#20482 = PLANE ( 'NONE',  #33614 ) ;
#20481 = CYLINDRICAL_SURFACE ( 'NONE', #7904, 6.118999999999985562 ) ;
#20483 = CARTESIAN_POINT ( 'NONE',  ( 775.9200461376533440, -263.8055962898686175, -315.3028492785443291 ) ) ;
#20484 = CARTESIAN_POINT ( 'NONE',  ( 815.3608509340175488, -170.7363362996983938, -341.2497674668889545 ) ) ;
#20485 = LINE ( 'NONE', #7322, #42199 ) ;
#20486 = DIRECTION ( 'NONE',  ( -0.000000000000000000, 1.000000000000000000, -0.000000000000000000 ) ) ;
#20487 = EDGE_CURVE ( 'NONE', #12435, #27745, #20951, .T. ) ;
#20488 = CARTESIAN_POINT ( 'NONE',  ( 755.1538015810308480, -326.1908817542433781, 343.0433043558613804 ) ) ;
#20489 = CARTESIAN_POINT ( 'NONE',  ( 795.8262568251477660, -286.3726999360617356, 308.3538107759623585 ) ) ;
#20490 = CARTESIAN_POINT ( 'NONE',  ( 751.6929314249750860, -174.9982390220563673, -318.8095938919659034 ) ) ;
#20491 = DIRECTION ( 'NONE',  ( 1.000000000000000000, 0.000000000000000000, 0.000000000000000000 ) ) ;
#20492 = CARTESIAN_POINT ( 'NONE',  ( 793.5525998758768083, -127.0999726633348672, 372.6845335610516941 ) ) ;
#20493 = CARTESIAN_POINT ( 'NONE',  ( 751.6929314249748586, -318.9982390220557704, -318.8095938919659034 ) ) ;
#20494 = DIRECTION ( 'NONE',  ( -0.000000000000000000, -0.000000000000000000, 1.000000000000000000 ) ) ;
#20495 = DIRECTION ( 'NONE',  ( 0.000000000000000000, 0.000000000000000000, -1.000000000000000000 ) ) ;
#20496 = CARTESIAN_POINT ( 'NONE',  ( 757.8323909638827445, -194.6346026584198796, 352.1044303154654358 ) ) ;
#20497 = ORIENTED_EDGE ( 'NONE', *, *, #26039, .F. ) ;
#20498 = CARTESIAN_POINT ( 'NONE',  ( 814.8207195650702488, -410.1908817542430370, 336.2433038121456548 ) ) ;
#20499 = CARTESIAN_POINT ( 'NONE',  ( 748.3538107759620743, -376.7146871989592682, -355.8262568251490165 ) ) ;
#20500 = VECTOR ( 'NONE', #28467, 1000.000000000000000 ) ;
#20501 = CARTESIAN_POINT ( 'NONE',  ( 808.3070685750230950, -114.9982390220565236, -361.1904061080339261 ) ) ;
#20502 = CARTESIAN_POINT ( 'NONE',  ( 755.3028492785439312, -39.28179084515331709, 335.9200461376539693 ) ) ;
#20503 = CARTESIAN_POINT ( 'NONE',  ( 814.9108240113580450, -400.2709662947828519, -337.5031285880265273 ) ) ;
#20505 = EDGE_CURVE ( 'NONE', #38193, #21185, #3295, .T. ) ;
#20504 = DIRECTION ( 'NONE',  ( -0.000000000000000000, 0.000000000000000000, -1.000000000000000000 ) ) ;
#20506 = CARTESIAN_POINT ( 'NONE',  ( 769.1273215169530886, -430.7146871989590409, 317.4527132478988847 ) ) ;
#20507 = ORIENTED_EDGE ( 'NONE', *, *, #9376, .T. ) ;
#20508 = CARTESIAN_POINT ( 'NONE',  ( 764.3348316497523456, -166.7146871989598367, -308.6759233522265617 ) ) ;
#20509 = CARTESIAN_POINT ( 'NONE',  ( 989.9999999999992042, 56.78581973499402835, -212.6378164459127049 ) ) ;
#20510 = CARTESIAN_POINT ( 'NONE',  ( 744.9990715423526808, -258.3510508353231785, 341.2370466360926002 ) ) ;
#20511 = CARTESIAN_POINT ( 'NONE',  ( 759.9864689768902508, -122.0891481129656171, 354.9819416627836404 ) ) ;
#20512 = ORIENTED_EDGE ( 'NONE', *, *, #21338, .T. ) ;
#20513 = CARTESIAN_POINT ( 'NONE',  ( 758.0580252608178853, -270.4527844766014937, 328.0187753319985404 ) ) ;
#20514 = CARTESIAN_POINT ( 'NONE',  ( 748.9653473494363425, -2.634602658420536869, -356.9462024416521331 ) ) ;
#20515 = LINE ( 'NONE', #14051, #2521 ) ;
#20516 = VERTEX_POINT ( 'NONE', #33175 ) ;
#20517 = CARTESIAN_POINT ( 'NONE',  ( 788.6739635108323228, -415.6454272087885897, -373.9316612368139090 ) ) ;
#20518 = ADVANCED_FACE ( 'NONE', ( #15398, #12380, #43551 ), #26457, .F. ) ;
#20519 = CARTESIAN_POINT ( 'NONE',  ( 781.7834795799800531, -250.8164208402379245, -315.0636971347436202 ) ) ;
#20521 = CARTESIAN_POINT ( 'NONE',  ( 815.0009284576459549, -270.3510508353231216, 338.7629533639073429 ) ) ;
#20520 = CARTESIAN_POINT ( 'NONE',  ( 813.1304606946831655, -353.9073299311467053, 352.3570229623691716 ) ) ;
#20522 = CARTESIAN_POINT ( 'NONE',  ( 805.2837595273609850, -266.7363362996981095, -340.5290396650784714 ) ) ;
#20523 = CARTESIAN_POINT ( 'NONE',  ( 765.0180583372156207, -264.9982390220561115, -360.0135310231089534 ) ) ;
#20524 = CARTESIAN_POINT ( 'NONE',  ( 755.3201227861273992, -435.7255117493282341, -345.3687786644892981 ) ) ;
#20525 = CARTESIAN_POINT ( 'NONE',  ( 767.8955696845333705, -72.45278447660213317, -362.1676090361162323 ) ) ;
#20526 = CARTESIAN_POINT ( 'NONE',  ( 768.0187753319979720, -248.6346026584197659, 318.0580252608186242 ) ) ;
#20527 = ORIENTED_EDGE ( 'NONE', *, *, #35398, .F. ) ;
#20528 = CARTESIAN_POINT ( 'NONE',  ( 792.2312462859673587, -347.9073299311467053, 307.2067596250082602 ) ) ;
#20529 = CARTESIAN_POINT ( 'NONE',  ( 959.5497976682736407, 229.9999999999998579, -209.9999999999999716 ) ) ;
#20530 = CARTESIAN_POINT ( 'NONE',  ( 754.3581564841646241, -41.46360902697149697, -316.1443688327762516 ) ) ;
#20531 = CYLINDRICAL_SURFACE ( 'NONE', #41105, 8.024999999999948841 ) ;
#20532 = CARTESIAN_POINT ( 'NONE',  ( 795.2725662613897839, 16.45630643248849267, -314.1785221222716586 ) ) ;
#20533 = CARTESIAN_POINT ( 'NONE',  ( 776.9254006560222479, -236.1908817542436338, 314.8983024940802125 ) ) ;
#20534 = CARTESIAN_POINT ( 'NONE',  ( 794.9819416627830151, -108.9982390220565804, 319.9864689768909898 ) ) ;
#20535 = VERTEX_POINT ( 'NONE', #43767 ) ;
#20536 = CARTESIAN_POINT ( 'NONE',  ( 800.9840315886518738, -28.91815448151699286, -354.1144889064786412 ) ) ;
#20537 = CARTESIAN_POINT ( 'NONE',  ( 796.9462024416508257, -84.45278447660207632, -308.9653473494370246 ) ) ;
#20538 = CARTESIAN_POINT ( 'NONE',  ( 761.2382568024794409, -279.6237781080503737, 356.9571628226838129 ) ) ;
#20539 = CARTESIAN_POINT ( 'NONE',  ( 797.8594530101008786, -445.5436935675098766, -322.1405469898980982 ) ) ;
#20540 = CARTESIAN_POINT ( 'NONE',  ( 805.1927285166399315, -40.81642084023859951, -341.8018195045277707 ) ) ;
#20541 = CARTESIAN_POINT ( 'NONE',  ( 797.8822607201568644, -6.554518117880697048, 370.1134526219340160 ) ) ;
#20542 = CARTESIAN_POINT ( 'NONE',  ( 796.7737145352015204, -188.6346026584199365, -370.7187646348536987 ) ) ;
#20543 = CARTESIAN_POINT ( 'NONE',  ( 311.1634899080286232, 258.0939999999999941, -206.1189999999963050 ) ) ;
#20544 = CARTESIAN_POINT ( 'NONE',  ( 787.4999999999992042, -512.9681489794448908, -339.9999999999999432 ) ) ;
#20545 = CARTESIAN_POINT ( 'NONE',  ( 744.8212110874229666, -258.8965053807777963, -336.2046728542121627 ) ) ;
#20546 = CARTESIAN_POINT ( 'NONE',  ( 791.0478386215596629, -429.8272453906067199, 306.7653713866226326 ) ) ;
#20547 = CARTESIAN_POINT ( 'NONE',  ( 796.9462024416508257, -276.4527844766013800, -308.9653473494370246 ) ) ;
#20548 = DIRECTION ( 'NONE',  ( -0.000000000000000000, -1.000000000000000000, -0.000000000000000000 ) ) ;
#20549 = CARTESIAN_POINT ( 'NONE',  ( 745.7998596910086917, -413.3618753856920307, 332.5602148656461168 ) ) ;
#20550 = CARTESIAN_POINT ( 'NONE',  ( 744.7301800767020268, -28.81642084023863504, 337.4774526936615189 ) ) ;
#20551 = CARTESIAN_POINT ( 'NONE',  ( 808.7758568127978833, -28.16923265350574468, -320.0363995740631822 ) ) ;
#20552 = CARTESIAN_POINT ( 'NONE',  ( 794.9819416627830151, -372.9982390220557704, -319.9864689768909898 ) ) ;
#20553 = CARTESIAN_POINT ( 'NONE',  ( 805.0264073115434940, -30.35105083532391390, 339.4763451958999099 ) ) ;
#20554 = CARTESIAN_POINT ( 'NONE',  ( 773.7943932421234194, -47.80559628986931386, -305.5313806188329409 ) ) ;
#20555 = CARTESIAN_POINT ( 'NONE',  ( 761.2382568024794409, -159.6237781080508285, -356.9571628226838129 ) ) ;
#20556 = CARTESIAN_POINT ( 'NONE',  ( 746.7653713866222915, -161.2601417444143976, 351.0478386215610271 ) ) ;
#20557 = CARTESIAN_POINT ( 'NONE',  ( 771.2633955100217236, 0.09267006885218045942, 363.4237431249939618 ) ) ;
#20558 = AXIS2_PLACEMENT_3D ( 'NONE', #7334, #21410, #32719 ) ;
#20559 = CARTESIAN_POINT ( 'NONE',  ( 811.6461892240364477, -172.7146871989598083, 324.1737431748509835 ) ) ;
#20560 = EDGE_LOOP ( 'NONE', ( #38877, #39328, #40917, #1210 ) ) ;
#20561 = CARTESIAN_POINT ( 'NONE',  ( 788.8264449731200330, -69.18005720387488111, -363.6646147819171233 ) ) ;
#20562 = CARTESIAN_POINT ( 'NONE',  ( 787.6308680596127942, -179.2601417444143692, -364.1105419155492768 ) ) ;
#20563 = PRODUCT_DEFINITION_CONTEXT ( 'detailed design', #38789, 'design' ) ;
#20564 = CARTESIAN_POINT ( 'NONE',  ( 765.0180583372156207, -168.9982390220563673, 360.0135310231089534 ) ) ;
#20565 = CARTESIAN_POINT ( 'NONE',  ( 751.2241431872005251, 7.830767346494148740, -359.9636004259367610 ) ) ;
#20566 = CARTESIAN_POINT ( 'NONE',  ( 829.9999999999992042, -600.0000000000000000, -244.9999999999999716 ) ) ;
#20567 = ORIENTED_EDGE ( 'NONE', *, *, #37668, .T. ) ;
#20568 = CARTESIAN_POINT ( 'NONE',  ( 776.9566956441375396, -12.89650538077851216, 364.8461984189686405 ) ) ;
#20569 = CARTESIAN_POINT ( 'NONE',  ( 768.9521613784389729, -297.8272453906070041, -373.2346286133773106 ) ) ;
#20570 = CARTESIAN_POINT ( 'NONE',  ( 745.0891759886404770, -244.2709662947834204, 342.4968714119734159 ) ) ;
#20571 = CARTESIAN_POINT ( 'NONE',  ( 796.9571628226829034, -335.4636090269705733, 321.2382568024804641 ) ) ;
#20572 = CARTESIAN_POINT ( 'NONE',  ( 783.7566961878529810, 23.10349461922137237, 305.1792804349288417 ) ) ;
#20573 = CARTESIAN_POINT ( 'NONE',  ( 773.4516893846965786, -163.6454272087893003, -315.8398074228977066 ) ) ;
#20574 = CARTESIAN_POINT ( 'NONE',  ( 755.5713283507202505, -149.3618753856928265, -334.6858677611754729 ) ) ;
#20575 = CARTESIAN_POINT ( 'NONE',  ( 778.2165204200184689, -310.8164208402377540, -364.9363028652563230 ) ) ;
#20576 = ORIENTED_EDGE ( 'NONE', *, *, #41103, .F. ) ;
#20577 = B_SPLINE_CURVE_WITH_KNOTS ( 'NONE', 3,
 ( #38763, #35050, #20049, #10123, #38522, #34370, #24198, #38305, #13141, #17271, #27218, #2740, #17521, #31127, #20727, #10568, #24417, #31595 ),
 .UNSPECIFIED., .F., .F.,
 ( 4, 2, 2, 2, 2, 2, 2, 2, 4 ),
 ( 0.5000000000000000000, 0.5621992937191080397, 0.6243985874382160794, 0.6865978811573241192, 0.7487971748764321589, 0.8109964685955401986, 0.8731957623146482383, 0.9353950560337562781, 0.9975943497528643178 ),
 .UNSPECIFIED. ) ;
#20578 = CARTESIAN_POINT ( 'NONE',  ( 784.0799538623451781, -323.8055962898684470, 364.6971507214555572 ) ) ;
#20579 = LINE ( 'NONE', #45541, #41081 ) ;
#20580 = CARTESIAN_POINT ( 'NONE',  ( 761.4292242960306112, -113.4636090269712554, 323.2154366446414429 ) ) ;
#20581 = CARTESIAN_POINT ( 'NONE',  ( 791.9812246680005501, -20.63460265842048003, 361.9419747391813189 ) ) ;
#20582 = ORIENTED_EDGE ( 'NONE', *, *, #25473, .T. ) ;
#20583 = CARTESIAN_POINT ( 'NONE',  ( 815.3608509340175488, -386.7363362996977116, -341.2497674668889545 ) ) ;
#20584 = CARTESIAN_POINT ( 'NONE',  ( 571.1634899080285095, 239.9999999999999716, -202.7499999999980105 ) ) ;
#20585 = CARTESIAN_POINT ( 'NONE',  ( 783.7953271457878373, -248.1908817542435202, 375.1787889125761239 ) ) ;
#20586 = VECTOR ( 'NONE', #34645, 1000.000000000000000 ) ;
#20587 = CARTESIAN_POINT ( 'NONE',  ( 760.5453621957607311, -189.0783235625961822, 323.8424801807151425 ) ) ;
#20588 = CARTESIAN_POINT ( 'NONE',  ( 755.5713283507202505, -341.3618753856922012, -334.6858677611754729 ) ) ;
#20589 = CARTESIAN_POINT ( 'NONE',  ( 769.9779781133707957, -187.0999726633346825, -316.7813123517150871 ) ) ;
#20590 = CARTESIAN_POINT ( 'NONE',  ( 810.7187646348534145, -90.45278447660209054, 356.7737145352016341 ) ) ;
#20591 = CARTESIAN_POINT ( 'NONE',  ( 808.9106007788763009, -452.9681489794446065, 335.7521713694408731 ) ) ;
#20592 = CARTESIAN_POINT ( 'NONE',  ( 767.7687537140311633, -407.9073299311465348, -372.7932403749916830 ) ) ;
#20593 = DIRECTION ( 'NONE',  ( -1.000000000000000000, 0.000000000000000000, 0.000000000000000000 ) ) ;
#20594 = CARTESIAN_POINT ( 'NONE',  ( 814.8207195650702488, -362.1908817542432644, 336.2433038121456548 ) ) ;
#20595 = CARTESIAN_POINT ( 'NONE',  ( -786.4999999999993179, -512.9681489794448908, -350.0000000000000000 ) ) ;
#20596 = CARTESIAN_POINT ( 'NONE',  ( 792.3570229623688874, -309.1800572038740711, 373.1304606946836202 ) ) ;
#20597 = CARTESIAN_POINT ( 'NONE',  ( 745.7998596910086917, -53.36187538569310362, -332.5602148656461168 ) ) ;
#20598 = CARTESIAN_POINT ( 'NONE',  ( 804.4286716492782716, -257.3618753856924286, -345.3141322388244703 ) ) ;
#20599 = FACE_OUTER_BOUND ( 'NONE', #19205, .T. ) ;
#20600 = CARTESIAN_POINT ( 'NONE',  ( 795.1360043628807261, -380.0891481129646650, 360.2193346964456282 ) ) ;
#20601 = CARTESIAN_POINT ( 'NONE',  ( 758.4439275373578084, -156.5545181178802636, 353.2243759319684386 ) ) ;
#20602 = CARTESIAN_POINT ( 'NONE',  ( 791.0478386215596629, -21.82724539060792424, -306.7653713866226326 ) ) ;
#20603 = CARTESIAN_POINT ( 'NONE',  ( 780.5290396650775619, -60.35105083532383219, -365.2837595273619513 ) ) ;
#20604 = CARTESIAN_POINT ( 'NONE',  ( 781.2497674668890113, -60.35105083532383219, 375.3608509340180603 ) ) ;
#20605 = CARTESIAN_POINT ( 'NONE',  ( 785.3141322388236176, -381.7255117493284615, 364.4286716492789537 ) ) ;
#20606 = CARTESIAN_POINT ( 'NONE',  ( 769.9999999999992042, 205.0000000000000568, -319.9999999999999432 ) ) ;
#20607 = DIRECTION ( 'NONE',  ( 0.000000000000000000, 0.000000000000000000, 1.000000000000000000 ) ) ;
#20608 = CARTESIAN_POINT ( 'NONE',  ( 785.3687786644884454, -419.3618753856918033, 315.3201227861279676 ) ) ;
#20609 = ORIENTED_EDGE ( 'NONE', *, *, #39725, .T. ) ;
#20610 = CARTESIAN_POINT ( 'NONE',  ( 800.2193346964447755, -66.99823902205672255, -355.1360043628815788 ) ) ;
#20611 = CARTESIAN_POINT ( 'NONE',  ( 799.4546378042377910, -369.0783235625956422, -356.1575198192848006 ) ) ;
#20613 = CARTESIAN_POINT ( 'NONE',  ( 804.4286716492782716, -185.3618753856926844, 345.3141322388244703 ) ) ;
#20612 = CARTESIAN_POINT ( 'NONE',  ( 755.0636971347428243, -196.2709662947835909, 341.7834795799807353 ) ) ;
#20614 = CARTESIAN_POINT ( 'NONE',  ( 771.2368401574024119, -349.4419599262320162, -374.2805881961240857 ) ) ;
#20615 = CARTESIAN_POINT ( 'NONE',  ( 441.1634899080286232, 239.9999999999999716, -199.9999999999972431 ) ) ;
#20616 = ORIENTED_EDGE ( 'NONE', *, *, #15287, .T. ) ;
#20617 = CARTESIAN_POINT ( 'NONE',  ( 801.9419747391806368, -402.4527844766010389, 351.9812246680014027 ) ) ;
#20618 = AXIS2_PLACEMENT_3D ( 'NONE', #20630, #13031, #34256 ) ;
#20619 = EDGE_LOOP ( 'NONE', ( #11999, #41427, #24368, #43464 ) ) ;
#20620 = CARTESIAN_POINT ( 'NONE',  ( 804.7487373415286811, -211.5436935675107861, -364.7487373415288516 ) ) ;
#20621 = CARTESIAN_POINT ( 'NONE',  ( 745.7998596910086917, -149.3618753856928265, 332.5602148656461168 ) ) ;
#20622 = ORIENTED_EDGE ( 'NONE', *, *, #38917, .T. ) ;
#20624 = EDGE_CURVE ( 'NONE', #38644, #38597, #8907, .T. ) ;
#20623 = CARTESIAN_POINT ( 'NONE',  ( 794.9819416627830151, -204.9982390220562820, -319.9864689768909898 ) ) ;
#20625 = ORIENTED_EDGE ( 'NONE', *, *, #45596, .T. ) ;
#20626 = CARTESIAN_POINT ( 'NONE',  ( 771.1735550268778070, -369.1800572038739574, -316.3353852180827630 ) ) ;
#20627 = CARTESIAN_POINT ( 'NONE',  ( 754.8072714833581358, -28.81642084023863148, -338.1981804954720587 ) ) ;
#20628 = CARTESIAN_POINT ( 'NONE',  ( 759.2295555964440155, -208.1692326535051905, 353.9708237608231229 ) ) ;
#20629 = DIRECTION ( 'NONE',  ( 1.880165489482579047E-16, 1.000000000000000000, 0.000000000000000000 ) ) ;
#20630 = CARTESIAN_POINT ( 'NONE',  ( 779.9999999999992042, -462.9681489794448339, -339.9999999999999432 ) ) ;
#20631 = ORIENTED_EDGE ( 'NONE', *, *, #24693, .F. ) ;
#20632 = CARTESIAN_POINT ( 'NONE',  ( 804.6971507214547046, -459.2817908451519884, -344.0799538623459739 ) ) ;
#20633 = DIRECTION ( 'NONE',  ( 0.000000000000000000, 0.000000000000000000, 1.000000000000000000 ) ) ;
#20634 = CARTESIAN_POINT ( 'NONE',  ( 879.9999999999992042, 99.99999999999984368, 360.0000000000000000 ) ) ;
#20635 = CARTESIAN_POINT ( 'NONE',  ( 807.2620300519052989, -288.0090635724252479, -318.0141637701419768 ) ) ;
#20636 = CARTESIAN_POINT ( 'NONE',  ( 812.3518521366052028, -145.0999726633347677, 326.5853460496235243 ) ) ;
#20638 = CARTESIAN_POINT ( 'NONE',  ( 755.5713283507202505, -221.3618753856925707, -334.6858677611754729 ) ) ;
#20637 = DIRECTION ( 'NONE',  ( 0.000000000000000000, 0.000000000000000000, 1.000000000000000000 ) ) ;
#20639 = CARTESIAN_POINT ( 'NONE',  ( 765.8855110935204493, -406.1692326535045368, -319.0159684113471599 ) ) ;
#20640 = DIRECTION ( 'NONE',  ( -0.000000000000000000, 1.000000000000000000, -0.000000000000000000 ) ) ;
#20641 = CYLINDRICAL_SURFACE ( 'NONE', #5398, 20.00000000000001776 ) ;
#20642 = CARTESIAN_POINT ( 'NONE',  ( 760.7433823573367135, -84.00906357242590161, -355.9930595647440441 ) ) ;
#20643 = ADVANCED_FACE ( 'NONE', ( #44463 ), #16522, .F. ) ;
#20644 = CARTESIAN_POINT ( 'NONE',  ( 811.3240766477731540, -388.3726999360613945, 355.6651683502462902 ) ) ;
#20645 = CARTESIAN_POINT ( 'NONE',  ( 772.4999999999993179, -512.9681489794448908, 309.9999999999998863 ) ) ;
#20646 = CARTESIAN_POINT ( 'NONE',  ( 756.1443688327750579, 2.376221891948710585, -314.3581564841659315 ) ) ;
#20647 = CARTESIAN_POINT ( 'NONE',  ( 745.7998596910086917, -293.3618753856923718, -332.5602148656461168 ) ) ;
#20648 = CARTESIAN_POINT ( 'NONE',  ( -775.4999999999993179, -501.1515549466498669, -368.0974687824633520 ) ) ;
#20649 = CARTESIAN_POINT ( 'NONE',  ( 879.9999999999992042, 429.9999999999999432, -224.9999999999999716 ) ) ;
#20650 = CARTESIAN_POINT ( 'NONE',  ( 797.6776695296629214, -91.54369356751116982, -357.6776695296636603 ) ) ;
#20651 = CARTESIAN_POINT ( 'NONE',  ( 746.4236121716829757, -207.8272453906073451, 328.8385539511384650 ) ) ;
#20652 = CARTESIAN_POINT ( 'NONE',  ( 761.9338519418445230, -182.5328690171416497, -370.4231160770881957 ) ) ;
#20653 = CARTESIAN_POINT ( 'NONE',  ( 787.4397851343537695, -189.7255117493290300, 374.2001403089903988 ) ) ;
#20654 = CARTESIAN_POINT ( 'NONE',  ( 767.7687537140311633, -407.9073299311465348, -372.7932403749916830 ) ) ;
#20655 = LINE ( 'NONE', #20205, #6951 ) ;
#20656 = CARTESIAN_POINT ( 'NONE',  ( 800.0135310231082713, -278.0891481129651197, 325.0180583372163028 ) ) ;
#20657 = CARTESIAN_POINT ( 'NONE',  ( 763.8424801807145741, -66.00906357242595845, 320.5453621957614700 ) ) ;
#20658 = CARTESIAN_POINT ( 'NONE',  ( 785.3141322388236176, -429.7255117493282910, -364.4286716492789537 ) ) ;
#20659 = DIRECTION ( 'NONE',  ( -1.000000000000000000, 1.892425610156518601E-16, 0.000000000000000000 ) ) ;
#20660 = DIRECTION ( 'NONE',  ( -0.000000000000000000, 1.000000000000000000, -0.000000000000000000 ) ) ;
#20662 = CARTESIAN_POINT ( 'NONE',  ( 788.8264449731200330, -309.1800572038740711, 363.6646147819171233 ) ) ;
#20661 = CARTESIAN_POINT ( 'NONE',  ( 794.1144889064781864, -106.1692326535054889, 360.9840315886528401 ) ) ;
#20663 = VERTEX_POINT ( 'NONE', #23881 ) ;
#20664 = ADVANCED_FACE ( 'NONE', ( #27149 ), #9368, .F. ) ;
#20665 = CARTESIAN_POINT ( 'NONE',  ( 776.9566956441375396, -252.8965053807777394, -364.8461984189686405 ) ) ;
#20666 = CARTESIAN_POINT ( 'NONE',  ( 804.6798772138708955, -87.72551174932937101, 334.6312213355107019 ) ) ;
#20667 = CARTESIAN_POINT ( 'NONE',  ( 810.1134526219336749, -272.5328690171413086, -357.8822607201570349 ) ) ;
#20668 = DIRECTION ( 'NONE',  ( 0.000000000000000000, 0.000000000000000000, -1.000000000000000000 ) ) ;
#20669 = CARTESIAN_POINT ( 'NONE',  ( 766.5853460496234675, -397.9874144716864066, 372.3518521366060554 ) ) ;
#20670 = ORIENTED_EDGE ( 'NONE', *, *, #20988, .T. ) ;
#20671 = CARTESIAN_POINT ( 'NONE',  ( 788.7366044899766848, -299.9073299311468759, 316.5762568750059813 ) ) ;
#20672 = CARTESIAN_POINT ( 'NONE',  ( 799.4546378042377910, -33.07832356259662987, -356.1575198192848006 ) ) ;
#20673 = CARTESIAN_POINT ( 'NONE',  ( 756.5762568750052424, -171.1800572038745543, -348.7366044899774238 ) ) ;
#20674 = CARTESIAN_POINT ( 'NONE',  ( 755.0636971347428243, -196.2709662947835909, -341.7834795799807353 ) ) ;
#20675 = CARTESIAN_POINT ( 'NONE',  ( 804.9363028652555840, -424.2709662947829088, 338.2165204200192079 ) ) ;
#20676 = EDGE_CURVE ( 'NONE', #32443, #11154, #2420, .T. ) ;
#20677 = CARTESIAN_POINT ( 'NONE',  ( 751.6929314249748586, -126.9982390220565094, -318.8095938919659034 ) ) ;
#20678 = CARTESIAN_POINT ( 'NONE',  ( 795.1360043628808398, -116.0891481129656313, -360.2193346964456282 ) ) ;
#20679 = VERTEX_POINT ( 'NONE', #17197 ) ;
#20680 = CARTESIAN_POINT ( 'NONE',  ( 800.9840315886518738, -28.91815448151699286, -354.1144889064786412 ) ) ;
#20681 = CARTESIAN_POINT ( 'NONE',  ( 775.8780910478218402, -393.2817908451522726, -364.9511171171680530 ) ) ;
#20683 = CARTESIAN_POINT ( 'NONE',  ( 761.4292242960306112, -425.4636090269703459, 323.2154366446414429 ) ) ;
#20682 = CARTESIAN_POINT ( 'NONE',  ( 803.4237431249931660, -135.1800572038746679, 331.2633955100225194 ) ) ;
#20686 = CARTESIAN_POINT ( 'NONE',  ( 815.1787889125755555, -342.8965053807773984, 343.7953271457877804 ) ) ;
#20685 = CARTESIAN_POINT ( 'NONE',  ( 759.9999999999992042, -512.9681489794448908, 309.9999999999998863 ) ) ;
#20684 = DIRECTION ( 'NONE',  ( 0.000000000000000000, -0.9235249282889858025, -0.3835384033298669948 ) ) ;
#20687 = ORIENTED_EDGE ( 'NONE', *, *, #42896, .T. ) ;
#20688 = CARTESIAN_POINT ( 'NONE',  ( 757.0176451133909268, -349.0999726633342561, -349.9200121543848354 ) ) ;
#20689 = CARTESIAN_POINT ( 'NONE',  ( 756.3353852180819104, -341.9073299311465917, -331.1735550268788302 ) ) ;
#20690 = CARTESIAN_POINT ( 'NONE',  ( 746.4236121716829757, -135.8272453906076009, -328.8385539511384650 ) ) ;
#20691 = CARTESIAN_POINT ( 'NONE',  ( 786.2694204179717872, -45.28179084515329578, 305.1769319972829067 ) ) ;
#20693 = CARTESIAN_POINT ( 'NONE',  ( 794.9999999999993179, 205.0000000000000568, -235.0000000000000284 ) ) ;
#20692 = CARTESIAN_POINT ( 'NONE',  ( 571.1634899080285095, 259.9999999999999432, -193.8809999999981528 ) ) ;
#20694 = CARTESIAN_POINT ( 'NONE',  ( 769.1273215169530886, -286.7146871989594388, -317.4527132478988847 ) ) ;
#20695 = EDGE_CURVE ( 'NONE', #44609, #9031, #41641, .T. ) ;
#20696 = CARTESIAN_POINT ( 'NONE',  ( 807.2620300519052989, -144.0090635724257027, -318.0141637701419768 ) ) ;
#20697 = CARTESIAN_POINT ( 'NONE',  ( 799.9999999999993179, -512.9681489794448908, -339.9999999999999432 ) ) ;
#20698 = DIRECTION ( 'NONE',  ( -1.880165489482579047E-16, -1.000000000000000000, -0.000000000000000000 ) ) ;
#20699 = CARTESIAN_POINT ( 'NONE',  ( 763.8424801807145741, -330.0090635724251342, 320.5453621957614700 ) ) ;
#20700 = CARTESIAN_POINT ( 'NONE',  ( 754.3581564841646241, -305.4636090269706870, 316.1443688327762516 ) ) ;
#20701 = CARTESIAN_POINT ( 'NONE',  ( 782.4968714119720516, -178.8164208402381519, -305.0891759886411023 ) ) ;
#20702 = CARTESIAN_POINT ( 'NONE',  ( -454.7528517110260964, 200.0000000000001137, -122.7905160835438068 ) ) ;
#20703 = CARTESIAN_POINT ( 'NONE',  ( 773.7305795820266212, -105.2817908451530968, 374.8230680027170365 ) ) ;
#20704 = CARTESIAN_POINT ( 'NONE',  ( 772.5602148656447525, -297.7255117493286889, -305.7998596910095443 ) ) ;
#20705 = CARTESIAN_POINT ( 'NONE',  ( 571.1634899080285095, 239.9999999999999716, -197.2499999999982947 ) ) ;
#20706 = CARTESIAN_POINT ( 'NONE',  ( -879.9999999999992042, 430.0000000000002842, -224.9999999999999716 ) ) ;
#20707 = CARTESIAN_POINT ( 'NONE',  ( 757.8323909638827445, -170.6346026584199649, 352.1044303154654358 ) ) ;
#20708 = ORIENTED_EDGE ( 'NONE', *, *, #34245, .F. ) ;
#20709 = CARTESIAN_POINT ( 'NONE',  ( 812.3518521366052028, -433.0999726633339151, 326.5853460496235243 ) ) ;
#20710 = CARTESIAN_POINT ( 'NONE',  ( 752.4576283171824116, -381.0783235625954717, -317.7880784355627952 ) ) ;
#20711 = CARTESIAN_POINT ( 'NONE',  ( 801.1904061080336987, -140.0891481129654892, -368.3070685750235498 ) ) ;
#20712 = EDGE_CURVE ( 'NONE', #10766, #17501, #44702, .T. ) ;
#20713 = CARTESIAN_POINT ( 'NONE',  ( 800.9747183278959710, -372.9982390220557704, -311.9810565676471583 ) ) ;
#20714 = PLANE ( 'NONE',  #359 ) ;
#20715 = CARTESIAN_POINT ( 'NONE',  ( 756.1443688327750579, 2.376221891948710585, 314.3581564841659315 ) ) ;
#20716 = ORIENTED_EDGE ( 'NONE', *, *, #17129, .F. ) ;
#20717 = EDGE_CURVE ( 'NONE', #30506, #41883, #42363, .T. ) ;
#20718 = CARTESIAN_POINT ( 'NONE',  ( 813.2346286133761168, -149.2601417444144261, -328.9521613784389160 ) ) ;
#20719 = CARTESIAN_POINT ( 'NONE',  ( 919.9999999999993179, 154.9999999999998863, 360.0000000000000000 ) ) ;
#20720 = CARTESIAN_POINT ( 'NONE',  ( 744.9990715423526808, -282.3510508353230080, 341.2370466360926002 ) ) ;
#20721 = CARTESIAN_POINT ( 'NONE',  ( 771.1735550268780344, -129.1800572038746679, 316.3353852180828198 ) ) ;
#20722 = VERTEX_POINT ( 'NONE', #37536 ) ;
#20723 = EDGE_CURVE ( 'NONE', #9965, #31705, #2197, .T. ) ;
#20724 = CARTESIAN_POINT ( 'NONE',  ( 755.3201227861273992, -291.7255117493285752, 345.3687786644892981 ) ) ;
#20725 = EDGE_CURVE ( 'NONE', #3824, #17451, #5895, .T. ) ;
#20726 = CARTESIAN_POINT ( 'NONE',  ( 810.7187646348534145, -18.45278447660230725, -356.7737145352016341 ) ) ;
#20727 = CARTESIAN_POINT ( 'NONE',  ( 789.5207239089294262, -450.4903526743926250, 363.8345956117046285 ) ) ;
#20728 = VERTEX_POINT ( 'NONE', #9595 ) ;
#20729 = CARTESIAN_POINT ( 'NONE',  ( 745.5313806188320314, -399.2817908451522726, -333.7943932421247268 ) ) ;
#20730 = CARTESIAN_POINT ( 'NONE',  ( 771.2633955100217236, -23.90732993114773919, 363.4237431249939618 ) ) ;
#20731 = CARTESIAN_POINT ( 'NONE',  ( 764.8639956371174549, -272.0891481129651197, -319.7806653035542013 ) ) ;
#20733 = CARTESIAN_POINT ( 'NONE',  ( 808.7758568127978833, -244.1692326535050768, 320.0363995740631822 ) ) ;
#20732 = CARTESIAN_POINT ( 'NONE',  ( 787.5162901302840055, -371.3618753856920307, 305.4481719005793252 ) ) ;
#20734 = CARTESIAN_POINT ( 'NONE',  ( 815.0009284576459549, -54.35105083532383219, 338.7629533639073429 ) ) ;
#20735 = CARTESIAN_POINT ( 'NONE',  ( 779.4763451958990572, -248.7363362996981380, -365.0264073115438919 ) ) ;
#20736 = CARTESIAN_POINT ( 'NONE',  ( 778.2165204200184689, -262.8164208402379245, -364.9363028652563230 ) ) ;
#20737 = DIRECTION ( 'NONE',  ( -0.000000000000000000, 1.000000000000000000, -0.000000000000000000 ) ) ;
#20738 = CARTESIAN_POINT ( 'NONE',  ( 785.3141322388236176, -93.72551174932934259, -364.4286716492789537 ) ) ;
#20739 = EDGE_CURVE ( 'NONE', #10345, #9331, #27830, .T. ) ;
#20740 = CARTESIAN_POINT ( 'NONE',  ( 774.6858677611749044, -249.7255117493288594, 315.5713283507209894 ) ) ;
#20741 = CARTESIAN_POINT ( 'NONE',  ( 782.4968714119720516, -370.8164208402375834, 305.0891759886411023 ) ) ;
#20742 = CARTESIAN_POINT ( 'NONE',  ( -829.9999999999994316, 579.9999999999998863, -320.0000000000000000 ) ) ;
#20743 = ADVANCED_FACE ( 'NONE', ( #9814 ), #16289, .F. ) ;
#20744 = CARTESIAN_POINT ( 'NONE',  ( 815.3608509340175488, -50.73633629969874193, -341.2497674668889545 ) ) ;
#20745 = DIRECTION ( 'NONE',  ( 0.000000000000000000, 0.000000000000000000, 1.000000000000000000 ) ) ;
#20746 = CARTESIAN_POINT ( 'NONE',  ( -728.8365100919714905, 230.0000000000001705, -197.2499999999891998 ) ) ;
#20747 = CARTESIAN_POINT ( 'NONE',  ( 759.0159684113467620, -232.9181544815163249, 325.8855110935213020 ) ) ;
#20748 = APPLICATION_CONTEXT ( 'automotive_design' ) ;
#20749 = CARTESIAN_POINT ( 'NONE',  ( 758.0580252608178853, -126.4527844766019626, 328.0187753319985404 ) ) ;
#20750 = VERTEX_POINT ( 'NONE', #34060 ) ;
#20751 = CARTESIAN_POINT ( 'NONE',  ( 804.6971507214547046, -27.28179084515336328, -344.0799538623459739 ) ) ;
#20752 = CIRCLE ( 'NONE', #13386, 8.025000000000003908 ) ;
#20753 = CARTESIAN_POINT ( 'NONE',  ( 804.7487373415286811, -67.54369356751125508, -364.7487373415288516 ) ) ;
#20754 = CARTESIAN_POINT ( 'NONE',  ( 799.4546378042377910, -297.0783235625957559, 356.1575198192848006 ) ) ;
#20755 = CARTESIAN_POINT ( 'NONE',  ( 771.1735550268778070, -441.1800572038735027, -316.3353852180827630 ) ) ;
#20756 = CARTESIAN_POINT ( 'NONE',  ( 750.9282345327678740, -16.91815448151702839, 319.8311093483690115 ) ) ;
#20757 = CARTESIAN_POINT ( 'NONE',  ( 812.7932403749906598, -207.1800572038744406, -327.7687537140311633 ) ) ;
#20758 = CARTESIAN_POINT ( 'NONE',  ( 755.2512626584698410, -175.5436935675108998, 315.2512626584710915 ) ) ;
#20759 = CARTESIAN_POINT ( 'NONE',  ( 755.5713283507202505, -77.36187538569302546, 334.6858677611754729 ) ) ;
#20760 = DIRECTION ( 'NONE',  ( -0.000000000000000000, 1.000000000000000000, -1.056348263647623421E-15 ) ) ;
#20761 = DIRECTION ( 'NONE',  ( 0.000000000000000000, 0.000000000000000000, 1.000000000000000000 ) ) ;
#20762 = ADVANCED_FACE ( 'NONE', ( #38001, #6357 ), #38230, .F. ) ;
#20763 = CARTESIAN_POINT ( 'NONE',  ( 776.2433038121456548, -276.8965053807776258, -374.8207195650711014 ) ) ;
#20764 = EDGE_CURVE ( 'NONE', #5117, #44956, #40908, .T. ) ;
#20765 = CARTESIAN_POINT ( 'NONE',  ( 747.6481478633932056, -421.0999726633340288, 353.4146539503763620 ) ) ;
#20766 = CARTESIAN_POINT ( 'NONE',  ( 759.0252816721024374, -264.9982390220561115, -368.0189434323527280 ) ) ;
#20767 = CARTESIAN_POINT ( 'NONE',  ( 758.7867965644026071, 16.45630643248849267, -318.7867965644036303 ) ) ;
#20768 = CARTESIAN_POINT ( 'NONE',  ( 770.0799878456142551, -349.9874144716865771, 362.9823548866085616 ) ) ;
#20769 = CARTESIAN_POINT ( 'NONE',  ( 747.2067596250078623, -51.18005720387493085, 352.2312462859687230 ) ) ;
#20770 = CARTESIAN_POINT ( 'NONE',  ( 771.2633955100217236, -383.9073299311466485, -363.4237431249939618 ) ) ;
#20771 = EDGE_CURVE ( 'NONE', #34249, #31022, #20655, .T. ) ;
#20772 = CARTESIAN_POINT ( 'NONE',  ( 786.6156483768007774, -25.44195992623301450, 315.5913626894246136 ) ) ;
#20773 = CARTESIAN_POINT ( 'NONE',  ( 744.8212110874229666, -66.89650538077835051, -336.2046728542121627 ) ) ;
#20774 = CARTESIAN_POINT ( 'NONE',  ( 804.1601925771018387, -175.4419599262325562, -346.5483106153029098 ) ) ;
#20775 = CARTESIAN_POINT ( 'NONE',  ( 747.3154664389472828, -187.9874144716870603, 326.4474001241230781 ) ) ;
#20776 = CARTESIAN_POINT ( 'NONE',  ( 788.7366044899766848, -11.90732993114778182, 316.5762568750059813 ) ) ;
#20777 = ORIENTED_EDGE ( 'NONE', *, *, #30930, .F. ) ;
#20778 = CARTESIAN_POINT ( 'NONE',  ( 800.2193346964447755, -66.99823902205672255, -355.1360043628815788 ) ) ;
#20779 = CARTESIAN_POINT ( 'NONE',  ( 775.9200461376533440, -215.8055962898687881, -315.3028492785443291 ) ) ;
#20780 = CARTESIAN_POINT ( 'NONE',  ( 778.1981804954714335, -154.2709662947836478, 314.8072714833589885 ) ) ;
#20781 = CARTESIAN_POINT ( 'NONE',  ( 801.9858362298568863, -3.078323562596726681, -312.7379699480935642 ) ) ;
#20782 = CARTESIAN_POINT ( 'NONE',  ( 803.4237431249931660, -327.1800572038741279, 331.2633955100225194 ) ) ;
#20783 = CARTESIAN_POINT ( 'NONE',  ( 799.9999999999993179, 205.0000000000000568, 339.9999999999999432 ) ) ;
#20784 = ORIENTED_EDGE ( 'NONE', *, *, #31927, .T. ) ;
#20785 = CARTESIAN_POINT ( 'NONE',  ( 803.2186876482843445, -31.98741447168754348, 350.0220218866286928 ) ) ;
#20786 = CARTESIAN_POINT ( 'NONE',  ( 760.0363995740630116, -298.9181544815161828, -368.7758568127991907 ) ) ;
#20787 = CARTESIAN_POINT ( 'NONE',  ( 749.2812353651451076, -270.4527844766014937, 323.2262854647983090 ) ) ;
#20788 = CARTESIAN_POINT ( 'NONE',  ( 766.0291762391763086, -346.9181544815160123, 360.7704444035551319 ) ) ;
#20789 = CARTESIAN_POINT ( 'NONE',  ( 756.7813123517142913, -427.9874144716862929, 329.9779781133712504 ) ) ;
#20790 = CARTESIAN_POINT ( 'NONE',  ( 755.3028492785439312, -135.2817908451530116, -335.9200461376539693 ) ) ;
#20791 = CARTESIAN_POINT ( 'NONE',  ( 804.9363028652555840, -136.2709662947837330, -338.2165204200192079 ) ) ;
#20792 = CARTESIAN_POINT ( 'NONE',  ( 788.7366044899766848, -323.9073299311468190, -316.5762568750059813 ) ) ;
#20793 = ORIENTED_EDGE ( 'NONE', *, *, #41855, .T. ) ;
#20794 = CARTESIAN_POINT ( 'NONE',  ( 803.2186876482843445, -319.9874144716866340, 350.0220218866286928 ) ) ;
#20795 = CARTESIAN_POINT ( 'NONE',  ( 939.9999999999992042, 240.0000000000000568, -210.0000000000000000 ) ) ;
#20796 = CARTESIAN_POINT ( 'NONE',  ( 760.7433823573367135, -132.0090635724257595, 355.9930595647440441 ) ) ;
#20797 = CARTESIAN_POINT ( 'NONE',  ( 794.9819416627830151, -12.99823902205686821, 319.9864689768909898 ) ) ;
#20798 = ORIENTED_EDGE ( 'NONE', *, *, #13176, .F. ) ;
#20799 = CARTESIAN_POINT ( 'NONE',  ( 778.7629533639073998, -368.7363362996977685, -375.0009284576466371 ) ) ;
#20800 = CARTESIAN_POINT ( 'NONE',  ( 772.4999999999993179, -462.9681489794447202, 270.0000000000000568 ) ) ;
#20801 = CARTESIAN_POINT ( 'NONE',  ( 809.0717654672305343, -220.9181544815164102, 360.1688906516309885 ) ) ;
#20802 = CARTESIAN_POINT ( 'NONE',  ( 763.2154366446407039, -189.6237781080507148, 321.4292242960311228 ) ) ;
#20803 = CARTESIAN_POINT ( 'NONE',  ( 771.2633955100217236, -311.9073299311468759, -363.4237431249939618 ) ) ;
#20804 = SURFACE_STYLE_FILL_AREA ( #28198 ) ;
#20805 = CARTESIAN_POINT ( 'NONE',  ( 790.9844846989617508, -214.3726999360618493, -317.2208543904092721 ) ) ;
#20806 = CARTESIAN_POINT ( 'NONE',  ( 787.4397851343537695, 2.274488250670355871, 374.2001403089903988 ) ) ;
#20807 = CARTESIAN_POINT ( 'NONE',  ( 745.7998596910086917, -77.36187538569302546, 332.5602148656461168 ) ) ;
#20808 = AXIS2_PLACEMENT_3D ( 'NONE', #7770, #14712, #39418 ) ;
#20809 = CARTESIAN_POINT ( 'NONE',  ( 807.4745771775690173, -452.9681489794449476, 340.5093320845589346 ) ) ;
#20810 = CARTESIAN_POINT ( 'NONE',  ( 796.7737145352015204, -428.6346026584192259, -370.7187646348536987 ) ) ;
#20811 = DIRECTION ( 'NONE',  ( -1.000000000000000000, -0.000000000000000000, -0.000000000000000000 ) ) ;
#20812 = CARTESIAN_POINT ( 'NONE',  ( 811.3240766477731540, -340.3726999360615082, 355.6651683502462902 ) ) ;
#20813 = CARTESIAN_POINT ( 'NONE',  ( 794.9285562942586694, -457.5945560043289788, -366.0218793896430043 ) ) ;
#20814 = CARTESIAN_POINT ( 'NONE',  ( 787.5162901302840055, -299.3618753856922581, 305.4481719005792684 ) ) ;
#20815 = CARTESIAN_POINT ( 'NONE',  ( 782.5225473063381969, -70.27096629478397460, -375.2698199232970637 ) ) ;
#20816 = CARTESIAN_POINT ( 'NONE',  ( 781.8018195045266339, -286.2709662947833635, -365.1927285166406705 ) ) ;
#20817 = FACE_BOUND ( 'NONE', #3948, .T. ) ;
#20818 = CARTESIAN_POINT ( 'NONE',  ( 800.2193346964447755, -402.9982390220555430, 355.1360043628815788 ) ) ;
#20819 = CARTESIAN_POINT ( 'NONE',  ( 804.8461984189677878, -146.1908817542438896, 336.9566956441385628 ) ) ;
#20820 = CARTESIAN_POINT ( 'NONE',  ( 814.2805881961230625, -25.64542720878973014, -331.2368401574024119 ) ) ;
#20821 = CARTESIAN_POINT ( 'NONE',  ( 759.2295555964440155, -40.16923265350570915, -353.9708237608231229 ) ) ;
#20822 = CARTESIAN_POINT ( 'NONE',  ( 791.1614460488616487, -59.26014174441473870, 373.5763878283158874 ) ) ;
#20823 = CARTESIAN_POINT ( 'NONE',  ( 802.1676090361155502, -398.6346026584193396, 327.8955696845344505 ) ) ;
#20824 = CARTESIAN_POINT ( 'NONE',  ( 800.9747183278959710, 11.00176097794305541, 311.9810565676471583 ) ) ;
#20825 = FACE_OUTER_BOUND ( 'NONE', #20887, .T. ) ;
#20826 = CARTESIAN_POINT ( 'NONE',  ( 805.1927285166397041, -424.8164208402372992, 341.8018195045277707 ) ) ;
#20828 = ORIENTED_EDGE ( 'NONE', *, *, #10242, .F. ) ;
#20827 = CARTESIAN_POINT ( 'NONE',  ( 805.1016975059191054, -102.8965053807782368, -343.0745993439771837 ) ) ;
#20829 = CARTESIAN_POINT ( 'NONE',  ( 785.3687786644884454, -59.36187538569306810, -315.3201227861279676 ) ) ;
#20830 = CARTESIAN_POINT ( 'NONE',  ( 793.2243759319678702, -362.5328690171410813, -318.4439275373583200 ) ) ;
#20832 = CARTESIAN_POINT ( 'NONE',  ( 755.0636971347428243, -196.2709662947835909, 341.7834795799807353 ) ) ;
#20831 = CARTESIAN_POINT ( 'NONE',  ( 765.0180583372156207, -240.9982390220561683, 360.0135310231089534 ) ) ;
#20833 = VECTOR ( 'NONE', #33002, 1000.000000000000114 ) ;
#20834 = ORIENTED_EDGE ( 'NONE', *, *, #26387, .T. ) ;
#20835 = CARTESIAN_POINT ( 'NONE',  ( 803.8556311672234642, -393.6237781080500326, -365.6418435158340117 ) ) ;
#20836 = FACE_OUTER_BOUND ( 'NONE', #39457, .T. ) ;
#20837 = ORIENTED_EDGE ( 'NONE', *, *, #37974, .F. ) ;
#20838 = CARTESIAN_POINT ( 'NONE',  ( 765.0180583372156207, -408.9982390220556567, 360.0135310231089534 ) ) ;
#20839 = VERTEX_POINT ( 'NONE', #34747 ) ;
#20840 = SHAPE_REPRESENTATION_RELATIONSHIP ( 'NONE' , 'NONE' ,  #20360, #14437 ) ;
#20841 = CARTESIAN_POINT ( 'NONE',  ( 787.5162901302840055, -251.3618753856923149, -305.4481719005792684 ) ) ;
#20842 = CARTESIAN_POINT ( 'NONE',  ( 744.7301800767020268, -148.8164208402382656, 337.4774526936615189 ) ) ;
#20843 = ORIENTED_EDGE ( 'NONE', *, *, #43599, .F. ) ;
#20844 = VECTOR ( 'NONE', #27574, 999.9999999999998863 ) ;
#20845 = CARTESIAN_POINT ( 'NONE',  ( 788.7366044899766848, -227.9073299311471033, -316.5762568750059813 ) ) ;
#20846 = ORIENTED_EDGE ( 'NONE', *, *, #10865, .F. ) ;
#20847 = CARTESIAN_POINT ( 'NONE',  ( 755.5713283507202505, -365.3618753856920875, -334.6858677611754729 ) ) ;
#20848 = CARTESIAN_POINT ( 'NONE',  ( 774.6858677611749044, -9.725511749329603717, -315.5713283507209894 ) ) ;
#20849 = CARTESIAN_POINT ( 'NONE',  ( 803.2186876482843445, -223.9874144716869182, 350.0220218866286928 ) ) ;
#20850 = CARTESIAN_POINT ( 'NONE',  ( 787.4999999999992042, -462.9681489794447202, 270.0000000000000568 ) ) ;
#20851 = CYLINDRICAL_SURFACE ( 'NONE', #11044, 10.00000000000000888 ) ;
#20852 = ORIENTED_EDGE ( 'NONE', *, *, #17049, .T. ) ;
#20853 = CARTESIAN_POINT ( 'NONE',  ( 762.3223304703356007, 16.45630643248849267, -322.3223304703362828 ) ) ;
#20854 = DIRECTION ( 'NONE',  ( 0.000000000000000000, 0.000000000000000000, 1.000000000000000000 ) ) ;
#20855 = LINE ( 'NONE', #17653, #35159 ) ;
#20856 = VERTEX_POINT ( 'NONE', #34530 ) ;
#20857 = CARTESIAN_POINT ( 'NONE',  ( 771.3260364891663130, -283.6454272087889308, -306.0683387631859773 ) ) ;
#20858 = CARTESIAN_POINT ( 'NONE',  ( 810.4231160770870019, -144.5545181178802636, 321.9338519418446936 ) ) ;
#20860 = CARTESIAN_POINT ( 'NONE',  ( 801.9419747391806368, -234.4527844766016358, -351.9812246680014027 ) ) ;
#20859 = CARTESIAN_POINT ( 'NONE',  ( 989.9999999999992042, 62.85347435602256638, 357.4246812887967053 ) ) ;
#20861 = CARTESIAN_POINT ( 'NONE',  ( 801.3366627262608972, -392.5328690171409107, -353.0897708529566899 ) ) ;
#20862 = DIRECTION ( 'NONE',  ( 0.000000000000000000, 0.000000000000000000, 1.000000000000000000 ) ) ;
#20863 = LINE ( 'NONE', #3334, #25329 ) ;
#20864 = CARTESIAN_POINT ( 'NONE',  ( 800.9840315886518738, -124.9181544815167086, -354.1144889064786412 ) ) ;
#20865 = CARTESIAN_POINT ( 'NONE',  ( 755.8990559732751535, -371.4636090269705164, 365.9055244015606831 ) ) ;
#20866 = AXIS2_PLACEMENT_3D ( 'NONE', #19281, #29467, #18853 ) ;
#20867 = PLANE ( 'NONE',  #27638 ) ;
#20868 = CARTESIAN_POINT ( 'NONE',  ( 756.1443688327750579, 26.37622189194863509, -314.3581564841659315 ) ) ;
#20869 = CARTESIAN_POINT ( 'NONE',  ( 815.2698199232962679, -328.8164208402375834, -342.5225473063383674 ) ) ;
#20870 = DIRECTION ( 'NONE',  ( -1.880165489482579047E-16, -1.000000000000000000, -0.000000000000000000 ) ) ;
#20871 = DIRECTION ( 'NONE',  ( 1.000000000000000000, 0.000000000000000000, 0.000000000000000000 ) ) ;
#20872 = CARTESIAN_POINT ( 'NONE',  ( 757.8323909638827445, -74.63460265842032015, -352.1044303154654358 ) ) ;
#20873 = AXIS2_PLACEMENT_3D ( 'NONE', #34186, #36765, #15742 ) ;
#20874 = CARTESIAN_POINT ( 'NONE',  ( 797.8822607201568644, -246.5545181178799510, 370.1134526219340160 ) ) ;
#20875 = CARTESIAN_POINT ( 'NONE',  ( 815.0009284576459549, -198.3510508353234059, -338.7629533639073429 ) ) ;
#20876 = CARTESIAN_POINT ( 'NONE',  ( 808.3070685750230950, -186.9982390220563104, 361.1904061080339261 ) ) ;
#20877 = CARTESIAN_POINT ( 'NONE',  ( 745.4481719005789273, -435.7255117493282341, -347.5162901302853129 ) ) ;
#20878 = CARTESIAN_POINT ( 'NONE',  ( 879.9999999999992042, 239.9999999999998863, -244.9999999999999716 ) ) ;
#20879 = CARTESIAN_POINT ( 'NONE',  ( 762.1405469898971887, -289.5436935675103882, 357.8594530101015607 ) ) ;
#20880 = CARTESIAN_POINT ( 'NONE',  ( 755.8894580844503253, -87.82724539060770041, 332.3691319403863531 ) ) ;
#20881 = CARTESIAN_POINT ( 'NONE',  ( 759.9864689768902508, -410.0891481129647218, -354.9819416627836404 ) ) ;
#20882 = CARTESIAN_POINT ( 'NONE',  ( 51.16348990802859475, 260.0000000000000568, -199.9999999999945146 ) ) ;
#20883=STYLED_ITEM('',(#45744),#32965);
#20884 = CARTESIAN_POINT ( 'NONE',  ( 441.1634899080286232, 258.0939999999999372, -193.8809999999972433 ) ) ;
#20886 = CARTESIAN_POINT ( 'NONE',  ( 767.8955696845333705, -312.4527844766012663, 362.1676090361162323 ) ) ;
#20885 = CARTESIAN_POINT ( 'NONE',  ( 783.0433043558608688, -120.8965053807781800, 315.1538015810313027 ) ) ;
#20887 = EDGE_LOOP ( 'NONE', ( #2035, #18288, #16267, #4731 ) ) ;
#20888 = CARTESIAN_POINT ( 'NONE',  ( 801.3366627262608972, -248.5328690171414223, -353.0897708529566899 ) ) ;
#20889 = CARTESIAN_POINT ( 'NONE',  ( 755.0636971347428243, -100.2709662947838609, 341.7834795799807353 ) ) ;
#20890 = CARTESIAN_POINT ( 'NONE',  ( 773.7943932421234194, -287.8055962898685038, -305.5313806188329409 ) ) ;
#20891 = PLANE ( 'NONE',  #25343 ) ;
#20892 = CARTESIAN_POINT ( 'NONE',  ( 807.5423716828161105, -417.0783235625954148, 362.2119215644372048 ) ) ;
#20893 = ORIENTED_EDGE ( 'NONE', *, *, #31178, .F. ) ;
#20894 = CARTESIAN_POINT ( 'NONE',  ( 758.0580252608178853, -294.4527844766013800, 328.0187753319985404 ) ) ;
#20895 = CARTESIAN_POINT ( 'NONE',  ( 764.0069404352550464, -39.07832356259662276, -359.2566176426627180 ) ) ;
#20896 = CARTESIAN_POINT ( 'NONE',  ( 755.3201227861273992, -147.7255117493291152, -345.3687786644892981 ) ) ;
#20897 = CARTESIAN_POINT ( 'NONE',  ( 755.3201227861273992, -219.7255117493289447, -345.3687786644892981 ) ) ;
#20898 = CARTESIAN_POINT ( 'NONE',  ( 778.1981804954714335, -394.2709662947827951, 314.8072714833589885 ) ) ;
#20899 = CARTESIAN_POINT ( 'NONE',  ( 763.2262854647970016, -104.6346026584202207, -309.2812353651462445 ) ) ;
#20900 = CIRCLE ( 'NONE', #995, 30.00000000000008171 ) ;
#20901 = CARTESIAN_POINT ( 'NONE',  ( 800.2193346964446619, -114.9982390220565378, -355.1360043628816925 ) ) ;
#20902 = EDGE_LOOP ( 'NONE', ( #32338, #2052 ) ) ;
#20903 = AXIS2_PLACEMENT_3D ( 'NONE', #22386, #43647, #40641 ) ;
#20904 = CARTESIAN_POINT ( 'NONE',  ( 755.8894580844503253, -399.8272453906067767, -332.3691319403863531 ) ) ;
#20906 = CARTESIAN_POINT ( 'NONE',  ( 755.1538015810308480, -446.1908817542429802, 343.0433043558613804 ) ) ;
#20905 = CARTESIAN_POINT ( 'NONE',  ( 792.1044303154645831, -132.4527844766018916, 317.8323909638837677 ) ) ;
#20907 = CARTESIAN_POINT ( 'NONE',  ( 805.1016975059191054, -126.8965053807781516, 343.0745993439771837 ) ) ;
#20910 = CARTESIAN_POINT ( 'NONE',  ( 814.8230680027162407, -365.8055962898682765, 333.7305795820267917 ) ) ;
#20909 = DIRECTION ( 'NONE',  ( 0.000000000000000000, 0.000000000000000000, -1.000000000000000000 ) ) ;
#20908 = DIRECTION ( 'NONE',  ( -0.000000000000000000, -1.110223024625155554E-15, 1.000000000000000000 ) ) ;
#20911 = ORIENTED_EDGE ( 'NONE', *, *, #23265, .T. ) ;
#20912 = CARTESIAN_POINT ( 'NONE',  ( 760.7433823573367135, -348.0090635724251342, -355.9930595647440441 ) ) ;
#20913 = CARTESIAN_POINT ( 'NONE',  ( 801.9419747391806368, -354.4527844766012095, -351.9812246680014027 ) ) ;
#20914 = CARTESIAN_POINT ( 'NONE',  ( 745.7194118038753459, -157.6454272087893287, -348.7631598425976449 ) ) ;
#20915 = CARTESIAN_POINT ( 'NONE',  ( 771.3260364891663130, -19.64542720878974791, 306.0683387631859773 ) ) ;
#20916 = AXIS2_PLACEMENT_3D ( 'NONE', #6096, #16736, #30819 ) ;
#20918 = DIRECTION ( 'NONE',  ( -0.000000000000000000, -0.000000000000000000, 1.000000000000000000 ) ) ;
#20917 = DIRECTION ( 'NONE',  ( 0.000000000000000000, 0.000000000000000000, 1.000000000000000000 ) ) ;
#20919 = CARTESIAN_POINT ( 'NONE',  ( 773.3843516231979720, -301.4419599262320730, -364.4086373105754433 ) ) ;
#20920 = CARTESIAN_POINT ( 'NONE',  ( 801.9419747391806368, -450.4527844766009821, -351.9812246680014027 ) ) ;
#20921 = CARTESIAN_POINT ( 'NONE',  ( 771.3260364891663130, -139.6454272087893571, -306.0683387631859773 ) ) ;
#20922 = CARTESIAN_POINT ( 'NONE',  ( 799.9999999999993179, -512.9681489794448908, 370.0000000000000000 ) ) ;
#20923 = LINE ( 'NONE', #17717, #8328 ) ;
#20924 = CARTESIAN_POINT ( 'NONE',  ( 790.9844846989617508, -382.3726999360613945, 317.2208543904092721 ) ) ;
#20925 = CARTESIAN_POINT ( 'NONE',  ( 786.2694204179717872, -333.2817908451523863, 305.1769319972829067 ) ) ;
#20926 = CARTESIAN_POINT ( 'NONE',  ( 745.4481719005789273, -219.7255117493289447, -347.5162901302853697 ) ) ;
#20927 = CARTESIAN_POINT ( 'NONE',  ( 794.9999999999993179, -365.3551492539851893, -18.13243251470705886 ) ) ;
#20928 = CARTESIAN_POINT ( 'NONE',  ( 768.9521613784389729, -129.8272453906075725, 373.2346286133773106 ) ) ;
#20929 = CARTESIAN_POINT ( 'NONE',  ( 745.7998596910086917, -341.3618753856922012, -332.5602148656461168 ) ) ;
#20930 = ADVANCED_FACE ( 'NONE', ( #10268 ), #2659, .T. ) ;
#20931 = LINE ( 'NONE', #41290, #13425 ) ;
#20932 = FACE_OUTER_BOUND ( 'NONE', #16733, .T. ) ;
#20933 = CARTESIAN_POINT ( 'NONE',  ( 797.6776695296629214, -187.5436935675108430, 357.6776695296636603 ) ) ;
#20934 = CIRCLE ( 'NONE', #23124, 2.749999999999842792 ) ;
#20935 = ORIENTED_EDGE ( 'NONE', *, *, #30039, .F. ) ;
#20936 = VECTOR ( 'NONE', #39361, 1000.000000000000000 ) ;
#20937 = CARTESIAN_POINT ( 'NONE',  ( 764.1737431748507561, -418.3726999360612808, 371.6461892240376415 ) ) ;
#20938 = CARTESIAN_POINT ( 'NONE',  ( 801.9858362298568863, -387.0783235625955285, -312.7379699480935642 ) ) ;
#20939 = CARTESIAN_POINT ( 'NONE',  ( 813.1304606946830518, -113.9073299311474301, -352.3570229623690580 ) ) ;
#20940 = CARTESIAN_POINT ( 'NONE',  ( 747.2067596250078623, -435.1800572038737869, -352.2312462859687230 ) ) ;
#20941 = CARTESIAN_POINT ( 'NONE',  ( 939.9999999999993179, -431.4567479753240491, 350.0000000000000000 ) ) ;
#20942 = CARTESIAN_POINT ( 'NONE',  ( 771.2368401574024119, 10.55804007376686826, 374.2805881961240857 ) ) ;
#20943 = ORIENTED_EDGE ( 'NONE', *, *, #35323, .F. ) ;
#20944 = CARTESIAN_POINT ( 'NONE',  ( 766.5853460496234675, -157.9874144716871456, -372.3518521366060554 ) ) ;
#20945 = FACE_OUTER_BOUND ( 'NONE', #44796, .T. ) ;
#20946 = CARTESIAN_POINT ( 'NONE',  ( 754.0944755984390895, -303.6237781080503169, 364.1009440267246760 ) ) ;
#20947 = CARTESIAN_POINT ( 'NONE',  ( 803.6646147819162707, -113.9073299311474585, 348.8264449731211130 ) ) ;
#20948 = EDGE_LOOP ( 'NONE', ( #2055, #2742, #20070, #13024 ) ) ;
#20949 = AXIS2_PLACEMENT_3D ( 'NONE', #6436, #31360, #9885 ) ;
#20950 = CARTESIAN_POINT ( 'NONE',  ( 755.5713283507202505, -317.3618753856922581, 334.6858677611754729 ) ) ;
#20951 = CIRCLE ( 'NONE', #39452, 2.749999999999919176 ) ;
#20952 = CARTESIAN_POINT ( 'NONE',  ( 759.0252816721024374, -24.99823902205683268, -368.0189434323527280 ) ) ;
#20953 = EDGE_CURVE ( 'NONE', #38419, #9771, #26132, .T. ) ;
#20954 = CARTESIAN_POINT ( 'NONE',  ( 779.9999999999992042, -462.9681489794448339, -339.9999999999999432 ) ) ;
#20955 = CARTESIAN_POINT ( 'NONE',  ( 771.3260364891663130, -427.6454272087885897, -306.0683387631859773 ) ) ;
#20956 = EDGE_LOOP ( 'NONE', ( #1036, #33053, #23614, #3164, #34600, #4518 ) ) ;
#20957 = CARTESIAN_POINT ( 'NONE',  ( 758.0580252608178853, -270.4527844766014937, -328.0187753319985404 ) ) ;
#20959 = CARTESIAN_POINT ( 'NONE',  ( 814.8230680027162407, -245.8055962898686460, 333.7305795820267917 ) ) ;
#20958 = CARTESIAN_POINT ( 'NONE',  ( 745.7998596910086917, -365.3618753856920875, 332.5602148656461168 ) ) ;
#20960 = AXIS2_PLACEMENT_3D ( 'NONE', #7259, #6778, #31713 ) ;
#20961 = CARTESIAN_POINT ( 'NONE',  ( 813.9316612368132837, -79.44195992623286884, 348.6739635108323228 ) ) ;
#20962 = CARTESIAN_POINT ( 'NONE',  ( 784.1219089521767955, -261.2817908451526705, -315.0488828828318333 ) ) ;
#20963 = CARTESIAN_POINT ( 'NONE',  ( 774.6312213355099630, -239.3618753856924570, -364.6798772138717482 ) ) ;
#20964 = CIRCLE ( 'NONE', #1067, 2.749999999999919176 ) ;
#20965 = CARTESIAN_POINT ( 'NONE',  ( -190.7583438952259485, 290.0000000000001137, -274.9999999999999432 ) ) ;
#20966 = CARTESIAN_POINT ( 'NONE',  ( 774.6312213355099630, -119.3618753856928691, -364.6798772138717482 ) ) ;
#20967 = CIRCLE ( 'NONE', #27601, 30.00000000000008171 ) ;
#20968 = CARTESIAN_POINT ( 'NONE',  ( 771.2633955100217236, -239.9073299311470748, 363.4237431249939618 ) ) ;
#20969 = ORIENTED_EDGE ( 'NONE', *, *, #17079, .T. ) ;
#20970 = CARTESIAN_POINT ( 'NONE',  ( 804.7487373415286811, -379.5436935675102745, 364.7487373415288516 ) ) ;
#20971 = CARTESIAN_POINT ( 'NONE',  ( -879.9999999999992042, 240.0000000000002274, -219.9999999999999716 ) ) ;
#20972 = CARTESIAN_POINT ( 'NONE',  ( 783.7953271457878373, -32.19088175424425913, -375.1787889125761239 ) ) ;
#20973 = LINE ( 'NONE', #6670, #45529 ) ;
#20974 = CARTESIAN_POINT ( 'NONE',  ( 799.9999999999993179, 205.0000000000000568, 339.9999999999999432 ) ) ;
#20975 = ADVANCED_FACE ( 'NONE', ( #102 ), #42826, .F. ) ;
#20976 = CARTESIAN_POINT ( 'NONE',  ( 783.0745993439762742, -272.1908817542434917, 365.1016975059196739 ) ) ;
#20977 = CARTESIAN_POINT ( 'NONE',  ( 778.1981804954714335, -106.2709662947838467, 314.8072714833589885 ) ) ;
#20978 = ORIENTED_EDGE ( 'NONE', *, *, #28363, .F. ) ;
#20979 = CARTESIAN_POINT ( 'NONE',  ( 766.0291762391763086, -10.91815448151704793, -360.7704444035551319 ) ) ;
#20980 = AXIS2_PLACEMENT_3D ( 'NONE', #12028, #19182, #19628 ) ;
#20981 = CARTESIAN_POINT ( 'NONE',  ( 812.7932403749906598, -63.18005720387488822, -327.7687537140311633 ) ) ;
#20982 = CARTESIAN_POINT ( 'NONE',  ( 787.6308680596127942, -299.2601417444139997, 364.1105419155492768 ) ) ;
#20983 = CARTESIAN_POINT ( 'NONE',  ( 190.7583438952258916, 294.6698570112193920, -244.9999999999999716 ) ) ;
#20984 = AXIS2_PLACEMENT_3D ( 'NONE', #9426, #44769, #40835 ) ;
#20985 = CARTESIAN_POINT ( 'NONE',  ( 752.7379699480933368, -12.00906357242613609, 361.9858362298580232 ) ) ;
#20986 = EDGE_CURVE ( 'NONE', #8411, #9209, #45626, .T. ) ;
#20987 = CARTESIAN_POINT ( 'NONE',  ( 812.7932403749906598, -183.1800572038744974, -327.7687537140311633 ) ) ;
#20988 = EDGE_CURVE ( 'NONE', #36028, #3140, #11187, .T. ) ;
#20989 = CIRCLE ( 'NONE', #17304, 9.999999999999982236 ) ;
#20990 = CARTESIAN_POINT ( 'NONE',  ( 792.3570229623688874, -165.1800572038745258, 373.1304606946836202 ) ) ;
#20991 = CARTESIAN_POINT ( 'NONE',  ( 778.2165204200184689, -70.81642084023850714, 364.9363028652563230 ) ) ;
#20992 = CARTESIAN_POINT ( 'NONE',  ( 755.2512626584698410, 16.45630643248848912, 315.2512626584710915 ) ) ;
#20993 = CARTESIAN_POINT ( 'NONE',  ( 745.1769319972822814, -257.8055962898686744, -346.2694204179732083 ) ) ;
#20994 = CARTESIAN_POINT ( 'NONE',  ( 773.4516893846965786, 4.354572791210176597, 315.8398074228977066 ) ) ;
#20995 = CARTESIAN_POINT ( 'NONE',  ( 755.2512626584698410, -295.5436935675105588, -315.2512626584710915 ) ) ;
#20996 = FACE_OUTER_BOUND ( 'NONE', #20956, .T. ) ;
#20997 = CARTESIAN_POINT ( 'NONE',  ( 790.8726784830453198, -370.7146871989592114, 362.5472867521010585 ) ) ;
#20998 = CARTESIAN_POINT ( 'NONE',  ( 777.4774526936600978, -58.27096629478398881, 304.7301800767028226 ) ) ;
#20999 = CARTESIAN_POINT ( 'NONE',  ( 774.6312213355099630, -383.3618753856921444, -364.6798772138717482 ) ) ;
#21000 = CARTESIAN_POINT ( 'NONE',  ( 773.3843516231979720, -37.44195992623299674, 364.4086373105754433 ) ) ;
#21001 = CARTESIAN_POINT ( 'NONE',  ( 771.2633955100217236, -191.9073299311471885, -363.4237431249939618 ) ) ;
#21002 = MECHANICAL_DESIGN_GEOMETRIC_PRESENTATION_REPRESENTATION (  '', ( #15125 ), #13664 ) ;
#21003 = CARTESIAN_POINT ( 'NONE',  ( 747.3154664389472828, -43.98741447168752217, -326.4474001241230781 ) ) ;
#21004 = CARTESIAN_POINT ( 'NONE',  ( 805.1016975059191054, -174.8965053807779952, -343.0745993439771837 ) ) ;
#21005 = EDGE_CURVE ( 'NONE', #42174, #28618, #37204, .T. ) ;
#21006 = CARTESIAN_POINT ( 'NONE',  ( 811.6461892240364477, -196.7146871989598083, 324.1737431748509835 ) ) ;
#21007 = CARTESIAN_POINT ( 'NONE',  ( 788.8264449731201466, -21.18005720387502322, 363.6646147819170665 ) ) ;
#21008 = VECTOR ( 'NONE', #2774, 1000.000000000000000 ) ;
#21009 = EDGE_CURVE ( 'NONE', #14468, #44027, #25038, .T. ) ;
#21010 = VERTEX_POINT ( 'NONE', #14669 ) ;
#21011 = CARTESIAN_POINT ( 'NONE',  ( 804.4286716492782716, -89.36187538569299704, -345.3141322388244703 ) ) ;
#21012 = CARTESIAN_POINT ( 'NONE',  ( 805.1016975059191054, -198.8965053807779384, -343.0745993439771837 ) ) ;
#21013 = CARTESIAN_POINT ( 'NONE',  ( 754.8072714833581358, -196.8164208402380950, 338.1981804954720587 ) ) ;
#21014 = CARTESIAN_POINT ( 'NONE',  ( 801.9858362298568863, -27.07832356259665474, -312.7379699480935642 ) ) ;
#21015 = CARTESIAN_POINT ( 'NONE',  ( 755.5713283507202505, -317.3618753856922581, 334.6858677611754729 ) ) ;
#21016 = CARTESIAN_POINT ( 'NONE',  ( 767.9999999999992042, 178.9475563372491251, -320.0000000000000000 ) ) ;
#21017 = EDGE_LOOP ( 'NONE', ( #25355, #21197, #39100, #12606 ) ) ;
#21018 = CARTESIAN_POINT ( 'NONE',  ( 790.8726784830453198, -34.71468719896025590, 362.5472867521010585 ) ) ;
#21019 = CARTESIAN_POINT ( 'NONE',  ( 805.6418435158337843, -317.4636090269706301, -363.8556311672236916 ) ) ;
#21020 = VECTOR ( 'NONE', #25994, 1000.000000000000000 ) ;
#21021 = AXIS2_PLACEMENT_3D ( 'NONE', #5155, #43716, #43497 ) ;
#21022 = CARTESIAN_POINT ( 'NONE',  ( 804.7487373415286811, -259.5436935675106156, 364.7487373415288516 ) ) ;
#21023 = CARTESIAN_POINT ( 'NONE',  ( 759.0159684113467620, -328.9181544815160692, 325.8855110935213020 ) ) ;
#21024 = CIRCLE ( 'NONE', #32846, 2.749999999999891642 ) ;
#21025 = CARTESIAN_POINT ( 'NONE',  ( 803.8651313633788504, -437.2601417444135450, 332.4468031744301015 ) ) ;
#21026 = CARTESIAN_POINT ( 'NONE',  ( 783.0745993439762742, -152.1908817542438612, -365.1016975059196739 ) ) ;
#21027 = CARTESIAN_POINT ( 'NONE',  ( 802.1676090361156639, -158.6346026584199933, -327.8955696845344505 ) ) ;
#21028 = CARTESIAN_POINT ( 'NONE',  ( 791.9812246680005501, -356.6346026584193964, -361.9419747391813189 ) ) ;
#21029 = ORIENTED_EDGE ( 'NONE', *, *, #28357, .F. ) ;
#21030 = CARTESIAN_POINT ( 'NONE',  ( 815.2698199232961542, -304.8164208402376403, 342.5225473063383106 ) ) ;
#21031 = ADVANCED_FACE ( 'NONE', ( #18361 ), #14431, .F. ) ;
#21032 = CARTESIAN_POINT ( 'NONE',  ( 805.1016975059191054, -318.8965053807775121, 343.0745993439771837 ) ) ;
#21033 = CYLINDRICAL_SURFACE ( 'NONE', #37124, 1.000000000000000888 ) ;
#21034 = ADVANCED_FACE ( 'NONE', ( #32442 ), #25258, .F. ) ;
#21035 = CIRCLE ( 'NONE', #26181, 6.118999999999985562 ) ;
#21036 = CARTESIAN_POINT ( 'NONE',  ( 766.9102291470427417, -114.5545181178803631, 318.6633372737382501 ) ) ;
#21037 = CARTESIAN_POINT ( 'NONE',  ( 764.8639956371174549, -8.089148112965974136, 319.7806653035542013 ) ) ;
#21038 = EDGE_LOOP ( 'NONE', ( #43422, #28235, #41823, #11375 ) ) ;
#21039 = CARTESIAN_POINT ( 'NONE',  ( 809.0717654672305343, -364.9181544815158986, -360.1688906516309885 ) ) ;
#21040 = CIRCLE ( 'NONE', #31361, 2.749999999999919176 ) ;
#21041 = CARTESIAN_POINT ( 'NONE',  ( -26.63011601220122060, -513.1383975375929367, -369.9999999999999432 ) ) ;
#21042 = CARTESIAN_POINT ( 'NONE',  ( 788.6739635108323228, -247.6454272087890160, 373.9316612368139090 ) ) ;
#21043 = CARTESIAN_POINT ( 'NONE',  ( 803.8651313633788504, -197.2601417444143124, 332.4468031744301015 ) ) ;
#21044 = VECTOR ( 'NONE', #25292, 999.9999999999998863 ) ;
#21045 = CARTESIAN_POINT ( 'NONE',  ( 756.5762568750052424, -315.1800572038740711, -348.7366044899774238 ) ) ;
#21046 = DIRECTION ( 'NONE',  ( -1.000000000000000000, -0.000000000000000000, -0.000000000000000000 ) ) ;
#21047 = CARTESIAN_POINT ( 'NONE',  ( 804.8461984189677878, -218.1908817542437191, -336.9566956441385628 ) ) ;
#21048 = EDGE_CURVE ( 'NONE', #17397, #23953, #15850, .T. ) ;
#21049 = AXIS2_PLACEMENT_3D ( 'NONE', #28084, #20918, #10089 ) ;
#21050 = EDGE_CURVE ( 'NONE', #9329, #12718, #28263, .T. ) ;
#21051 = CARTESIAN_POINT ( 'NONE',  ( 792.2312462859673587, -11.90732993114778182, 307.2067596250082602 ) ) ;
#21052 = CARTESIAN_POINT ( 'NONE',  ( 792.2312462859673587, -83.90732993114754379, 307.2067596250082602 ) ) ;
#21053 = CARTESIAN_POINT ( 'NONE',  ( 801.0087853405226497, -452.9681489794447202, 354.4092604580203556 ) ) ;
#21054 = CARTESIAN_POINT ( 'NONE',  ( 751.6929314249750860, -414.9982390220555430, -318.8095938919659034 ) ) ;
#21055 = CARTESIAN_POINT ( 'NONE',  ( 769.9999999999992042, 205.0000000000000568, -339.9999999999999432 ) ) ;
#21056 = VECTOR ( 'NONE', #11251, 1000.000000000000000 ) ;
#21057 = CARTESIAN_POINT ( 'NONE',  ( 768.9521613784389729, -345.8272453906069472, 373.2346286133773106 ) ) ;
#21058 = CARTESIAN_POINT ( 'NONE',  ( 798.6699377194444196, -457.0491014588743042, -363.8754770338464368 ) ) ;
#21059 = CARTESIAN_POINT ( 'NONE',  ( 748.9653473494363425, -314.6346026584194533, 356.9462024416521331 ) ) ;
#21060 = CARTESIAN_POINT ( 'NONE',  ( 744.7301800767019131, -52.81642084023856398, -337.4774526936615757 ) ) ;
#21061 = CARTESIAN_POINT ( 'NONE',  ( 797.6776695296629214, -283.5436935675105019, -357.6776695296636603 ) ) ;
#21062 = CIRCLE ( 'NONE', #15184, 10.00000000000000888 ) ;
#21063 = DIRECTION ( 'NONE',  ( 0.000000000000000000, 0.000000000000000000, 1.000000000000000000 ) ) ;
#21064 = CARTESIAN_POINT ( 'NONE',  ( 755.0636971347428243, -388.2709662947829656, 341.7834795799807353 ) ) ;
#21065 = CARTESIAN_POINT ( 'NONE',  ( 793.9708237608222134, -166.9181544815165523, 319.2295555964448681 ) ) ;
#21066 = CARTESIAN_POINT ( 'NONE',  ( 755.8990559732751535, -35.46360902697151829, -365.9055244015606831 ) ) ;
#21067 = CARTESIAN_POINT ( 'NONE',  ( 756.7813123517142913, -91.98741447168737295, -329.9779781133712504 ) ) ;
#21068 = CARTESIAN_POINT ( 'NONE',  ( 761.9338519418445230, -62.53286901714199786, 370.4231160770881957 ) ) ;
#21069 = CARTESIAN_POINT ( 'NONE',  ( 804.9363028652555840, -400.2709662947828519, 338.2165204200192079 ) ) ;
#21070 = CARTESIAN_POINT ( 'NONE',  ( 815.2698199232962679, 7.183579159761249500, 342.5225473063383674 ) ) ;
#21071 = DIRECTION ( 'NONE',  ( -1.000000000000000000, -0.000000000000000000, -0.000000000000000000 ) ) ;
#21072 = CARTESIAN_POINT ( 'NONE',  ( 813.2346286133761168, -149.2601417444144261, 328.9521613784389160 ) ) ;
#21073 = CARTESIAN_POINT ( 'NONE',  ( 781.7834795799800531, -10.81642084023869543, -315.0636971347436202 ) ) ;
#21074 = ORIENTED_EDGE ( 'NONE', *, *, #25004, .T. ) ;
#21075 = CARTESIAN_POINT ( 'NONE',  ( 765.0180583372156207, -48.99823902205675807, -360.0135310231089534 ) ) ;
#21076 = CARTESIAN_POINT ( 'NONE',  ( 800.7704444035546203, -412.1692326535045936, -326.0291762391768771 ) ) ;
#21078 = CARTESIAN_POINT ( 'NONE',  ( 797.6776695296629214, -211.5436935675107861, 357.6776695296636603 ) ) ;
#21077 = CARTESIAN_POINT ( 'NONE',  ( 771.2633955100217236, -239.9073299311470748, 363.4237431249939618 ) ) ;
#21079 = ORIENTED_EDGE ( 'NONE', *, *, #16234, .T. ) ;
#21080 = CIRCLE ( 'NONE', #44691, 20.00000000000001776 ) ;
#21081 = CARTESIAN_POINT ( 'NONE',  ( 815.1787889125755555, -390.8965053807772279, -343.7953271457877804 ) ) ;
#21082 = CARTESIAN_POINT ( 'NONE',  ( 800.9747183278959710, 11.00176097794305541, 311.9810565676471583 ) ) ;
#21083 = DIRECTION ( 'NONE',  ( -1.000000000000000000, 0.000000000000000000, 0.000000000000000000 ) ) ;
#21084 = ORIENTED_EDGE ( 'NONE', *, *, #35683, .T. ) ;
#21085 = CARTESIAN_POINT ( 'NONE',  ( 759.9864689768902508, -434.0891481129646081, 354.9819416627836404 ) ) ;
#21086 = AXIS2_PLACEMENT_3D ( 'NONE', #3999, #24784, #32181 ) ;
#21087 = ORIENTED_EDGE ( 'NONE', *, *, #9203, .F. ) ;
#21088 =( NAMED_UNIT ( * ) SI_UNIT ( $, .STERADIAN. ) SOLID_ANGLE_UNIT ( ) );
#21089 = CIRCLE ( 'NONE', #33643, 2.749999999999863665 ) ;
#21090 = CARTESIAN_POINT ( 'NONE',  ( 767.7687537140311633, -239.9073299311470748, -372.7932403749916830 ) ) ;
#21091 = CARTESIAN_POINT ( 'NONE',  ( 745.4481719005789273, -147.7255117493291721, 347.5162901302853697 ) ) ;
#21092 = ORIENTED_EDGE ( 'NONE', *, *, #33961, .T. ) ;
#21093 = CARTESIAN_POINT ( 'NONE',  ( 795.1360043628808398, -236.0891481129652334, -360.2193346964456282 ) ) ;
#21094 = EDGE_LOOP ( 'NONE', ( #23456, #13256, #1876, #17524 ) ) ;
#21095 = CARTESIAN_POINT ( 'NONE',  ( 781.7834795799800531, -346.8164208402376971, -315.0636971347436202 ) ) ;
#21096 = CARTESIAN_POINT ( 'NONE',  ( 802.1676090361156639, -14.63460265842049424, -327.8955696845344505 ) ) ;
#21097 = VECTOR ( 'NONE', #22595, 1000.000000000000000 ) ;
#21098 = EDGE_CURVE ( 'NONE', #34451, #29646, #39148, .T. ) ;
#21099 = CARTESIAN_POINT ( 'NONE',  ( 759.2295555964440155, -232.1692326535051620, 353.9708237608231229 ) ) ;
#21100 = LINE ( 'NONE', #14869, #2653 ) ;
#21101 = PLANE ( 'NONE',  #20618 ) ;
#21102 = VECTOR ( 'NONE', #17228, 1000.000000000000000 ) ;
#21103 = PRODUCT ( 'Moving Blade Support Base', 'Moving Blade Support Base', '', ( #11267 ) ) ;
#21104 = VERTEX_POINT ( 'NONE', #13975 ) ;
#21105 = CARTESIAN_POINT ( 'NONE',  ( 756.3353852180819104, -5.907329931147798696, -331.1735550268788302 ) ) ;
#21106 = FACE_OUTER_BOUND ( 'NONE', #8926, .T. ) ;
#21107 = DIRECTION ( 'NONE',  ( -1.058954862565134068E-16, 0.6438296778008191223, -0.7651688349527137056 ) ) ;
#21108 = CARTESIAN_POINT ( 'NONE',  ( 804.1009440267234822, -263.4636090269708006, -314.0944755984392600 ) ) ;
#21109 = CARTESIAN_POINT ( 'NONE',  ( 811.3240766477731540, -148.3726999360620198, 355.6651683502462902 ) ) ;
#21111 = CARTESIAN_POINT ( 'NONE',  ( 803.6646147819161570, -233.9073299311470180, -348.8264449731210561 ) ) ;
#21110 = PLANE ( 'NONE',  #33485 ) ;
#21112 = CARTESIAN_POINT ( 'NONE',  ( 770.0799878456142551, -397.9874144716864066, -362.9823548866085616 ) ) ;
#21113 = DIRECTION ( 'NONE',  ( 0.000000000000000000, 0.000000000000000000, 1.000000000000000000 ) ) ;
#21114 = CARTESIAN_POINT ( 'NONE',  ( 796.1575198192839480, -126.0090635724257737, -359.4546378042384163 ) ) ;
#21115 = EDGE_CURVE ( 'NONE', #27436, #43717, #28377, .T. ) ;
#21116 = PLANE ( 'NONE',  #20350 ) ;
#21117 = CARTESIAN_POINT ( 'NONE',  ( 796.7845633553578182, -441.6237781080499190, -358.5707757039688204 ) ) ;
#21118 = CARTESIAN_POINT ( 'NONE',  ( 755.2512626584698410, -295.5436935675105588, -315.2512626584710915 ) ) ;
#21119 = FILL_AREA_STYLE ('',( #45381 ) ) ;
#21120 = DIRECTION ( 'NONE',  ( -8.326672684688676025E-16, 1.000000000000000000, 0.000000000000000000 ) ) ;
#21121 = CARTESIAN_POINT ( 'NONE',  ( 778.2165204200184689, -70.81642084023850714, -364.9363028652563230 ) ) ;
#21122 = CARTESIAN_POINT ( 'NONE',  ( 773.7305795820266212, -249.2817908451526421, 374.8230680027170365 ) ) ;
#21123 = CARTESIAN_POINT ( 'NONE',  ( 783.7566961878529810, -192.8965053807779668, -305.1792804349288417 ) ) ;
#21124 = CARTESIAN_POINT ( 'NONE',  ( 767.6429770376289525, -225.1800572038743269, 306.8695393053162093 ) ) ;
#21125 = CARTESIAN_POINT ( 'NONE',  ( 787.4397851343537695, -429.7255117493282910, -374.2001403089903988 ) ) ;
#21126 = CIRCLE ( 'NONE', #10809, 8.024999999999948841 ) ;
#21127 = CARTESIAN_POINT ( 'NONE',  ( 799.9999999999993179, 212.6707680665973612, 236.5295014342203785 ) ) ;
#21128 = CARTESIAN_POINT ( 'NONE',  ( 800.0135310231082713, -302.0891481129650629, 325.0180583372163028 ) ) ;
#21129 = CARTESIAN_POINT ( 'NONE',  ( 804.4086373105744769, -97.64542720878949922, 333.3843516231986541 ) ) ;
#21130 = CARTESIAN_POINT ( 'NONE',  ( 802.1676090361156639, -446.6346026584189985, -327.8955696845344505 ) ) ;
#21131 = DIRECTION ( 'NONE',  ( -1.058954862565134068E-16, 0.6438296778008191223, -0.7651688349527137056 ) ) ;
#21132 = CARTESIAN_POINT ( 'NONE',  ( 939.9999999999992042, 50.81038600091411439, -217.3872392842761769 ) ) ;
#21134 = CARTESIAN_POINT ( 'NONE',  ( 791.9812246680005501, -332.6346026584195101, 361.9419747391813189 ) ) ;
#21133 = CARTESIAN_POINT ( 'NONE',  ( 784.0799538623451781, -107.8055962898691433, 364.6971507214555572 ) ) ;
#21135 = ORIENTED_EDGE ( 'NONE', *, *, #45318, .T. ) ;
#21136 = AXIS2_PLACEMENT_3D ( 'NONE', #32357, #42963, #11331 ) ;
#21137 = CARTESIAN_POINT ( 'NONE',  ( 798.7617431975189675, -243.6237781080504590, -323.0428371773161871 ) ) ;
#21138 = CARTESIAN_POINT ( 'NONE',  ( 768.0187753319979720, -104.6346026584202207, 318.0580252608186242 ) ) ;
#21139 = CARTESIAN_POINT ( 'NONE',  ( 781.2497674668890113, -300.3510508353230080, -375.3608509340180603 ) ) ;
#21140 = DIRECTION ( 'NONE',  ( -0.000000000000000000, 1.000000000000000000, -0.000000000000000000 ) ) ;
#21141 = CARTESIAN_POINT ( 'NONE',  ( 776.2433038121456548, -420.8965053807772279, 374.8207195650711014 ) ) ;
#21142 = ORIENTED_EDGE ( 'NONE', *, *, #44180, .T. ) ;
#21143 = CARTESIAN_POINT ( 'NONE',  ( 804.9363028652555840, -304.2709662947832499, 338.2165204200192079 ) ) ;
#21144 = CARTESIAN_POINT ( 'NONE',  ( 755.8398074228967971, -43.44195992623296831, -333.4516893846970333 ) ) ;
#21145 = CARTESIAN_POINT ( 'NONE',  ( 788.8264449731200330, -165.1800572038745258, -363.6646147819171233 ) ) ;
#21146 = CARTESIAN_POINT ( 'NONE',  ( 774.6312213355099630, -191.3618753856925991, -364.6798772138717482 ) ) ;
#21147 = CARTESIAN_POINT ( 'NONE',  ( 774.6858677611749044, -393.7255117493283478, 315.5713283507209894 ) ) ;
#21148 = CARTESIAN_POINT ( 'NONE',  ( 814.2001403089898304, -137.3618753856928265, -347.4397851343538264 ) ) ;
#21149 = CARTESIAN_POINT ( 'NONE',  ( 754.8072714833583632, -100.8164208402383935, -338.1981804954721156 ) ) ;
#21150 = VERTEX_POINT ( 'NONE', #32205 ) ;
#21151 = CARTESIAN_POINT ( 'NONE',  ( 769.9779781133707957, -379.0999726633341993, -316.7813123517150871 ) ) ;
#21152 = CARTESIAN_POINT ( 'NONE',  ( 804.8461984189677878, -434.1908817542430370, 336.9566956441385628 ) ) ;
#21153 = CARTESIAN_POINT ( 'NONE',  ( 773.3843516231979720, -109.4419599262327836, 364.4086373105754433 ) ) ;
#21154 = CIRCLE ( 'NONE', #2691, 6.118999999999985562 ) ;
#21157 = CARTESIAN_POINT ( 'NONE',  ( 748.3538107759620743, -400.7146871989590977, 355.8262568251490165 ) ) ;
#21156 = DIRECTION ( 'NONE',  ( -0.000000000000000000, 0.000000000000000000, -1.000000000000000000 ) ) ;
#21155 = FACE_BOUND ( 'NONE', #43730, .T. ) ;
#21158 = ORIENTED_EDGE ( 'NONE', *, *, #30903, .T. ) ;
#21159 = CARTESIAN_POINT ( 'NONE',  ( 786.5483106153019435, -367.6454272087886466, -364.1601925771022366 ) ) ;
#21160 = CARTESIAN_POINT ( 'NONE',  ( 778.2165204200184689, -358.8164208402375834, -364.9363028652563230 ) ) ;
#21161 = CARTESIAN_POINT ( 'NONE',  ( 804.1009440267234822, -167.4636090269711133, -314.0944755984392600 ) ) ;
#21162 = AXIS2_PLACEMENT_3D ( 'NONE', #29248, #8682, #32705 ) ;
#21163 = CARTESIAN_POINT ( 'NONE',  ( 810.4231160770870019, -24.55451811788064020, 321.9338519418446936 ) ) ;
#21164 = AXIS2_PLACEMENT_3D ( 'NONE', #27741, #23579, #37684 ) ;
#21166 = CARTESIAN_POINT ( 'NONE',  ( -2.174186756557595869E-13, 469.9999999999994884, 0.000000000000000000 ) ) ;
#21165 = FACE_OUTER_BOUND ( 'NONE', #42784, .T. ) ;
#21167 = CARTESIAN_POINT ( 'NONE',  ( 804.1601925771018387, -295.4419599262320730, -346.5483106153029098 ) ) ;
#21168 = DIRECTION ( 'NONE',  ( -0.000000000000000000, 1.000000000000000000, -0.000000000000000000 ) ) ;
#21169 = CARTESIAN_POINT ( 'NONE',  ( 757.7880784355613741, -162.0090635724256742, -312.4576283171834916 ) ) ;
#21170 = LINE ( 'NONE', #17716, #28583 ) ;
#21171 = DIRECTION ( 'NONE',  ( 0.000000000000000000, 0.000000000000000000, 1.000000000000000000 ) ) ;
#21172 = AXIS2_PLACEMENT_3D ( 'NONE', #37570, #26944, #16562 ) ;
#21173 = CARTESIAN_POINT ( 'NONE',  ( 759.0159684113467620, -352.9181544815159555, 325.8855110935213020 ) ) ;
#21174 = CARTESIAN_POINT ( 'NONE',  ( 797.8822607201568644, -342.5545181178796952, 370.1134526219340160 ) ) ;
#21175 = CARTESIAN_POINT ( 'NONE',  ( 815.2698199232962679, -208.8164208402380666, -342.5225473063383674 ) ) ;
#21176 = FACE_OUTER_BOUND ( 'NONE', #228, .T. ) ;
#21177 = CARTESIAN_POINT ( 'NONE',  ( 779.9999999999992042, -462.9681489794448339, 339.9999999999999432 ) ) ;
#21178 = CARTESIAN_POINT ( 'NONE',  ( 813.5763878283155464, -147.8272453906075157, 351.1614460488615350 ) ) ;
#21179 = CARTESIAN_POINT ( 'NONE',  ( 808.7758568127978833, -100.1692326535055315, -320.0363995740631822 ) ) ;
#21180 = CARTESIAN_POINT ( 'NONE',  ( 772.4837098697144029, -71.36187538569302546, 374.5518280994205611 ) ) ;
#21181 = CARTESIAN_POINT ( 'NONE',  ( 782.5225473063381969, -334.2709662947829656, -375.2698199232970637 ) ) ;
#21182 = CARTESIAN_POINT ( 'NONE',  ( 919.9999999999993179, 154.9999999999998863, -360.0000000000000000 ) ) ;
#21183 = CARTESIAN_POINT ( 'NONE',  ( 769.9999999999992042, 205.0000000000000568, -339.9999999999999432 ) ) ;
#21184 = CARTESIAN_POINT ( 'NONE',  ( 756.3353852180819104, -197.9073299311472169, 331.1735550268788302 ) ) ;
#21185 = VERTEX_POINT ( 'NONE', #14890 ) ;
#21186 = CARTESIAN_POINT ( 'NONE',  ( 781.2370466360911223, -452.7363362996975411, 304.9990715423533629 ) ) ;
#21187 = CARTESIAN_POINT ( 'NONE',  ( 811.6461892240364477, -412.7146871989590409, -324.1737431748509835 ) ) ;
#21188 = CARTESIAN_POINT ( 'NONE',  ( 763.0537975583475827, -144.4527844766018632, -371.0346526505627480 ) ) ;
#21189 = CARTESIAN_POINT ( 'NONE',  ( 777.4774526936600978, -418.2709662947827383, -304.7301800767027657 ) ) ;
#21190 = DIRECTION ( 'NONE',  ( 0.000000000000000000, 0.000000000000000000, 1.000000000000000000 ) ) ;
#21191 = CARTESIAN_POINT ( 'NONE',  ( 814.8230680027162407, 18.19440371013048008, 333.7305795820267917 ) ) ;
#21192 = ORIENTED_EDGE ( 'NONE', *, *, #28021, .T. ) ;
#21193 = CIRCLE ( 'NONE', #33037, 2.749999999999863665 ) ;
#21194 = CARTESIAN_POINT ( 'NONE',  ( 800.1688906516307043, -178.1692326535052473, -369.0717654672308186 ) ) ;
#21195 = CARTESIAN_POINT ( 'NONE',  ( 751.2241431872005251, -304.1692326535048210, 359.9636004259367610 ) ) ;
#21196 = CARTESIAN_POINT ( 'NONE',  ( 797.8594530101009923, -109.5436935675110988, 322.1405469898982119 ) ) ;
#21197 = ORIENTED_EDGE ( 'NONE', *, *, #28109, .F. ) ;
#21198 = CARTESIAN_POINT ( 'NONE',  ( 771.2633955100217236, -287.9073299311468759, 363.4237431249939618 ) ) ;
#21199 = CARTESIAN_POINT ( 'NONE',  ( 787.5162901302840055, -35.36187538569316047, -305.4481719005792684 ) ) ;
#21200 = CARTESIAN_POINT ( 'NONE',  ( 782.5225473063383106, -70.27096629478397460, 375.2698199232970637 ) ) ;
#21201 = VERTEX_POINT ( 'NONE', #7722 ) ;
#21202 = CARTESIAN_POINT ( 'NONE',  ( 795.8262568251477660, -454.3726999360611103, -308.3538107759623585 ) ) ;
#21203 = VERTEX_POINT ( 'NONE', #567 ) ;
#21204 = ITEM_DEFINED_TRANSFORMATION ( 'NONE', 'NONE', #4665,  #26858 ) ;
#21205 = CARTESIAN_POINT ( 'NONE',  ( 755.5713283507202505, -29.36187538569318178, 334.6858677611754729 ) ) ;
#21206 = CARTESIAN_POINT ( 'NONE',  ( 758.0580252608178853, -246.4527844766016074, -328.0187753319985404 ) ) ;
#21208 = CARTESIAN_POINT ( 'NONE',  ( 791.1614460488616487, -299.2601417444139997, 373.5763878283158874 ) ) ;
#21207 = CARTESIAN_POINT ( 'NONE',  ( 777.5031285880264704, -358.8164208402375834, 374.9108240113588408 ) ) ;
#21209 = CARTESIAN_POINT ( 'NONE',  ( 745.1769319972822814, -65.80559628986925702, 346.2694204179732083 ) ) ;
#21210 = CARTESIAN_POINT ( 'NONE',  ( 759.0159684113467620, -256.9181544815163534, -325.8855110935213020 ) ) ;
#21211 = CARTESIAN_POINT ( 'NONE',  ( 762.1405469898971887, -241.5436935675106156, -357.8594530101015607 ) ) ;
#21212 = LINE ( 'NONE', #11054, #40828 ) ;
#21213 = CARTESIAN_POINT ( 'NONE',  ( 781.8018195045266339, -118.2709662947837899, -365.1927285166406705 ) ) ;
#21214 = CARTESIAN_POINT ( 'NONE',  ( 797.6776695296629214, -259.5436935675106156, 357.6776695296636603 ) ) ;
#21215 = ORIENTED_EDGE ( 'NONE', *, *, #1239, .T. ) ;
#21216 = CARTESIAN_POINT ( 'NONE',  ( 772.4837098697144029, -383.3618753856921444, 374.5518280994205611 ) ) ;
#21218 = CARTESIAN_POINT ( 'NONE',  ( 914.9999999999990905, 469.9999999999999432, 350.0000000000000000 ) ) ;
#21217 = CARTESIAN_POINT ( 'NONE',  ( 831.1634899080286232, 259.9999999999998863, -206.1189999999999429 ) ) ;
#21219 = CARTESIAN_POINT ( 'NONE',  ( 745.7194118038753459, -37.64542720878968396, -348.7631598425976449 ) ) ;
#21220 = LINE ( 'NONE', #17765, #7924 ) ;
#21221 = CYLINDRICAL_SURFACE ( 'NONE', #10493, 20.00000000000001776 ) ;
#21222 = CARTESIAN_POINT ( 'NONE',  ( 755.1538015810308480, -278.1908817542434917, 343.0433043558613804 ) ) ;
#21223 = CARTESIAN_POINT ( 'NONE',  ( 785.3687786644884454, -107.3618753856928976, 315.3201227861279676 ) ) ;
#21224 = ORIENTED_EDGE ( 'NONE', *, *, #2348, .T. ) ;
#21225 = CARTESIAN_POINT ( 'NONE',  ( 755.1538015810308480, -14.19088175424431242, -343.0433043558613804 ) ) ;
#21226 = CARTESIAN_POINT ( 'NONE',  ( 772.4837098697145166, -95.36187538569296862, -374.5518280994205611 ) ) ;
#21227 = CARTESIAN_POINT ( 'NONE',  ( 776.9566956441375396, -276.8965053807776258, 364.8461984189686405 ) ) ;
#21228 = AXIS2_PLACEMENT_3D ( 'NONE', #29156, #24997, #39108 ) ;
#21229 = CARTESIAN_POINT ( 'NONE',  ( 181.1634899080285948, 258.0939999999999941, -199.9999999999953957 ) ) ;
#21230 = CARTESIAN_POINT ( 'NONE',  ( 749.5768839229115201, -36.55451811788061178, 358.0661480581553064 ) ) ;
#21231 = CARTESIAN_POINT ( 'NONE',  ( 751.9810565676468741, -242.0891481129652618, -360.9747183278973921 ) ) ;
#21232 = CARTESIAN_POINT ( 'NONE',  ( 782.4968714119720516, -178.8164208402381519, 305.0891759886411023 ) ) ;
#21233 = CARTESIAN_POINT ( 'NONE',  ( 762.1405469898971887, -97.54369356751112718, 357.8594530101015607 ) ) ;
#21234 = CARTESIAN_POINT ( 'NONE',  ( 745.1769319972822814, -281.8055962898686175, -346.2694204179732083 ) ) ;
#21235 = CARTESIAN_POINT ( 'NONE',  ( 799.9636004259356241, -454.9181544815156713, 311.2241431872006956 ) ) ;
#21236 = CARTESIAN_POINT ( 'NONE',  ( 745.0891759886404770, -316.2709662947832499, -342.4968714119734159 ) ) ;
#21237 = DIRECTION ( 'NONE',  ( 0.000000000000000000, -1.000000000000000000, 0.000000000000000000 ) ) ;
#21238 = CARTESIAN_POINT ( 'NONE',  ( 803.2186876482843445, -367.9874144716865203, 350.0220218866286928 ) ) ;
#21239 = CARTESIAN_POINT ( 'NONE',  ( 808.3070685750232087, -42.99823902205676518, 361.1904061080339829 ) ) ;
#21240 = CARTESIAN_POINT ( 'NONE',  ( 768.0187753319979720, -392.6346026584193396, -318.0580252608186242 ) ) ;
#21241 = CARTESIAN_POINT ( 'NONE',  ( 783.0433043558608688, -48.89650538077840025, 315.1538015810313027 ) ) ;
#21242 = CARTESIAN_POINT ( 'NONE',  ( 785.3687786644884454, -203.3618753856925991, -315.3201227861279676 ) ) ;
#21243 = CARTESIAN_POINT ( 'NONE',  ( 793.4146539503750546, -73.98741447168741558, -307.6481478633938877 ) ) ;
#21244 = CARTESIAN_POINT ( 'NONE',  ( 814.8230680027162407, -197.8055962898688733, 333.7305795820267917 ) ) ;
#21245 = CARTESIAN_POINT ( 'NONE',  ( 756.3353852180820240, -29.90732993114772142, 331.1735550268787733 ) ) ;
#21246 = CARTESIAN_POINT ( 'NONE',  ( 770.0799878456142551, -373.9874144716864066, 362.9823548866085616 ) ) ;
#21247 = EDGE_LOOP ( 'NONE', ( #44263, #13713, #14949, #28418 ) ) ;
#21248 = CARTESIAN_POINT ( 'NONE',  ( 758.6633372737375112, -212.5328690171415076, -326.9102291470432533 ) ) ;
#21249 = CARTESIAN_POINT ( 'NONE',  ( 755.3201227861273992, -195.7255117493289731, 345.3687786644892981 ) ) ;
#21250 = ADVANCED_FACE ( 'NONE', ( #10730 ), #38930, .F. ) ;
#21251 = CARTESIAN_POINT ( 'NONE',  ( 808.7758568127978833, -28.16923265350574468, -320.0363995740631822 ) ) ;
#21252 = CARTESIAN_POINT ( 'NONE',  ( 762.3223304703356007, -319.5436935675104451, 322.3223304703362828 ) ) ;
#21253 = DIRECTION ( 'NONE',  ( 1.258530456726092671E-16, -0.7651688349527167032, -0.6438296778008156807 ) ) ;
#21254 = VERTEX_POINT ( 'NONE', #21802 ) ;
#21255 = CARTESIAN_POINT ( 'NONE',  ( 775.9200461376533440, -47.80559628986931386, 315.3028492785443291 ) ) ;
#21256 = CARTESIAN_POINT ( 'NONE',  ( 815.3608509340175488, -314.7363362996979959, -341.2497674668889545 ) ) ;
#21257 = VECTOR ( 'NONE', #21477, 1000.000000000000000 ) ;
#21258 = EDGE_CURVE ( 'NONE', #10285, #19003, #3800, .T. ) ;
#21259 = CARTESIAN_POINT ( 'NONE',  ( 800.9747183278959710, -252.9982390220560831, 311.9810565676471583 ) ) ;
#21260 = CARTESIAN_POINT ( 'NONE',  ( 786.2056067578752163, 12.19440371013049784, 374.4686193811670023 ) ) ;
#21261 = CARTESIAN_POINT ( 'NONE',  ( 757.4527132478984868, -160.3726999360620482, -329.1273215169538844 ) ) ;
#21262 = CARTESIAN_POINT ( 'NONE',  ( 803.4237431249931660, -135.1800572038746679, -331.2633955100225194 ) ) ;
#21263 = CARTESIAN_POINT ( 'NONE',  ( 778.2165204200184689, -334.8164208402376403, -364.9363028652563230 ) ) ;
#21264 = VERTEX_POINT ( 'NONE', #17890 ) ;
#21265 = CARTESIAN_POINT ( 'NONE',  ( 805.0032342141412300, -301.5436935675105588, 314.9967657858571783 ) ) ;
#21266 = FACE_OUTER_BOUND ( 'NONE', #34841, .T. ) ;
#21267 = CARTESIAN_POINT ( 'NONE',  ( 801.3366627262608972, -320.5328690171411949, 353.0897708529566899 ) ) ;
#21268 = CARTESIAN_POINT ( 'NONE',  ( -338.8365100919713200, 256.5000000000001137, -202.7499999999917009 ) ) ;
#21269 = CARTESIAN_POINT ( 'NONE',  ( 755.5913626894240451, -157.6454272087893287, 346.6156483768012890 ) ) ;
#21270 = CARTESIAN_POINT ( 'NONE',  ( 765.0180583372156207, -0.9982390220569063999, 360.0135310231089534 ) ) ;
#21271 = ORIENTED_EDGE ( 'NONE', *, *, #23244, .T. ) ;
#21272 = CARTESIAN_POINT ( 'NONE',  ( 773.7305795820266212, -393.2817908451522726, -374.8230680027170365 ) ) ;
#21273 = CARTESIAN_POINT ( 'NONE',  ( 814.2001403089898304, -17.36187538569322086, -347.4397851343538264 ) ) ;
#21274 = EDGE_CURVE ( 'NONE', #37602, #8774, #31958, .T. ) ;
#21275 = CARTESIAN_POINT ( 'NONE',  ( 764.1737431748507561, -226.3726999360617924, 371.6461892240376415 ) ) ;
#21276 = CARTESIAN_POINT ( 'NONE',  ( 795.9930595647434757, -171.0783235625962106, 320.7433823573372820 ) ) ;
#21277 = CARTESIAN_POINT ( 'NONE',  ( 757.8323909638827445, -362.6346026584194533, -352.1044303154654358 ) ) ;
#21278 = EDGE_CURVE ( 'NONE', #13363, #40120, #7757, .T. ) ;
#21279 = CARTESIAN_POINT ( 'NONE',  ( 802.9823548866075953, -457.0999726633339151, 330.0799878456151077 ) ) ;
#21280 = CARTESIAN_POINT ( 'NONE',  ( 190.7583438952258916, 294.6698570112193920, -274.9999999999999432 ) ) ;
#21281 = CARTESIAN_POINT ( 'NONE',  ( 773.4516893846965786, -235.6454272087890729, -315.8398074228977066 ) ) ;
#21282 = CARTESIAN_POINT ( 'NONE',  ( 745.7998596910086917, -5.361875385693257279, 332.5602148656461168 ) ) ;
#21283 = CARTESIAN_POINT ( 'NONE',  ( 808.3070685750230950, -66.99823902205672255, 361.1904061080339261 ) ) ;
#21284 = CARTESIAN_POINT ( 'NONE',  ( -879.9999999999992042, 430.0000000000002842, -224.9999999999999716 ) ) ;
#21285 = CARTESIAN_POINT ( 'NONE',  ( 748.9653473494365699, -410.6346026584191691, -356.9462024416520762 ) ) ;
#21286 = DIRECTION ( 'NONE',  ( -1.000000000000000000, 0.000000000000000000, 0.000000000000000000 ) ) ;
#21287 = AXIS2_PLACEMENT_3D ( 'NONE', #41622, #24283, #6738 ) ;
#21288 = CARTESIAN_POINT ( 'NONE',  ( 783.7953271457878373, -344.1908817542433212, 375.1787889125761239 ) ) ;
#21289 = LINE ( 'NONE', #41861, #23481 ) ;
#21290 = CARTESIAN_POINT ( 'NONE',  ( 767.6429770376289525, -321.1800572038740142, 306.8695393053162093 ) ) ;
#21291 = CARTESIAN_POINT ( 'NONE',  ( 751.6929314249748586, -54.99823902205672255, -318.8095938919659034 ) ) ;
#21292 = CARTESIAN_POINT ( 'NONE',  ( 755.3201227861273992, -267.7255117493286320, -345.3687786644892981 ) ) ;
#21293 = LINE ( 'NONE', #273, #45389 ) ;
#21294 = CARTESIAN_POINT ( 'NONE',  ( 802.1676090361156639, -422.6346026584192259, 327.8955696845344505 ) ) ;
#21295 = CARTESIAN_POINT ( 'NONE',  ( 793.0897708529556667, -198.5545181178800647, 361.3366627262616362 ) ) ;
#21296 = CARTESIAN_POINT ( 'NONE',  ( 809.0717654672305343, -28.91815448151699286, -360.1688906516309885 ) ) ;
#21297 = CARTESIAN_POINT ( 'NONE',  ( 772.3691319403857278, -71.26014174441469606, -315.8894580844506663 ) ) ;
#21298 = CARTESIAN_POINT ( 'NONE',  ( 746.0683387631852383, -115.4419599262327409, 331.3260364891676204 ) ) ;
#21299 = CARTESIAN_POINT ( 'NONE',  ( 768.0187753319979720, -416.6346026584192259, 318.0580252608186242 ) ) ;
#21300 = EDGE_CURVE ( 'NONE', #10014, #9510, #13649, .T. ) ;
#21301 = LINE ( 'NONE', #29092, #35871 ) ;
#21302 = CARTESIAN_POINT ( 'NONE',  ( 804.6798772138708955, 8.274488250670337663, -334.6312213355107019 ) ) ;
#21303 = ORIENTED_EDGE ( 'NONE', *, *, #31506, .F. ) ;
#21304 = CARTESIAN_POINT ( 'NONE',  ( 797.6776695296629214, -91.54369356751116982, -357.6776695296636603 ) ) ;
#21305 = EDGE_CURVE ( 'NONE', #17231, #13352, #39839, .T. ) ;
#21306 = CARTESIAN_POINT ( 'NONE',  ( 786.6156483768007774, -409.4419599262317320, -315.5913626894246136 ) ) ;
#21308 = CARTESIAN_POINT ( 'NONE',  ( 758.0580252608178853, -222.4527844766016642, 328.0187753319985404 ) ) ;
#21307 = CARTESIAN_POINT ( 'NONE',  ( 802.1676090361156639, -230.6346026584197659, 327.8955696845344505 ) ) ;
#21309 = ORIENTED_EDGE ( 'NONE', *, *, #11465, .T. ) ;
#21310 = CARTESIAN_POINT ( 'NONE',  ( 815.0009284576459549, -390.3510508353227237, -338.7629533639073429 ) ) ;
#21311 = CARTESIAN_POINT ( 'NONE',  ( 939.9999999999993179, -600.0000000000001137, 360.0000000000000000 ) ) ;
#21312 = ORIENTED_EDGE ( 'NONE', *, *, #12270, .F. ) ;
#21313 = CARTESIAN_POINT ( 'NONE',  ( 767.8955696845333705, -432.4527844766008684, 362.1676090361162323 ) ) ;
#21314 = ORIENTED_EDGE ( 'NONE', *, *, #35945, .F. ) ;
#21315 = EDGE_CURVE ( 'NONE', #7478, #33715, #1240, .T. ) ;
#21316 = ADVANCED_FACE ( 'NONE', ( #19239 ), #19459, .T. ) ;
#21317 = CARTESIAN_POINT ( 'NONE',  ( 810.7187646348534145, -258.4527844766016074, -356.7737145352016341 ) ) ;
#21318 = CARTESIAN_POINT ( 'NONE',  ( 813.1304606946831655, -161.9073299311472738, 352.3570229623691716 ) ) ;
#21319 = ORIENTED_EDGE ( 'NONE', *, *, #11931, .F. ) ;
#21320 = CARTESIAN_POINT ( 'NONE',  ( 788.8264449731201466, -237.1800572038742985, -363.6646147819170665 ) ) ;
#21321 = VERTEX_POINT ( 'NONE', #43279 ) ;
#21322 = VECTOR ( 'NONE', #19871, 1000.000000000000000 ) ;
#21323 = CARTESIAN_POINT ( 'NONE',  ( 785.3687786644884454, -371.3618753856919739, -315.3201227861279676 ) ) ;
#21324 = CARTESIAN_POINT ( 'NONE',  ( 788.7366044899766848, -11.90732993114778182, -316.5762568750059813 ) ) ;
#21325 = CARTESIAN_POINT ( 'NONE',  ( 779.4709603349208464, -240.3510508353232069, 314.7162404726379918 ) ) ;
#21326 = DIRECTION ( 'NONE',  ( 1.000000000000000000, 0.000000000000000000, -0.000000000000000000 ) ) ;
#21327 = DIRECTION ( 'NONE',  ( 0.000000000000000000, 0.000000000000000000, 1.000000000000000000 ) ) ;
#21328 = ORIENTED_EDGE ( 'NONE', *, *, #1789, .F. ) ;
#21329 = CARTESIAN_POINT ( 'NONE',  ( 781.7834795799800531, -10.81642084023869543, -315.0636971347436202 ) ) ;
#21330 = DIRECTION ( 'NONE',  ( 0.000000000000000000, 1.000000000000000000, -0.000000000000000000 ) ) ;
#21331 = DIRECTION ( 'NONE',  ( 8.326672684688676025E-16, 1.000000000000000000, 0.000000000000000000 ) ) ;
#21332 = ORIENTED_EDGE ( 'NONE', *, *, #11685, .T. ) ;
#21333 = CARTESIAN_POINT ( 'NONE',  ( 781.2370466360911223, -260.7363362996981095, -304.9990715423533629 ) ) ;
#21334 = CARTESIAN_POINT ( 'NONE',  ( 788.6739635108323228, -127.6454272087894140, 373.9316612368139090 ) ) ;
#21336 = CARTESIAN_POINT ( 'NONE',  ( 804.6798772138708955, -255.7255117493287742, -334.6312213355107019 ) ) ;
#21335 = CARTESIAN_POINT ( 'NONE',  ( -786.4999999999993179, -292.9981031064102126, 121.3637880562633171 ) ) ;
#21337 = CARTESIAN_POINT ( 'NONE',  ( 793.2243759319678702, -410.5328690171408539, -318.4439275373583200 ) ) ;
#21338 = EDGE_CURVE ( 'NONE', #13729, #39585, #40198, .T. ) ;
#21339 = DIRECTION ( 'NONE',  ( 0.000000000000000000, -0.000000000000000000, -1.000000000000000000 ) ) ;
#21340 = CARTESIAN_POINT ( 'NONE',  ( 758.4439275373578084, -132.5545181178802920, -353.2243759319684386 ) ) ;
#21341 = CARTESIAN_POINT ( 'NONE',  ( 797.8822607201568644, -390.5545181178794678, 370.1134526219340160 ) ) ;
#21342 = DIRECTION ( 'NONE',  ( -1.000000000000000000, -0.000000000000000000, -0.000000000000000000 ) ) ;
#21343 = CARTESIAN_POINT ( 'NONE',  ( 766.5853460496234675, 10.01258552831232329, -372.3518521366060554 ) ) ;
#21344 = CARTESIAN_POINT ( 'NONE',  ( 748.9653473494365699, -314.6346026584195101, -356.9462024416520762 ) ) ;
#21345 = PRESENTATION_STYLE_ASSIGNMENT (( #31951 ) ) ;
#21346 = CARTESIAN_POINT ( 'NONE',  ( 797.6776695296629214, -19.54369356751139364, 357.6776695296636603 ) ) ;
#21347 = CARTESIAN_POINT ( 'NONE',  ( 795.8262568251477660, -238.3726999360617640, 308.3538107759623585 ) ) ;
#21348 = CARTESIAN_POINT ( 'NONE',  ( 813.9316612368132837, -199.4419599262324709, -348.6739635108323228 ) ) ;
#21349 = CARTESIAN_POINT ( 'NONE',  ( 763.2262854647970016, -224.6346026584198228, 309.2812353651462445 ) ) ;
#21350 = CARTESIAN_POINT ( 'NONE',  ( 758.8095938919642549, -440.0891481129644944, -311.6929314249763365 ) ) ;
#21351 = DIRECTION ( 'NONE',  ( 0.000000000000000000, 0.9235249282889854694, 0.3835384033298675499 ) ) ;
#21352 = CARTESIAN_POINT ( 'NONE',  ( 764.8639956371174549, -320.0891481129648355, 319.7806653035542013 ) ) ;
#21353 = CARTESIAN_POINT ( 'NONE',  ( 783.0745993439762742, -80.19088175424411702, 365.1016975059196739 ) ) ;
#21354 = CARTESIAN_POINT ( 'NONE',  ( 755.3028492785439312, -63.28179084515324604, 335.9200461376539693 ) ) ;
#21355 = CARTESIAN_POINT ( 'NONE',  ( 770.0799878456142551, 10.01258552831232329, -362.9823548866085616 ) ) ;
#21356 = AXIS2_PLACEMENT_3D ( 'NONE', #2861, #45599, #30570 ) ;
#21357 = DIRECTION ( 'NONE',  ( -0.000000000000000000, 1.000000000000000000, -0.000000000000000000 ) ) ;
#21358 = EDGE_CURVE ( 'NONE', #31246, #19577, #33326, .T. ) ;
#21359 = CARTESIAN_POINT ( 'NONE',  ( 779.9999999999992042, 126.4563064324884465, 339.9999999999999432 ) ) ;
#21361 = CARTESIAN_POINT ( 'NONE',  ( 765.0180583372156207, -360.9982390220557704, 360.0135310231089534 ) ) ;
#21360 = CARTESIAN_POINT ( 'NONE',  ( 758.6633372737375112, -116.5328690171418202, 326.9102291470432533 ) ) ;
#21362 = ORIENTED_EDGE ( 'NONE', *, *, #426, .T. ) ;
#21363 = CARTESIAN_POINT ( 'NONE',  ( 797.8594530101008786, -37.54369356751132614, -322.1405469898980982 ) ) ;
#21364 = ADVANCED_FACE ( 'NONE', ( #25937, #29863 ), #22469, .F. ) ;
#21365 = CARTESIAN_POINT ( 'NONE',  ( 755.8398074228967971, -283.4419599262321867, -333.4516893846970333 ) ) ;
#21366 = CARTESIAN_POINT ( 'NONE',  ( 768.0187753319979720, -80.63460265842029173, 318.0580252608186242 ) ) ;
#21367 = CARTESIAN_POINT ( 'NONE',  ( 815.1787889125755555, -294.8965053807775689, -343.7953271457877804 ) ) ;
#21368 = DIRECTION ( 'NONE',  ( 0.000000000000000000, 0.000000000000000000, -1.000000000000000000 ) ) ;
#21369 = CARTESIAN_POINT ( 'NONE',  ( 771.2368401574024119, -421.4419599262317888, 374.2805881961240857 ) ) ;
#21370 = ORIENTED_EDGE ( 'NONE', *, *, #10900, .F. ) ;
#21371 = CARTESIAN_POINT ( 'NONE',  ( 757.8323909638827445, -314.6346026584194533, 352.1044303154654358 ) ) ;
#21372 = CARTESIAN_POINT ( 'NONE',  ( 790.8726784830453198, -58.71468719896019905, -362.5472867521010585 ) ) ;
#21373 = CARTESIAN_POINT ( 'NONE',  ( 788.7366044899766848, -155.9073299311473306, -316.5762568750059813 ) ) ;
#21374 = CARTESIAN_POINT ( 'NONE',  ( 762.3223304703356007, -223.5436935675107577, -322.3223304703362828 ) ) ;
#21375 = CARTESIAN_POINT ( 'NONE',  ( 781.7834795799800531, -418.8164208402374129, 315.0636971347436202 ) ) ;
#21376 = CARTESIAN_POINT ( 'NONE',  ( 763.0537975583475827, -144.4527844766018632, -371.0346526505627480 ) ) ;
#21377 = APPLICATION_CONTEXT ( 'automotive_design' ) ;
#21378 = PRODUCT_DEFINITION ( 'UNKNOWN', '', #17930, #23776 ) ;
#21379 = ORIENTED_EDGE ( 'NONE', *, *, #29470, .T. ) ;
#21380 = CARTESIAN_POINT ( 'NONE',  ( 781.8018195045267476, -142.2709662947837330, -365.1927285166407273 ) ) ;
#21381 = ORIENTED_EDGE ( 'NONE', *, *, #31752, .T. ) ;
#21382 = CARTESIAN_POINT ( 'NONE',  ( 755.5913626894240451, -397.6454272087885329, -346.6156483768012890 ) ) ;
#21384 = CARTESIAN_POINT ( 'NONE',  ( 801.5560724626406000, -432.5545181178793541, 326.7756240680316182 ) ) ;
#21383 = CARTESIAN_POINT ( 'NONE',  ( 765.0180583372156207, -120.9982390220565378, 360.0135310231089534 ) ) ;
#21385 = CARTESIAN_POINT ( 'NONE',  ( 796.7845633553578182, -129.6237781080508853, 358.5707757039688204 ) ) ;
#21388 = CARTESIAN_POINT ( 'NONE',  ( 745.1769319972822814, -401.8055962898681059, 346.2694204179732083 ) ) ;
#21387 = CYLINDRICAL_SURFACE ( 'NONE', #45429, 6.118999999999985562 ) ;
#21386 = CARTESIAN_POINT ( 'NONE',  ( 180.7583438952258348, 394.6698570112193920, -244.9999999999999716 ) ) ;
#21389 = EDGE_LOOP ( 'NONE', ( #3988, #41546, #26319, #22892, #9664, #36305 ) ) ;
#21390 = CARTESIAN_POINT ( 'NONE',  ( 801.5560724626406000, -408.5545181178794110, -326.7756240680316182 ) ) ;
#21391 = DIRECTION ( 'NONE',  ( 5.551115123125783688E-16, 1.000000000000000000, -0.000000000000000000 ) ) ;
#21392 = CARTESIAN_POINT ( 'NONE',  ( 773.7305795820266212, -177.2817908451528695, -374.8230680027170365 ) ) ;
#21393 = CARTESIAN_POINT ( 'NONE',  ( 757.7880784355613741, -18.00906357242611477, 312.4576283171834916 ) ) ;
#21395 = CARTESIAN_POINT ( 'NONE',  ( 914.9999999999992042, 99.99999999999984368, 360.0000000000000000 ) ) ;
#21394 = CARTESIAN_POINT ( 'NONE',  ( 779.9999999999992042, 16.45630643248849267, 329.9999999999999432 ) ) ;
#21396 = DIRECTION ( 'NONE',  ( 5.551115123125783688E-16, -1.000000000000000000, 0.000000000000000000 ) ) ;
#21397 = CARTESIAN_POINT ( 'NONE',  ( 749.5768839229115201, -204.5545181178800931, -358.0661480581553064 ) ) ;
#21398 = CARTESIAN_POINT ( 'NONE',  ( 939.9999999999993179, 56.78581973499407809, 212.6378164459127618 ) ) ;
#21399 = CARTESIAN_POINT ( 'NONE',  ( -39.63011601220123481, -365.3551492539851893, -18.13243251470705886 ) ) ;
#21400 = CARTESIAN_POINT ( 'NONE',  ( 757.4527132478984868, -352.3726999360614514, 329.1273215169538844 ) ) ;
#21401 = CARTESIAN_POINT ( 'NONE',  ( 811.3240766477731540, -340.3726999360615082, 355.6651683502462902 ) ) ;
#21402 = CARTESIAN_POINT ( 'NONE',  ( 755.2512626584698410, -199.5436935675108430, -315.2512626584710915 ) ) ;
#21403 = CARTESIAN_POINT ( 'NONE',  ( 701.1634899080286232, 256.4999999999999432, -206.1189999999990334 ) ) ;
#21404 = DIRECTION ( 'NONE',  ( 0.000000000000000000, -0.3826834323650837866, -0.9238795325112891810 ) ) ;
#21405 = CARTESIAN_POINT ( 'NONE',  ( 747.6481478633932056, -133.0999726633348246, 353.4146539503763620 ) ) ;
#21406 = CARTESIAN_POINT ( 'NONE',  ( 752.4576283171824116, -93.07832356259645223, -317.7880784355627952 ) ) ;
#21407 = CARTESIAN_POINT ( 'NONE',  ( 754.9967657858570647, -121.5436935675110419, 365.0032342141425374 ) ) ;
#21408 = CARTESIAN_POINT ( 'NONE',  ( 808.0189434323515343, -326.0891481129649492, -319.0252816721025511 ) ) ;
#21409 = CARTESIAN_POINT ( 'NONE',  ( 799.9999999999993179, -462.9681489794448339, -309.9999999999998863 ) ) ;
#21410 = DIRECTION ( 'NONE',  ( -0.000000000000000000, 1.000000000000000000, -0.000000000000000000 ) ) ;
#21411 = CARTESIAN_POINT ( 'NONE',  ( 762.1405469898971887, -169.5436935675108430, 357.8594530101015607 ) ) ;
#21412 = CARTESIAN_POINT ( 'NONE',  ( 748.6759233522253680, -448.3726999360611103, 324.3348316497537098 ) ) ;
#21413 = CARTESIAN_POINT ( 'NONE',  ( 747.3154664389472828, -427.9874144716862929, -326.4474001241230781 ) ) ;
#21414 = CARTESIAN_POINT ( 'NONE',  ( 812.7932403749906598, -423.1800572038737300, -327.7687537140311633 ) ) ;
#21415 = CYLINDRICAL_SURFACE ( 'NONE', #33582, 6.119000000000013095 ) ;
#21416 = CARTESIAN_POINT ( 'NONE',  ( 758.0141637701419768, 8.921676437403235127, 367.2620300519063790 ) ) ;
#21417 = EDGE_LOOP ( 'NONE', ( #19892, #6815, #44311, #29828 ) ) ;
#21418 = ADVANCED_FACE ( 'NONE', ( #12092 ), #25498, .F. ) ;
#21419 = CARTESIAN_POINT ( 'NONE',  ( 812.6845335610512393, -199.9874144716870603, -353.5525998758768651 ) ) ;
#21420 = DIRECTION ( 'NONE',  ( 1.000000000000000000, 0.000000000000000000, 0.000000000000000000 ) ) ;
#21421 = CARTESIAN_POINT ( 'NONE',  ( 783.7566961878529810, -312.8965053807775689, 305.1792804349288417 ) ) ;
#21422 = CARTESIAN_POINT ( 'NONE',  ( 762.1405469898973024, -121.5436935675110561, 357.8594530101016176 ) ) ;
#21423 = ORIENTED_EDGE ( 'NONE', *, *, #24044, .T. ) ;
#21424 = CARTESIAN_POINT ( 'NONE',  ( 781.7834795799800531, -298.8164208402377540, 315.0636971347436202 ) ) ;
#21425 = CARTESIAN_POINT ( 'NONE',  ( 804.7487373415286811, -43.54369356751131903, -364.7487373415288516 ) ) ;
#21426 = CARTESIAN_POINT ( 'NONE',  ( 787.4397851343537695, -69.72551174932942786, 374.2001403089903988 ) ) ;
#21427 = ORIENTED_EDGE ( 'NONE', *, *, #10616, .T. ) ;
#21428 = CARTESIAN_POINT ( 'NONE',  ( 814.8207195650702488, -434.1908817542430370, -336.2433038121456548 ) ) ;
#21429 = EDGE_LOOP ( 'NONE', ( #27612, #15670, #3022, #14219 ) ) ;
#21430 = PRODUCT_CONTEXT ( 'NONE', #19885, 'mechanical' ) ;
#21431 = CARTESIAN_POINT ( 'NONE',  ( 774.6858677611749044, -33.72551174932952733, 315.5713283507209894 ) ) ;
#21432 = CARTESIAN_POINT ( 'NONE',  ( 805.1927285166397041, -280.8164208402378677, -341.8018195045277707 ) ) ;
#21434 = CARTESIAN_POINT ( 'NONE',  ( 813.9316612368132837, -295.4419599262320730, 348.6739635108323228 ) ) ;
#21433 = CARTESIAN_POINT ( 'NONE',  ( 808.3070685750232087, -402.9982390220555999, 361.1904061080339829 ) ) ;
#21435 = CARTESIAN_POINT ( 'NONE',  ( 758.0141637701419768, -87.07832356259646645, 367.2620300519063790 ) ) ;
#21436 = CARTESIAN_POINT ( 'NONE',  ( 805.2837595273609850, -290.7363362996980527, -340.5290396650784714 ) ) ;
#21437 = CARTESIAN_POINT ( 'NONE',  ( 785.3687786644884454, -251.3618753856923149, -315.3201227861279676 ) ) ;
#21438 = DIRECTION ( 'NONE',  ( 1.000000000000000000, 0.000000000000000000, 0.000000000000000000 ) ) ;
#21439 = CARTESIAN_POINT ( 'NONE',  ( 794.9819416627830151, -108.9982390220565804, -319.9864689768909898 ) ) ;
#21440 = DIRECTION ( 'NONE',  ( -0.000000000000000000, 1.000000000000000000, -0.000000000000000000 ) ) ;
#21441 = CARTESIAN_POINT ( 'NONE',  ( 810.7187646348534145, -402.4527844766010389, 356.7737145352016341 ) ) ;
#21443 = LINE ( 'NONE', #3895, #35163 ) ;
#21442 = CARTESIAN_POINT ( 'NONE',  ( 999.9999999999992042, 478.9999999999999432, 200.9999999999999432 ) ) ;
#21444 = CARTESIAN_POINT ( 'NONE',  ( 750.9282345327678740, -64.91815448151686496, -319.8311093483690115 ) ) ;
#21445 = CARTESIAN_POINT ( 'NONE',  ( -728.8365100919714905, 260.0000000000001705, -193.8809999999890863 ) ) ;
#21446 = CARTESIAN_POINT ( 'NONE',  ( 939.9999999999993179, -179.7356316342496712, 69.11609595480024382 ) ) ;
#21447 = CARTESIAN_POINT ( 'NONE',  ( 775.8780910478218402, -273.2817908451526137, 364.9511171171680530 ) ) ;
#21448 = CARTESIAN_POINT ( 'NONE',  ( 804.9363028652555840, -160.2709662947836762, 338.2165204200192079 ) ) ;
#21449 = ORIENTED_EDGE ( 'NONE', *, *, #17059, .F. ) ;
#21450 = CARTESIAN_POINT ( 'NONE',  ( 773.4516893846965786, -43.64542720878966975, -315.8398074228977066 ) ) ;
#21451 = CARTESIAN_POINT ( 'NONE',  ( 787.4397851343537695, -117.7255117493292715, -374.2001403089903988 ) ) ;
#21452 = CARTESIAN_POINT ( 'NONE',  ( 793.2243759319678702, -290.5328690171412518, 318.4439275373583200 ) ) ;
#21453 = DIRECTION ( 'NONE',  ( -0.000000000000000000, 1.000000000000000000, -0.000000000000000000 ) ) ;
#21454 = CARTESIAN_POINT ( 'NONE',  ( 752.7379699480933368, -36.00906357242605793, 361.9858362298580232 ) ) ;
#21455 = CARTESIAN_POINT ( 'NONE',  ( 747.2067596250078623, -243.1800572038743269, -352.2312462859687230 ) ) ;
#21456 = CARTESIAN_POINT ( 'NONE',  ( 747.2067596250078623, -195.1800572038744974, 352.2312462859687230 ) ) ;
#21457 = CARTESIAN_POINT ( 'NONE',  ( 764.8639956371174549, -80.08914811296574499, 319.7806653035542013 ) ) ;
#21458 = LINE ( 'NONE', #42708, #29167 ) ;
#21459 = CARTESIAN_POINT ( 'NONE',  ( 768.8385539511368734, -311.2601417444139429, -306.4236121716840557 ) ) ;
#21460 = CARTESIAN_POINT ( 'NONE',  ( 750.9282345327678740, -448.9181544815156144, 319.8311093483690115 ) ) ;
#21461 = CARTESIAN_POINT ( 'NONE',  ( 810.7187646348534145, -330.4527844766013231, -356.7737145352016341 ) ) ;
#21462 = DIRECTION ( 'NONE',  ( 1.000000000000000000, 0.000000000000000000, 0.000000000000000000 ) ) ;
#21463 = CARTESIAN_POINT ( 'NONE',  ( 794.1144889064781864, -346.1692326535047641, 360.9840315886528401 ) ) ;
#21464 = CARTESIAN_POINT ( 'NONE',  ( 796.7737145352015204, -44.63460265842040542, 370.7187646348536987 ) ) ;
#21465 = CARTESIAN_POINT ( 'NONE',  ( 804.4286716492782716, -401.3618753856920307, -345.3141322388244703 ) ) ;
#21466 = CARTESIAN_POINT ( 'NONE',  ( 756.1348686366196716, -65.26014174441471027, 347.5531968255698416 ) ) ;
#21467 = CARTESIAN_POINT ( 'NONE',  ( 759.8311093483677041, -70.16923265350563099, -310.9282345327691814 ) ) ;
#21468 = CARTESIAN_POINT ( 'NONE',  ( 764.3348316497523456, -214.7146871989597230, 308.6759233522265617 ) ) ;
#21469 = CARTESIAN_POINT ( 'NONE',  ( 785.3141322388236176, -21.72551174932956641, 364.4286716492789537 ) ) ;
#21470 = ORIENTED_EDGE ( 'NONE', *, *, #12270, .T. ) ;
#21471 = CARTESIAN_POINT ( 'NONE',  ( 798.7617431975189675, -195.6237781080506863, -323.0428371773161871 ) ) ;
#21472 = CARTESIAN_POINT ( 'NONE',  ( 785.3687786644884454, -203.3618753856925991, 315.3201227861279676 ) ) ;
#21473 = PRODUCT ( 'Upper Moving Shear Blade Bar', 'Upper Moving Shear Blade Bar', '', ( #3881 ) ) ;
#21474 = CARTESIAN_POINT ( 'NONE',  ( 812.6845335610512393, -31.98741447168754348, -353.5525998758768651 ) ) ;
#21475 = CARTESIAN_POINT ( 'NONE',  ( 805.1927285166399315, -328.8164208402375834, 341.8018195045277707 ) ) ;
#21476 = CARTESIAN_POINT ( 'NONE',  ( 808.4681505782122031, -452.9681489794450613, -336.7690310503822388 ) ) ;
#21477 = DIRECTION ( 'NONE',  ( -1.000000000000000000, -0.000000000000000000, -0.000000000000000000 ) ) ;
#21478 = EDGE_LOOP ( 'NONE', ( #18391, #34755, #43828 ) ) ;
#21479 = CARTESIAN_POINT ( 'NONE',  ( 801.3366627262608972, -56.53286901714201917, 353.0897708529566899 ) ) ;
#21480 = CARTESIAN_POINT ( 'NONE',  ( 797.8822607201568644, -342.5545181178796952, -370.1134526219340160 ) ) ;
#21481 = CARTESIAN_POINT ( 'NONE',  ( 759.0252816721024374, -288.9982390220559978, 368.0189434323527280 ) ) ;
#21482 = CARTESIAN_POINT ( 'NONE',  ( 764.3348316497523456, 1.285312801039623753, 308.6759233522265617 ) ) ;
#21483 = EDGE_CURVE ( 'NONE', #1277, #14035, #15557, .T. ) ;
#21484 = CARTESIAN_POINT ( 'NONE',  ( 755.1538015810308480, -182.1908817542437760, -343.0433043558613804 ) ) ;
#21485 = CARTESIAN_POINT ( 'NONE',  ( 785.3687786644884454, -155.3618753856927128, -315.3201227861279676 ) ) ;
#21486 = CARTESIAN_POINT ( 'NONE',  ( 762.1405469898973024, -361.5436935675103882, -357.8594530101016176 ) ) ;
#21487 = ORIENTED_EDGE ( 'NONE', *, *, #18752, .F. ) ;
#21488 = CARTESIAN_POINT ( 'NONE',  ( 759.0252816721024374, -288.9982390220559978, 368.0189434323527280 ) ) ;
#21489 = CARTESIAN_POINT ( 'NONE',  ( 806.6271908675616942, -455.4127378225107350, 353.8200110890837777 ) ) ;
#21490 = CARTESIAN_POINT ( 'NONE',  ( 757.2208543904082489, -328.7146871989592682, 350.9844846989624330 ) ) ;
#21491 = DIRECTION ( 'NONE',  ( 0.000000000000000000, 0.000000000000000000, 1.000000000000000000 ) ) ;
#21492 = CARTESIAN_POINT ( 'NONE',  ( 804.8461984189677878, -170.1908817542438328, 336.9566956441385628 ) ) ;
#21493 = CARTESIAN_POINT ( 'NONE',  ( 765.0180583372156207, -24.99823902205683268, 360.0135310231089534 ) ) ;
#21494 = ORIENTED_EDGE ( 'NONE', *, *, #39098, .F. ) ;
#21495 = CARTESIAN_POINT ( 'NONE',  ( 757.7880784355613741, -378.0090635724250774, -312.4576283171834916 ) ) ;
#21496 = CARTESIAN_POINT ( 'NONE',  ( 767.7687537140311633, 0.09267006885218045942, -372.7932403749916830 ) ) ;
#21497 = CARTESIAN_POINT ( 'NONE',  ( 786.2694204179717872, -285.2817908451526137, 305.1769319972829067 ) ) ;
#21498 = CARTESIAN_POINT ( 'NONE',  ( 758.6633372737375112, -188.5328690171416497, 326.9102291470432533 ) ) ;
#21499 = CARTESIAN_POINT ( 'NONE',  ( 804.4286716492782716, -353.3618753856922012, -345.3141322388244703 ) ) ;
#21500 = CARTESIAN_POINT ( 'NONE',  ( 792.1044303154645831, 11.54721552339760038, 317.8323909638837677 ) ) ;
#21501 = DIRECTION ( 'NONE',  ( -0.000000000000000000, -0.000000000000000000, 1.000000000000000000 ) ) ;
#21502 = CARTESIAN_POINT ( 'NONE',  ( 784.1219089521767955, -213.2817908451527842, -315.0488828828318333 ) ) ;
#21503 = CARTESIAN_POINT ( 'NONE',  ( 814.5518280994195948, -15.72551174932958951, 332.4837098697145734 ) ) ;
#21504 = CARTESIAN_POINT ( 'NONE',  ( 811.0346526505616112, -86.63460265842023489, 323.0537975583477532 ) ) ;
#21505 = DIRECTION ( 'NONE',  ( -1.000000000000000000, -0.000000000000000000, 0.000000000000000000 ) ) ;
#21506 = CARTESIAN_POINT ( 'NONE',  ( 805.0032342141413437, -421.5436935675101040, -314.9967657858572352 ) ) ;
#21507 = CARTESIAN_POINT ( 'NONE',  ( 779.9999999999992042, -452.9681489794448339, 350.0000000000000000 ) ) ;
#21508 = CARTESIAN_POINT ( 'NONE',  ( 755.8990559732751535, -371.4636090269705164, 365.9055244015606831 ) ) ;
#21509 = PLANE ( 'NONE',  #3605 ) ;
#21510 = CARTESIAN_POINT ( 'NONE',  ( 777.5031285880264704, -334.8164208402376403, 374.9108240113588408 ) ) ;
#21511 = CARTESIAN_POINT ( 'NONE',  ( 814.9108240113580450, -64.27096629478397460, -337.5031285880265273 ) ) ;
#21512 = ADVANCED_FACE ( 'NONE', ( #22919 ), #4933, .F. ) ;
#21513 = CARTESIAN_POINT ( 'NONE',  ( 762.1405469898971887, -289.5436935675103882, -357.8594530101015607 ) ) ;
#21514 = CARTESIAN_POINT ( 'NONE',  ( 939.9999999999994316, -434.4637272565419153, 347.3621835540871530 ) ) ;
#21515 = CARTESIAN_POINT ( 'NONE',  ( 778.1981804954714335, -418.2709662947827383, 314.8072714833589885 ) ) ;
#21516 = VECTOR ( 'NONE', #6730, 1000.000000000000000 ) ;
#21517 = ADVANCED_FACE ( 'NONE', ( #29637, #26399, #8181, #18580, #15775, #1902, #40500, #22246, #37010, #8638, #32663, #7967, #22700, #36343, #16011 ), #12326, .T. ) ;
#21518 = CARTESIAN_POINT ( 'NONE',  ( 799.2566176426618085, -192.0090635724255606, 324.0069404352559559 ) ) ;
#21519 = CARTESIAN_POINT ( 'NONE',  ( 812.3518521366052028, -49.09997266333511590, -326.5853460496235243 ) ) ;
#21520 = CARTESIAN_POINT ( 'NONE',  ( 784.0799538623451781, -83.80559628986920018, -364.6971507214555572 ) ) ;
#21521 = CARTESIAN_POINT ( 'NONE',  ( 747.3154664389472828, -91.98741447168737295, 326.4474001241230781 ) ) ;
#21522 = CARTESIAN_POINT ( 'NONE',  ( 754.8072714833583632, -412.8164208402373561, 338.1981804954721156 ) ) ;
#21523 = CARTESIAN_POINT ( 'NONE',  ( 812.6845335610512393, -151.9874144716871740, 353.5525998758768651 ) ) ;
#21524 = CARTESIAN_POINT ( 'NONE',  ( 762.1405469898971887, -1.543693567511449150, -357.8594530101015607 ) ) ;
#21525 = VERTEX_POINT ( 'NONE', #44174 ) ;
#21526 = CARTESIAN_POINT ( 'NONE',  ( 755.3201227861273992, -99.72551174932928575, -345.3687786644892981 ) ) ;
#21527 = CARTESIAN_POINT ( 'NONE',  ( 773.3843516231979720, -397.4419599262317320, -364.4086373105754433 ) ) ;
#21529 = CARTESIAN_POINT ( 'NONE',  ( 788.8264449731201466, -237.1800572038742985, 363.6646147819170665 ) ) ;
#21528 = CARTESIAN_POINT ( 'NONE',  ( 768.0187753319979720, -224.6346026584198228, 318.0580252608186242 ) ) ;
#21530 = CARTESIAN_POINT ( 'NONE',  ( 768.8385539511368734, -407.2601417444137155, -306.4236121716840557 ) ) ;
#21531 = DIRECTION ( 'NONE',  ( -1.000000000000000000, 0.000000000000000000, 0.000000000000000000 ) ) ;
#21532 = VERTEX_POINT ( 'NONE', #39611 ) ;
#21533 = CARTESIAN_POINT ( 'NONE',  ( 788.7366044899766848, -419.9073299311465348, 316.5762568750059813 ) ) ;
#21534 = EDGE_LOOP ( 'NONE', ( #40580, #6823 ) ) ;
#21535 = CARTESIAN_POINT ( 'NONE',  ( 745.7998596910086917, -245.3618753856925139, -332.5602148656461168 ) ) ;
#21536 = CARTESIAN_POINT ( 'NONE',  ( 767.7687537140311633, -167.9073299311473022, 372.7932403749916830 ) ) ;
#21537 = CARTESIAN_POINT ( 'NONE',  ( 804.6971507214547046, -267.2817908451526137, 344.0799538623459739 ) ) ;
#21538 = ORIENTED_EDGE ( 'NONE', *, *, #33417, .T. ) ;
#21539 = CARTESIAN_POINT ( 'NONE',  ( 798.5707757039680246, -53.46360902697146855, -356.7845633553585003 ) ) ;
#21540 = CARTESIAN_POINT ( 'NONE',  ( 774.6312213355098493, -263.3618753856924286, -364.6798772138717482 ) ) ;
#21541 = ORIENTED_EDGE ( 'NONE', *, *, #36744, .F. ) ;
#21542 = CARTESIAN_POINT ( 'NONE',  ( 774.6858677611749044, -345.7255117493285184, -315.5713283507209894 ) ) ;
#21543 = CARTESIAN_POINT ( 'NONE',  ( 803.4237431249931660, -15.18005720387504631, -331.2633955100225194 ) ) ;
#21544 = CARTESIAN_POINT ( 'NONE',  ( 798.7617431975189675, -219.6237781080506295, 323.0428371773161871 ) ) ;
#21545 = CARTESIAN_POINT ( 'NONE',  ( 998.9999999999992042, -600.0000000000001137, 360.0000000000000000 ) ) ;
#21546 = CARTESIAN_POINT ( 'NONE',  ( 989.9999999999992042, -422.8782571739196783, 207.4246812887968190 ) ) ;
#21547 = ORIENTED_EDGE ( 'NONE', *, *, #29090, .F. ) ;
#21548 = CARTESIAN_POINT ( 'NONE',  ( 778.1981804954714335, -34.27096629478407408, -314.8072714833589885 ) ) ;
#21549 = DIRECTION ( 'NONE',  ( 1.000000000000000000, 0.000000000000000000, 0.000000000000000000 ) ) ;
#21550 = CARTESIAN_POINT ( 'NONE',  ( 914.9999999999992042, 74.99999999999984368, -360.0000000000000000 ) ) ;
#21551 = ORIENTED_EDGE ( 'NONE', *, *, #3479, .T. ) ;
#21552 = CARTESIAN_POINT ( 'NONE',  ( 776.2046728542105711, -284.1908817542434917, -304.8212110874238761 ) ) ;
#21553 = AXIS2_PLACEMENT_3D ( 'NONE', #10715, #10477, #21339 ) ;
#21554 = CARTESIAN_POINT ( 'NONE',  ( 746.4236121716829757, -135.8272453906076009, 328.8385539511384650 ) ) ;
#21556 = CARTESIAN_POINT ( 'NONE',  ( 765.0180583372156207, -240.9982390220561683, -360.0135310231089534 ) ) ;
#21555 = DIRECTION ( 'NONE',  ( 0.000000000000000000, 0.000000000000000000, 1.000000000000000000 ) ) ;
#21557 = DIRECTION ( 'NONE',  ( -1.000000000000000000, 0.000000000000000000, 0.000000000000000000 ) ) ;
#21558 = CARTESIAN_POINT ( 'NONE',  ( 796.1575198192839480, -102.0090635724258448, -359.4546378042384163 ) ) ;
#21559 = EDGE_CURVE ( 'NONE', #25862, #5020, #22470, .T. ) ;
#21560 = CARTESIAN_POINT ( 'NONE',  ( 757.7880784355613741, -378.0090635724250774, 312.4576283171834916 ) ) ;
#21561 = LINE ( 'NONE', #11401, #43151 ) ;
#21562 = CARTESIAN_POINT ( 'NONE',  ( 758.0141637701419768, 8.921676437403235127, -367.2620300519063790 ) ) ;
#21563 = CARTESIAN_POINT ( 'NONE',  ( 796.9462024416508257, -300.4527844766013231, -308.9653473494370246 ) ) ;
#21564 = FACE_OUTER_BOUND ( 'NONE', #35623, .T. ) ;
#21565 = CARTESIAN_POINT ( 'NONE',  ( 791.9812246680005501, 3.365397341579444479, 361.9419747391813189 ) ) ;
#21566 = CARTESIAN_POINT ( 'NONE',  ( 804.1009440267234822, -239.4636090269709143, 314.0944755984392600 ) ) ;
#21567 = CARTESIAN_POINT ( 'NONE',  ( 803.8556311672234642, -201.6237781080506863, -365.6418435158340117 ) ) ;
#21568 = CARTESIAN_POINT ( 'NONE',  ( 810.7187646348534145, -234.4527844766016358, 356.7737145352016341 ) ) ;
#21569 = CARTESIAN_POINT ( 'NONE',  ( 777.4774526936600978, -442.2709662947826814, -304.7301800767027657 ) ) ;
#21570 = EDGE_CURVE ( 'NONE', #25461, #3140, #3336, .T. ) ;
#21571 = EDGE_CURVE ( 'NONE', #45702, #27431, #8911, .T. ) ;
#21572 = DIRECTION ( 'NONE',  ( 0.000000000000000000, 0.7071067811865578978, 0.7071067811865372477 ) ) ;
#21573 = CARTESIAN_POINT ( 'NONE',  ( 756.5762568750052424, -315.1800572038740711, 348.7366044899774238 ) ) ;
#21574 = CARTESIAN_POINT ( 'NONE',  ( 799.2566176426618085, -96.00906357242585898, 324.0069404352559559 ) ) ;
#21575 = CARTESIAN_POINT ( 'NONE',  ( 757.0176451133909268, -85.09997266333499510, 349.9200121543848354 ) ) ;
#21576 = CARTESIAN_POINT ( 'NONE',  ( 803.4237431249931660, -447.1800572038736732, -331.2633955100225194 ) ) ;
#21577 = CARTESIAN_POINT ( 'NONE',  ( 786.4999999999993179, 323.4107432173689176, 352.9408934102648345 ) ) ;
#21578 = CARTESIAN_POINT ( 'NONE',  ( 779.9999999999992042, -452.9681489794448339, 329.9999999999999432 ) ) ;
#21580 = CARTESIAN_POINT ( 'NONE',  ( 792.1044303154645831, -348.4527844766012663, 317.8323909638837677 ) ) ;
#21579 = CARTESIAN_POINT ( 'NONE',  ( 757.2208543904082489, -160.7146871989598651, 350.9844846989624330 ) ) ;
#21581 = ORIENTED_EDGE ( 'NONE', *, *, #7658, .F. ) ;
#21582 = CARTESIAN_POINT ( 'NONE',  ( 766.7756240680305382, -278.5328690171412518, -361.5560724626415663 ) ) ;
#21583 = CARTESIAN_POINT ( 'NONE',  ( 756.5762568750052424, -123.1800572038747106, 348.7366044899774238 ) ) ;
#21584 = VECTOR ( 'NONE', #1224, 1000.000000000000000 ) ;
#21585 = CARTESIAN_POINT ( 'NONE',  ( 756.1443688327750579, -309.6237781080502600, -314.3581564841659315 ) ) ;
#21586 = CARTESIAN_POINT ( 'NONE',  ( 989.9999999999992042, 249.9999999999998863, -209.9999999999999716 ) ) ;
#21587 = CARTESIAN_POINT ( 'NONE',  ( 744.9990715423526808, -402.3510508353228374, 341.2370466360926002 ) ) ;
#21588 = ADVANCED_FACE ( 'NONE', ( #2425 ), #7857, .F. ) ;
#21589 = ORIENTED_EDGE ( 'NONE', *, *, #12079, .F. ) ;
#21590 = CARTESIAN_POINT ( 'NONE',  ( 804.9363028652555840, -328.2709662947831362, 338.2165204200192079 ) ) ;
#21591 = EDGE_CURVE ( 'NONE', #6854, #28329, #4383, .T. ) ;
#21592 = CARTESIAN_POINT ( 'NONE',  ( 787.6308680596127942, -83.26014174441466764, -364.1105419155492768 ) ) ;
#21593 = CARTESIAN_POINT ( 'NONE',  ( 800.0135310231082713, -158.0891481129655176, -325.0180583372163028 ) ) ;
#21594 = CARTESIAN_POINT ( 'NONE',  ( 803.4237431249931660, -207.1800572038744406, -331.2633955100225194 ) ) ;
#21595 = CARTESIAN_POINT ( 'NONE',  ( 758.0580252608178853, -414.4527844766010389, 328.0187753319985404 ) ) ;
#21596 = CARTESIAN_POINT ( 'NONE',  ( 777.5031285880264704, -142.8164208402382656, -374.9108240113588408 ) ) ;
#21597 = EDGE_CURVE ( 'NONE', #29996, #40012, #12890, .T. ) ;
#21598 = ORIENTED_EDGE ( 'NONE', *, *, #43293, .T. ) ;
#21599 = CARTESIAN_POINT ( 'NONE',  ( 762.3223304703356007, -151.5436935675109851, -322.3223304703362828 ) ) ;
#21600 = ORIENTED_EDGE ( 'NONE', *, *, #13183, .T. ) ;
#21601 = CARTESIAN_POINT ( 'NONE',  ( 763.8424801807145741, -378.0090635724250774, -320.5453621957614700 ) ) ;
#21602 = CARTESIAN_POINT ( 'NONE',  ( 776.9254006560222479, -452.1908817542428665, 314.8983024940802125 ) ) ;
#21603 = CARTESIAN_POINT ( 'NONE',  ( 769.1273215169530886, -142.7146871989599219, 317.4527132478988847 ) ) ;
#21606 = CARTESIAN_POINT ( 'NONE',  ( 808.7758568127978833, -388.1692326535045936, 320.0363995740631822 ) ) ;
#21605 = DIRECTION ( 'NONE',  ( 0.000000000000000000, 0.000000000000000000, 1.000000000000000000 ) ) ;
#21604 = CARTESIAN_POINT ( 'NONE',  ( 181.1634899080285948, 260.0000000000000000, -199.9999999999953957 ) ) ;
#21607 = ORIENTED_EDGE ( 'NONE', *, *, #16099, .T. ) ;
#21608 = CARTESIAN_POINT ( 'NONE',  ( 801.5560724626406000, -384.5545181178795247, -326.7756240680316182 ) ) ;
#21609 = DIRECTION ( 'NONE',  ( 0.000000000000000000, 0.000000000000000000, -1.000000000000000000 ) ) ;
#21610 = AXIS2_PLACEMENT_3D ( 'NONE', #28089, #10315, #42651 ) ;
#21611 = CARTESIAN_POINT ( 'NONE',  ( 748.6759233522253680, -184.3726999360619629, -324.3348316497537098 ) ) ;
#21612 = CARTESIAN_POINT ( 'NONE',  ( 752.7379699480933368, -36.00906357242605793, 361.9858362298580232 ) ) ;
#21614 = DIRECTION ( 'NONE',  ( 0.000000000000000000, -0.6438296778008192334, -0.7651688349527138167 ) ) ;
#21613 = DIRECTION ( 'NONE',  ( -0.000000000000000000, -0.000000000000000000, 1.000000000000000000 ) ) ;
#21615 = EDGE_CURVE ( 'NONE', #32511, #2565, #21756, .T. ) ;
#21616 = CARTESIAN_POINT ( 'NONE',  ( 754.8983024940795303, -306.8965053807775689, -336.9254006560228163 ) ) ;
#21617 = DIRECTION ( 'NONE',  ( 0.000000000000000000, -0.6438296778008156807, 0.7651688349527167032 ) ) ;
#21618 = CARTESIAN_POINT ( 'NONE',  ( 750.9282345327678740, -184.9181544815165239, -319.8311093483690115 ) ) ;
#21619 = DIRECTION ( 'NONE',  ( -1.000000000000000000, 0.000000000000000000, 0.000000000000000000 ) ) ;
#21620 = CARTESIAN_POINT ( 'NONE',  ( 779.9999999999992042, -462.9681489794448339, 339.9999999999999432 ) ) ;
#21621 = CARTESIAN_POINT ( 'NONE',  ( 761.4292242960306112, -377.4636090269704596, 323.2154366446414429 ) ) ;
#21622 = ADVANCED_FACE ( 'NONE', ( #36020, #16069, #1517 ), #30609, .T. ) ;
#21623 = CARTESIAN_POINT ( 'NONE',  ( 762.1177392798416577, -330.5545181178796952, 309.8865473780659272 ) ) ;
#21624 = CARTESIAN_POINT ( 'NONE',  ( 808.3070685750232087, -210.9982390220562252, -361.1904061080339829 ) ) ;
#21625 = CARTESIAN_POINT ( 'NONE',  ( 799.9999999999993179, -462.9681489794448339, -309.9999999999998863 ) ) ;
#21626 = CARTESIAN_POINT ( 'NONE',  ( 803.6646147819161570, 6.092670068852159559, -348.8264449731210561 ) ) ;
#21627 = CARTESIAN_POINT ( 'NONE',  ( 754.3581564841646241, -137.4636090269711985, 316.1443688327762516 ) ) ;
#21628 = CARTESIAN_POINT ( 'NONE',  ( 795.6651683502461765, -82.71468719896012090, -371.3240766477733814 ) ) ;
#21629 = CARTESIAN_POINT ( 'NONE',  ( 758.8095938919642549, -104.0891481129656881, 311.6929314249763365 ) ) ;
#21630 = CARTESIAN_POINT ( 'NONE',  ( 751.9810565676468741, -338.0891481129649492, -360.9747183278973921 ) ) ;
#21631 = EDGE_CURVE ( 'NONE', #21185, #38193, #6992, .T. ) ;
#21632 = DIRECTION ( 'NONE',  ( 0.000000000000000000, 0.000000000000000000, -1.000000000000000000 ) ) ;
#21633 = LINE ( 'NONE', #35715, #30152 ) ;
#21634 = CARTESIAN_POINT ( 'NONE',  ( 804.9363028652555840, -208.2709662947835341, 338.2165204200192079 ) ) ;
#21635 = CARTESIAN_POINT ( 'NONE',  ( 805.6418435158337843, -461.4636090269701754, 363.8556311672236916 ) ) ;
#21636 = CARTESIAN_POINT ( 'NONE',  ( 763.2262854647970016, -416.6346026584192259, -309.2812353651462445 ) ) ;
#21637 = CARTESIAN_POINT ( 'NONE',  ( 911.9749999999993406, 154.9999999999998863, 360.0000000000000000 ) ) ;
#21638 = CARTESIAN_POINT ( 'NONE',  ( 815.1787889125755555, 17.10349461922139369, 343.7953271457877804 ) ) ;
#21639 = ORIENTED_EDGE ( 'NONE', *, *, #39584, .T. ) ;
#21640 = AXIS2_PLACEMENT_3D ( 'NONE', #37582, #15658, #12199 ) ;
#21641 = CARTESIAN_POINT ( 'NONE',  ( 785.3687786644884454, -35.36187538569316047, 315.3201227861279676 ) ) ;
#21642 = CARTESIAN_POINT ( 'NONE',  ( 815.0009284576459549, -174.3510508353234627, -338.7629533639073429 ) ) ;
#21643 = SURFACE_STYLE_FILL_AREA ( #39215 ) ;
#21644 = CARTESIAN_POINT ( 'NONE',  ( 764.3348316497523456, -310.7146871989593251, 308.6759233522265617 ) ) ;
#21645 = CARTESIAN_POINT ( 'NONE',  ( 797.6776695296629214, -163.5436935675109567, 357.6776695296636603 ) ) ;
#21646 = AXIS2_PLACEMENT_3D ( 'NONE', #34388, #13380, #44801 ) ;
#21647 = ORIENTED_EDGE ( 'NONE', *, *, #23279, .T. ) ;
#21648 = CARTESIAN_POINT ( 'NONE',  ( 804.6798772138708955, -303.7255117493287457, 334.6312213355107019 ) ) ;
#21649 = CARTESIAN_POINT ( 'NONE',  ( 808.3070685750230950, -42.99823902205675807, -361.1904061080339261 ) ) ;
#21650 = CARTESIAN_POINT ( 'NONE',  ( 767.6429770376291799, -81.18005720387482427, 306.8695393053162093 ) ) ;
#21651 = ORIENTED_EDGE ( 'NONE', *, *, #14268, .F. ) ;
#21652 = CARTESIAN_POINT ( 'NONE',  ( 809.0717654672305343, -460.9181544815156713, -360.1688906516309885 ) ) ;
#21653 = EDGE_LOOP ( 'NONE', ( #35379, #21811, #30902, #5120 ) ) ;
#21654 = SHAPE_DEFINITION_REPRESENTATION ( #42502, #20360 ) ;
#21655 = VECTOR ( 'NONE', #5679, 1000.000000000000000 ) ;
#21656 = CARTESIAN_POINT ( 'NONE',  ( 804.4286716492782716, -65.36187538569306810, 345.3141322388244703 ) ) ;
#21657 = CARTESIAN_POINT ( 'NONE',  ( 781.7834795799800531, -298.8164208402377540, -315.0636971347436202 ) ) ;
#21659 = CARTESIAN_POINT ( 'NONE',  ( 786.2056067578752163, -299.8055962898685038, 374.4686193811670023 ) ) ;
#21658 = CARTESIAN_POINT ( 'NONE',  ( 772.4837098697145166, -383.3618753856920875, 374.5518280994205611 ) ) ;
#21660 = CARTESIAN_POINT ( 'NONE',  ( 812.6845335610512393, -55.98741447168748664, 353.5525998758768651 ) ) ;
#21661 = CARTESIAN_POINT ( 'NONE',  ( 779.4763451958990572, -272.7363362996981095, -365.0264073115438919 ) ) ;
#21662 = CARTESIAN_POINT ( 'NONE',  ( 778.1981804954714335, -274.2709662947833067, -314.8072714833589885 ) ) ;
#21663 = CARTESIAN_POINT ( 'NONE',  ( 799.9999999999993179, -512.9681489794448908, 370.0000000000000000 ) ) ;
#21664 = CARTESIAN_POINT ( 'NONE',  ( 759.7806653035534055, -102.9982390220565520, -324.8639956371180801 ) ) ;
#21665 = CARTESIAN_POINT ( 'NONE',  ( 810.7187646348534145, -378.4527844766011526, 356.7737145352016341 ) ) ;
#21667 = CARTESIAN_POINT ( 'NONE',  ( -468.8365100919714337, 260.0000000000001705, -202.7499999999907345 ) ) ;
#21666 = CARTESIAN_POINT ( 'NONE',  ( 989.9999999999992042, -426.1357934546398383, 350.0000000000000000 ) ) ;
#21668 = CARTESIAN_POINT ( 'NONE',  ( 764.1737431748507561, -82.37269993606227558, -371.6461892240376415 ) ) ;
#21669 = FACE_OUTER_BOUND ( 'NONE', #30799, .T. ) ;
#21670 = CARTESIAN_POINT ( 'NONE',  ( 879.9999999999992042, 99.99999999999984368, 350.0000000000000000 ) ) ;
#21671 = CARTESIAN_POINT ( 'NONE',  ( 769.9779781133707957, -259.0999726633343698, 316.7813123517150871 ) ) ;
#21672 = CARTESIAN_POINT ( 'NONE',  ( 762.1405469898971887, -169.5436935675108430, 357.8594530101015607 ) ) ;
#21673 = ORIENTED_EDGE ( 'NONE', *, *, #24578, .F. ) ;
#21674 = CARTESIAN_POINT ( 'NONE',  ( 755.8894580844503253, -39.82724539060786384, -332.3691319403863531 ) ) ;
#21675 = AXIS2_PLACEMENT_3D ( 'NONE', #24174, #3157, #10320 ) ;
#21676 = AXIS2_PLACEMENT_3D ( 'NONE', #33836, #37061, #9359 ) ;
#21677 = CARTESIAN_POINT ( 'NONE',  ( 792.3570229623691148, -93.18005720387479585, -373.1304606946836770 ) ) ;
#21678 = CARTESIAN_POINT ( 'NONE',  ( 805.1016975059191054, -342.8965053807773984, 343.0745993439771837 ) ) ;
#21679 = CARTESIAN_POINT ( 'NONE',  ( -959.5497976682736407, 240.0000000000002274, -2132.806278688367456 ) ) ;
#21680 = CARTESIAN_POINT ( 'NONE',  ( 783.7953271457878373, -32.19088175424425913, 375.1787889125761239 ) ) ;
#21681 = CARTESIAN_POINT ( 'NONE',  ( 748.9653473494363425, -218.6346026584197944, -356.9462024416521331 ) ) ;
#21682 = CARTESIAN_POINT ( 'NONE',  ( 758.8095938919642549, -200.0891481129653187, 311.6929314249763365 ) ) ;
#21683 = CARTESIAN_POINT ( 'NONE',  ( 756.5762568750052424, -99.18005720387478164, 348.7366044899774238 ) ) ;
#21684 = CARTESIAN_POINT ( 'NONE',  ( 746.0683387631852383, -307.4419599262320730, -331.3260364891676204 ) ) ;
#21685 = VECTOR ( 'NONE', #7708, 1000.000000000000114 ) ;
#21686 = CARTESIAN_POINT ( 'NONE',  ( 755.8990559732751535, -443.4636090269702322, 365.9055244015606831 ) ) ;
#21687 = CARTESIAN_POINT ( 'NONE',  ( 782.4968714119720516, -322.8164208402377540, -305.0891759886411023 ) ) ;
#21688 = DIRECTION ( 'NONE',  ( 0.000000000000000000, 0.000000000000000000, 1.000000000000000000 ) ) ;
#21689 = CARTESIAN_POINT ( 'NONE',  ( 754.8983024940795303, -378.8965053807772847, 336.9254006560228163 ) ) ;
#21690 = CARTESIAN_POINT ( 'NONE',  ( 755.2512626584698410, -55.54369356751127640, 315.2512626584710915 ) ) ;
#21691 = CARTESIAN_POINT ( 'NONE',  ( 778.1981804954714335, -418.2709662947827383, -314.8072714833589885 ) ) ;
#21692 = CARTESIAN_POINT ( 'NONE',  ( 801.3366627262608972, -56.53286901714201917, 353.0897708529566899 ) ) ;
#21693 = CARTESIAN_POINT ( 'NONE',  ( 752.4576283171824116, -69.07832356259653750, -317.7880784355627952 ) ) ;
#21694 = CARTESIAN_POINT ( 'NONE',  ( 788.7631598425961101, -193.4419599262325278, 305.7194118038759143 ) ) ;
#21695 = CARTESIAN_POINT ( 'NONE',  ( 797.6776695296629214, -19.54369356751139364, 357.6776695296636603 ) ) ;
#21696 = ORIENTED_EDGE ( 'NONE', *, *, #17723, .F. ) ;
#21697 = CARTESIAN_POINT ( 'NONE',  ( 800.7704444035546203, -196.1692326535052473, -326.0291762391768771 ) ) ;
#21698 = CARTESIAN_POINT ( 'NONE',  ( 759.7806653035534055, -198.9982390220562252, 324.8639956371180801 ) ) ;
#21699 = CARTESIAN_POINT ( 'NONE',  ( 800.1688906516307043, -34.16923265350572336, -369.0717654672308186 ) ) ;
#21700 = CARTESIAN_POINT ( 'NONE',  ( 801.9419747391806368, -330.4527844766013231, 351.9812246680014027 ) ) ;
#21701 =( GEOMETRIC_REPRESENTATION_CONTEXT ( 3 ) GLOBAL_UNCERTAINTY_ASSIGNED_CONTEXT ( ( #21814 ) ) GLOBAL_UNIT_ASSIGNED_CONTEXT ( ( #20394, #13478, #41652 ) ) REPRESENTATION_CONTEXT ( 'NONE', 'WORKASPACE' ) );
#21702 = CARTESIAN_POINT ( 'NONE',  ( 798.5757817331792694, -452.9681489794448339, -357.1584183591081683 ) ) ;
#21703 = DIRECTION ( 'NONE',  ( 1.000000000000000000, 0.000000000000000000, 0.000000000000000000 ) ) ;
#21704 = VECTOR ( 'NONE', #6736, 1000.000000000000000 ) ;
#21705 = VERTEX_POINT ( 'NONE', #12601 ) ;
#21706 = CARTESIAN_POINT ( 'NONE',  ( 794.1144889064781864, -34.16923265350572336, 360.9840315886528401 ) ) ;
#21707 = CARTESIAN_POINT ( 'NONE',  ( 747.6481478633932056, -349.0999726633342561, -353.4146539503763620 ) ) ;
#21708 = CARTESIAN_POINT ( 'NONE',  ( 745.7998596910086917, -293.3618753856923718, 332.5602148656461168 ) ) ;
#21709 = CARTESIAN_POINT ( 'NONE',  ( 803.8556311672234642, -9.623778108051251223, 365.6418435158340117 ) ) ;
#21710 = CARTESIAN_POINT ( 'NONE',  ( 798.5707757039680246, -197.4636090269709996, -356.7845633553585003 ) ) ;
#21711 = CARTESIAN_POINT ( 'NONE',  ( 804.9363028652555840, -184.2709662947835909, -338.2165204200192079 ) ) ;
#21712 = CARTESIAN_POINT ( 'NONE',  ( 759.7806653035535192, -342.9982390220557704, -324.8639956371181370 ) ) ;
#21713 = VERTEX_POINT ( 'NONE', #43772 ) ;
#21714 = CARTESIAN_POINT ( 'NONE',  ( 757.2208543904082489, 7.285312801039605546, -350.9844846989624330 ) ) ;
#21715 = CARTESIAN_POINT ( 'NONE',  ( 782.4968714119720516, -298.8164208402377540, 305.0891759886411023 ) ) ;
#21716 = AXIS2_PLACEMENT_3D ( 'NONE', #43401, #36461, #895 ) ;
#21717 = DIRECTION ( 'NONE',  ( -0.000000000000000000, 1.000000000000000000, -0.000000000000000000 ) ) ;
#21718 = CARTESIAN_POINT ( 'NONE',  ( 780.5236548040995785, -212.7363362996982232, 314.9735926884559944 ) ) ;
#21719 = LINE ( 'NONE', #35813, #3941 ) ;
#21720 = AXIS2_PLACEMENT_3D ( 'NONE', #12819, #19984, #13517 ) ;
#21721 = CARTESIAN_POINT ( 'NONE',  ( 805.2837595273609850, -146.7363362996984506, 340.5290396650784714 ) ) ;
#21722 = CARTESIAN_POINT ( 'NONE',  ( 778.2165204200184689, -46.81642084023858530, 364.9363028652563230 ) ) ;
#21723 = VERTEX_POINT ( 'NONE', #25382 ) ;
#21724 = CARTESIAN_POINT ( 'NONE',  ( 752.7379699480933368, -396.0090635724249637, -361.9858362298580232 ) ) ;
#21725 = CARTESIAN_POINT ( 'NONE',  ( 755.2512626584698410, -7.543693567511430942, -315.2512626584710915 ) ) ;
#21726 = CARTESIAN_POINT ( 'NONE',  ( 747.6481478633932056, -253.0999726633345119, 353.4146539503763620 ) ) ;
#21727 = CARTESIAN_POINT ( 'NONE',  ( 757.2208543904082489, -232.7146871989596377, 350.9844846989624330 ) ) ;
#21728 = CARTESIAN_POINT ( 'NONE',  ( 788.7366044899766848, -371.9073299311465917, -316.5762568750059813 ) ) ;
#21729 = CARTESIAN_POINT ( 'NONE',  ( -786.4999999999993179, -365.3551492539851893, -18.13243251470705886 ) ) ;
#21730 = CARTESIAN_POINT ( 'NONE',  ( 755.0636971347428243, -4.270966294784170003, 341.7834795799807353 ) ) ;
#21731 = CARTESIAN_POINT ( 'NONE',  ( 801.5560724626406000, -216.5545181178800931, -326.7756240680316182 ) ) ;
#21732 = CARTESIAN_POINT ( 'NONE',  ( 759.0252816721024374, -24.99823902205683268, 368.0189434323527280 ) ) ;
#21733 = CARTESIAN_POINT ( 'NONE',  ( 805.0032342141412300, -109.5436935675110988, 314.9967657858571783 ) ) ;
#21734 = LINE ( 'NONE', #264, #26904 ) ;
#21735 = CARTESIAN_POINT ( 'NONE',  ( -784.4999999999993179, -496.5085659523897448, -356.8883017825714319 ) ) ;
#21736 = CIRCLE ( 'NONE', #1801, 8.000000000000007105 ) ;
#21737 = CARTESIAN_POINT ( 'NONE',  ( -39.63011601220123481, -365.3551492539851893, -8.132432514707076621 ) ) ;
#21738 = CARTESIAN_POINT ( 'NONE',  ( 814.4686193811664907, -387.2817908451522726, 346.2056067578752732 ) ) ;
#21739 = CARTESIAN_POINT ( 'NONE',  ( -769.9999999999992042, 205.0000000000000568, -339.9999999999999432 ) ) ;
#21740 = CARTESIAN_POINT ( 'NONE',  ( 749.2812353651451076, -342.4527844766013231, 323.2262854647983090 ) ) ;
#21741 = CARTESIAN_POINT ( 'NONE',  ( 747.2067596250078623, -99.18005720387478164, -352.2312462859687230 ) ) ;
#21742 = CARTESIAN_POINT ( 'NONE',  ( 791.9812246680005501, -284.6346026584196807, -361.9419747391813189 ) ) ;
#21743 = LINE ( 'NONE', #28689, #39501 ) ;
#21744 = CARTESIAN_POINT ( 'NONE',  ( 781.7834795799800531, -442.8164208402372992, 315.0636971347436202 ) ) ;
#21745 = AXIS2_PLACEMENT_3D ( 'NONE', #9004, #33487, #36734 ) ;
#21746 = CARTESIAN_POINT ( 'NONE',  ( 754.7162404726377645, -182.7363362996983369, 339.4709603349214717 ) ) ;
#21747 = CARTESIAN_POINT ( 'NONE',  ( 814.8207195650702488, -50.19088175424420939, -336.2433038121456548 ) ) ;
#21748 = CARTESIAN_POINT ( 'NONE',  ( 769.1273215169530886, -94.71468719896007826, -317.4527132478988847 ) ) ;
#21749 = CARTESIAN_POINT ( 'NONE',  ( 781.2497674668890113, -108.3510508353236759, 375.3608509340180603 ) ) ;
#21750 = CARTESIAN_POINT ( 'NONE',  ( 788.8264449731201466, -405.1800572038737869, 363.6646147819170665 ) ) ;
#21751 = VECTOR ( 'NONE', #4544, 1000.000000000000000 ) ;
#21752 = CARTESIAN_POINT ( 'NONE',  ( 811.6461892240364477, -148.7146871989598935, 324.1737431748509835 ) ) ;
#21753 = CARTESIAN_POINT ( 'NONE',  ( 756.3353852180819104, -5.907329931147798696, -331.1735550268788302 ) ) ;
#21754 = ORIENTED_EDGE ( 'NONE', *, *, #13193, .F. ) ;
#21755 = CARTESIAN_POINT ( 'NONE',  ( 788.8264449731200330, -93.18005720387481006, -363.6646147819171233 ) ) ;
#21756 = CIRCLE ( 'NONE', #11449, 6.119000000000013095 ) ;
#21757 = AXIS2_PLACEMENT_3D ( 'NONE', #9184, #39551, #22583 ) ;
#21758 = CARTESIAN_POINT ( 'NONE',  ( 766.7756240680305382, -398.5328690171409107, -361.5560724626415663 ) ) ;
#21760 = CARTESIAN_POINT ( 'NONE',  ( 800.0135310231082713, -230.0891481129652618, 325.0180583372163028 ) ) ;
#21759 = CARTESIAN_POINT ( 'NONE',  ( 800.2193346964447755, -210.9982390220561967, 355.1360043628815788 ) ) ;
#21761 = CARTESIAN_POINT ( 'NONE',  ( 798.0661480581538854, -410.5328690171408539, -309.5768839229118043 ) ) ;
#21762 = DIRECTION ( 'NONE',  ( -0.000000000000000000, 1.000000000000000000, -0.000000000000000000 ) ) ;
#21763 = ORIENTED_EDGE ( 'NONE', *, *, #33741, .F. ) ;
#21764 = CARTESIAN_POINT ( 'NONE',  ( 755.3201227861273992, -411.7255117493282910, 345.3687786644892981 ) ) ;
#21765 = ORIENTED_EDGE ( 'NONE', *, *, #13710, .F. ) ;
#21766 = CARTESIAN_POINT ( 'NONE',  ( 808.0189434323515343, -254.0891481129652334, -319.0252816721025511 ) ) ;
#21767 = CARTESIAN_POINT ( 'NONE',  ( 792.3570229623691148, -189.1800572038744690, 373.1304606946836770 ) ) ;
#21768 = AXIS2_PLACEMENT_3D ( 'NONE', #35371, #45563, #13457 ) ;
#21769 = CARTESIAN_POINT ( 'NONE',  ( 779.4763451958990572, -248.7363362996981380, 365.0264073115438919 ) ) ;
#21770 = ORIENTED_EDGE ( 'NONE', *, *, #17335, .T. ) ;
#21771 = CARTESIAN_POINT ( 'NONE',  ( 776.9254006560222479, -68.19088175424413123, -314.8983024940802125 ) ) ;
#21772 = CARTESIAN_POINT ( 'NONE',  ( 803.6646147819162707, -233.9073299311470464, -348.8264449731211130 ) ) ;
#21773 = AXIS2_PLACEMENT_3D ( 'NONE', #678, #446, #43168 ) ;
#21774 = ORIENTED_EDGE ( 'NONE', *, *, #8131, .F. ) ;
#21775 = CARTESIAN_POINT ( 'NONE',  ( 797.6776695296629214, -379.5436935675102745, -357.6776695296636603 ) ) ;
#21776 = CARTESIAN_POINT ( 'NONE',  ( 774.6858677611749044, -57.72551174932945628, -315.5713283507209894 ) ) ;
#21777 = CIRCLE ( 'NONE', #1843, 2.749999999999919176 ) ;
#21778 = CARTESIAN_POINT ( 'NONE',  ( 805.0264073115434940, -246.3510508353232638, 339.4763451958999099 ) ) ;
#21779 = CARTESIAN_POINT ( 'NONE',  ( -454.7528517110260964, 240.0000000000001421, -122.7905160835438068 ) ) ;
#21780 = CARTESIAN_POINT ( 'NONE',  ( 521.6730038022808458, 239.9999999999999432, -122.7905160835442615 ) ) ;
#21781 = CARTESIAN_POINT ( 'NONE',  ( 771.2633955100217236, -23.90732993114773919, -363.4237431249939618 ) ) ;
#21782 = CARTESIAN_POINT ( 'NONE',  ( 914.9999999999992042, -426.1357934546398383, -350.0000000000000000 ) ) ;
#21783 = DIRECTION ( 'NONE',  ( 1.000000000000000000, 0.000000000000000000, -0.000000000000000000 ) ) ;
#21784 = ORIENTED_EDGE ( 'NONE', *, *, #41912, .F. ) ;
#21785 = CARTESIAN_POINT ( 'NONE',  ( 766.4474001241216001, -307.0999726633343130, -307.3154664389482491 ) ) ;
#21786 = CARTESIAN_POINT ( 'NONE',  ( 749.5768839229115201, -156.5545181178802636, 358.0661480581553064 ) ) ;
#21787 = AXIS2_PLACEMENT_3D ( 'NONE', #12386, #33849, #22536 ) ;
#21789 = CARTESIAN_POINT ( 'NONE',  ( 755.0636971347428243, -244.2709662947834204, -341.7834795799807353 ) ) ;
#21788 = FACE_OUTER_BOUND ( 'NONE', #15199, .T. ) ;
#21790 = FACE_OUTER_BOUND ( 'NONE', #1473, .T. ) ;
#21791 = CARTESIAN_POINT ( 'NONE',  ( 776.9254006560222479, -116.1908817542440033, -314.8983024940802125 ) ) ;
#21792 = AXIS2_PLACEMENT_3D ( 'NONE', #20606, #6527, #41411 ) ;
#21793 = CARTESIAN_POINT ( 'NONE',  ( 181.1634899080285948, 240.0000000000000284, -197.2499999999955662 ) ) ;
#21794 = CARTESIAN_POINT ( 'NONE',  ( 746.0683387631852383, -19.44195992623303937, -331.3260364891676204 ) ) ;
#21795 = CARTESIAN_POINT ( 'NONE',  ( 767.6429770376291799, -297.1800572038741279, -306.8695393053162093 ) ) ;
#21796 = DIRECTION ( 'NONE',  ( -0.000000000000000000, 1.000000000000000000, -0.000000000000000000 ) ) ;
#21797 = CARTESIAN_POINT ( 'NONE',  ( 792.1044303154645831, -12.45278447660232146, 317.8323909638837677 ) ) ;
#21798 = CARTESIAN_POINT ( 'NONE',  ( 755.8990559732751535, -251.4636090269709143, 365.9055244015606831 ) ) ;
#21799 = CARTESIAN_POINT ( 'NONE',  ( 768.8385539511368734, -215.2601417444141987, -306.4236121716840557 ) ) ;
#21800 = CARTESIAN_POINT ( 'NONE',  ( 767.7687537140311633, -215.9073299311471317, 372.7932403749916830 ) ) ;
#21801 = CARTESIAN_POINT ( 'NONE',  ( 804.7487373415286811, -451.5436935675099903, -364.7487373415288516 ) ) ;
#21802 = CARTESIAN_POINT ( 'NONE',  ( 775.4999999999993179, -496.5085659523897448, -356.8883017825714319 ) ) ;
#21803 = CARTESIAN_POINT ( 'NONE',  ( 802.1676090361156639, -326.6346026584193396, 327.8955696845344505 ) ) ;
#21804 = CARTESIAN_POINT ( 'NONE',  ( 763.0428371773158460, -83.46360902697136908, 358.7617431975195359 ) ) ;
#21805 = CARTESIAN_POINT ( 'NONE',  ( 795.9930595647434757, 20.92167643740319605, -320.7433823573372820 ) ) ;
#21806 = CIRCLE ( 'NONE', #27706, 10.00000000000000888 ) ;
#21807 = PLANE ( 'NONE',  #401 ) ;
#21808 = DIRECTION ( 'NONE',  ( -4.625929269271485914E-16, 1.000000000000000000, 0.000000000000000000 ) ) ;
#21810 = CARTESIAN_POINT ( 'NONE',  ( 774.6858677611749044, -369.7255117493284615, 315.5713283507209894 ) ) ;
#21809 = CARTESIAN_POINT ( 'NONE',  ( 804.9511171171677688, -149.8055962898689870, 335.8780910478229202 ) ) ;
#21811 = ORIENTED_EDGE ( 'NONE', *, *, #34823, .F. ) ;
#21812 = CIRCLE ( 'NONE', #40261, 8.024999999999948841 ) ;
#21813 = CARTESIAN_POINT ( 'NONE',  ( 759.2295555964440155, -280.1692326535049347, -353.9708237608231229 ) ) ;
#21814 = UNCERTAINTY_MEASURE_WITH_UNIT (LENGTH_MEASURE( 1.000000000000000082E-05 ), #20394, 'distance_accuracy_value', 'NONE');
#21815 = CARTESIAN_POINT ( 'NONE',  ( 778.2165204200184689, -142.8164208402382656, 364.9363028652563230 ) ) ;
#21816 = CARTESIAN_POINT ( 'NONE',  ( 778.7502325331095108, -288.3510508353231216, -304.6391490659818828 ) ) ;
#21817 = DIRECTION ( 'NONE',  ( 0.000000000000000000, 0.000000000000000000, -1.000000000000000000 ) ) ;
#21818 = CARTESIAN_POINT ( 'NONE',  ( 763.2262854647970016, 15.36539734157940629, 309.2812353651462445 ) ) ;
#21819 = ORIENTED_EDGE ( 'NONE', *, *, #17010, .T. ) ;
#21820 = CARTESIAN_POINT ( 'NONE',  ( 759.9864689768902508, -338.0891481129649492, 354.9819416627836404 ) ) ;
#21821 = CARTESIAN_POINT ( 'NONE',  ( 761.2382568024794409, -87.62377810805102740, -356.9571628226838129 ) ) ;
#21822 = CARTESIAN_POINT ( 'NONE',  ( 805.1927285166397041, -448.8164208402371855, 341.8018195045277707 ) ) ;
#21823 = CIRCLE ( 'NONE', #7101, 9.999999999999980460 ) ;
#21824 = EDGE_CURVE ( 'NONE', #19590, #19031, #45376, .T. ) ;
#21825 = CARTESIAN_POINT ( 'NONE',  ( 814.9108240113580450, -160.2709662947836762, -337.5031285880265273 ) ) ;
#21826 = ORIENTED_EDGE ( 'NONE', *, *, #14121, .T. ) ;
#21827 = CARTESIAN_POINT ( 'NONE',  ( 788.7366044899766848, -131.9073299311473875, -316.5762568750059813 ) ) ;
#21828 = VERTEX_POINT ( 'NONE', #41012 ) ;
#21829 = CARTESIAN_POINT ( 'NONE',  ( 800.9840315886518738, -412.9181544815157281, -354.1144889064786412 ) ) ;
#21830 = CARTESIAN_POINT ( 'NONE',  ( 802.9823548866075953, -457.0999726633339151, 330.0799878456151077 ) ) ;
#21831 = CARTESIAN_POINT ( 'NONE',  ( 815.2698199232961542, -232.8164208402379245, 342.5225473063383106 ) ) ;
#21832 = CARTESIAN_POINT ( 'NONE',  ( 755.8398074228967971, -139.4419599262326699, 333.4516893846970333 ) ) ;
#21835 = CARTESIAN_POINT ( 'NONE',  ( 749.8865473780648472, -380.5328690171409676, 322.1177392798429082 ) ) ;
#21834 = DIRECTION ( 'NONE',  ( 0.000000000000000000, -0.000000000000000000, -1.000000000000000000 ) ) ;
#21833 = CARTESIAN_POINT ( 'NONE',  ( 775.4999999999993179, -563.3203001761231690, -342.3463313526983143 ) ) ;
#21836 = EDGE_CURVE ( 'NONE', #29708, #15262, #5670, .T. ) ;
#21837 = ORIENTED_EDGE ( 'NONE', *, *, #30318, .T. ) ;
#21838 = CARTESIAN_POINT ( 'NONE',  ( 790.9844846989617508, -382.3726999360613945, -317.2208543904092721 ) ) ;
#21839 = DIRECTION ( 'NONE',  ( -1.000000000000000000, 0.000000000000000000, 0.000000000000000000 ) ) ;
#21840 = CARTESIAN_POINT ( 'NONE',  ( 760.0363995740630116, -178.9181544815165239, -368.7758568127991907 ) ) ;
#21841 = CARTESIAN_POINT ( 'NONE',  ( 793.5525998758768083, -55.09997266333508747, 372.6845335610516941 ) ) ;
#21842 = VECTOR ( 'NONE', #34501, 1000.000000000000000 ) ;
#21844 = DIRECTION ( 'NONE',  ( -0.000000000000000000, 1.000000000000000000, -0.000000000000000000 ) ) ;
#21843 = DIRECTION ( 'NONE',  ( 0.000000000000000000, 0.000000000000000000, 1.000000000000000000 ) ) ;
#21845 = CARTESIAN_POINT ( 'NONE',  ( 803.8651313633788504, -317.2601417444139429, -332.4468031744301015 ) ) ;
#21846 = FACE_OUTER_BOUND ( 'NONE', #34442, .T. ) ;
#21848 = AXIS2_PLACEMENT_3D ( 'NONE', #34520, #10481, #23871 ) ;
#21847 = CARTESIAN_POINT ( 'NONE',  ( 793.5525998758768083, -175.0999726633346825, -372.6845335610516941 ) ) ;
#21849 = CARTESIAN_POINT ( 'NONE',  ( -775.4999999999993179, -563.3203001761231690, -342.3463313526983143 ) ) ;
#21850 = DIRECTION ( 'NONE',  ( -1.000000000000000000, 1.892425610156518354E-16, 0.000000000000000000 ) ) ;
#21851 = VECTOR ( 'NONE', #21609, 1000.000000000000000 ) ;
#21852 = CARTESIAN_POINT ( 'NONE',  ( 757.0176451133909268, -373.0999726633340856, 349.9200121543848354 ) ) ;
#21853 = CARTESIAN_POINT ( 'NONE',  ( 754.3581564841646241, -353.4636090269705733, 316.1443688327762516 ) ) ;
#21854 = CARTESIAN_POINT ( 'NONE',  ( 746.8695393053151292, -221.9073299311471033, -327.6429770376306578 ) ) ;
#21855 = EDGE_CURVE ( 'NONE', #24181, #32406, #40349, .T. ) ;
#21856 = DIRECTION ( 'NONE',  ( 0.000000000000000000, 0.000000000000000000, 1.000000000000000000 ) ) ;
#21857 = CARTESIAN_POINT ( 'NONE',  ( 759.9864689768902508, -2.089148112965993231, -354.9819416627836404 ) ) ;
#21858 = AXIS2_PLACEMENT_3D ( 'NONE', #36916, #30677, #2486 ) ;
#21859 = CARTESIAN_POINT ( 'NONE',  ( 745.7194118038753459, -133.6454272087893571, 348.7631598425976449 ) ) ;
#21860 = EDGE_CURVE ( 'NONE', #17501, #21525, #9372, .T. ) ;
#21861 = CARTESIAN_POINT ( 'NONE',  ( 744.9990715423526808, -90.35105083532373271, -341.2370466360926002 ) ) ;
#21862 = CARTESIAN_POINT ( 'NONE',  ( 811.0346526505616112, -110.6346026584201638, 323.0537975583477532 ) ) ;
#21863 = CARTESIAN_POINT ( 'NONE',  ( 777.4774526936600978, -346.2709662947830793, -304.7301800767027657 ) ) ;
#21864 = CIRCLE ( 'NONE', #1926, 10.00000000000000888 ) ;
#21865 = CARTESIAN_POINT ( 'NONE',  ( -773.4999999999993179, -513.1383975375929367, -369.9999999999999432 ) ) ;
#21866 = DIRECTION ( 'NONE',  ( -0.000000000000000000, 0.3835384033298669948, 0.9235249282889858025 ) ) ;
#21867 = ADVANCED_FACE ( 'NONE', ( #22767 ), #40775, .T. ) ;
#21868 = CARTESIAN_POINT ( 'NONE',  ( 785.3141322388236176, -213.7255117493289731, 364.4286716492789537 ) ) ;
#21869 = CARTESIAN_POINT ( 'NONE',  ( 795.8262568251477660, -454.3726999360611103, 308.3538107759623585 ) ) ;
#21870 = CARTESIAN_POINT ( 'NONE',  ( 788.7631598425961101, -409.4419599262317320, -305.7194118038759143 ) ) ;
#21871 = CARTESIAN_POINT ( 'NONE',  ( 767.6429770376289525, -417.1800572038736163, -306.8695393053162093 ) ) ;
#21872 = LINE ( 'NONE', #40777, #15884 ) ;
#21873 = CARTESIAN_POINT ( 'NONE',  ( 815.0009284576459549, -30.35105083532391390, 338.7629533639073429 ) ) ;
#21874 = ORIENTED_EDGE ( 'NONE', *, *, #8301, .F. ) ;
#21875 = CARTESIAN_POINT ( 'NONE',  ( 786.6156483768007774, -193.4419599262325278, -315.5913626894246136 ) ) ;
#21876 = CARTESIAN_POINT ( 'NONE',  ( 803.6646147819161570, -41.90732993114767169, 348.8264449731210561 ) ) ;
#21877 = CARTESIAN_POINT ( 'NONE',  ( 813.9316612368132837, -175.4419599262325562, -348.6739635108323228 ) ) ;
#21878 =( NAMED_UNIT ( * ) SI_UNIT ( $, .STERADIAN. ) SOLID_ANGLE_UNIT ( ) );
#21879 = CARTESIAN_POINT ( 'NONE',  ( 813.2346286133761168, -317.2601417444139429, 328.9521613784389160 ) ) ;
#21880 = CARTESIAN_POINT ( 'NONE',  ( 778.1981804954715471, -154.2709662947836762, 314.8072714833591021 ) ) ;
#21881 = ORIENTED_EDGE ( 'NONE', *, *, #27795, .T. ) ;
#21882 = VECTOR ( 'NONE', #31828, 1000.000000000000114 ) ;
#21883 = EDGE_CURVE ( 'NONE', #39622, #15578, #29927, .T. ) ;
#21884 = CARTESIAN_POINT ( 'NONE',  ( 804.9363028652555840, -328.2709662947831362, 338.2165204200192079 ) ) ;
#21885 = AXIS2_PLACEMENT_3D ( 'NONE', #35633, #308, #22621 ) ;
#21886 = EDGE_CURVE ( 'NONE', #7811, #20516, #19761, .T. ) ;
#21887 = CARTESIAN_POINT ( 'NONE',  ( 814.5518280994195948, -39.72551174932951312, -332.4837098697145734 ) ) ;
#21888 = VECTOR ( 'NONE', #37571, 1000.000000000000000 ) ;
#21889 = CARTESIAN_POINT ( 'NONE',  ( 777.5031285880264704, -94.81642084023843609, 374.9108240113588408 ) ) ;
#21890 = EDGE_LOOP ( 'NONE', ( #2042, #42325, #31254, #21673, #5681, #7976, #10460, #10950, #40637, #21379, #19612, #9152, #22102, #21135, #7865 ) ) ;
#21891 = CARTESIAN_POINT ( 'NONE',  ( 745.1792804349281596, -446.1908817542429802, -343.7566961878542884 ) ) ;
#21892 = VECTOR ( 'NONE', #4468, 1000.000000000000000 ) ;
#21893 = ORIENTED_EDGE ( 'NONE', *, *, #4624, .F. ) ;
#21894 = APPLICATION_PROTOCOL_DEFINITION ( 'draft international standard', 'automotive_design', 1998, #38789 ) ;
#21896 = CARTESIAN_POINT ( 'NONE',  ( 805.2837595273609850, -386.7363362996977116, 340.5290396650784714 ) ) ;
#21895 = CARTESIAN_POINT ( 'NONE',  ( 781.8018195045266339, -46.27096629478404566, 365.1927285166406705 ) ) ;
#21897 = EDGE_CURVE ( 'NONE', #26734, #33702, #16293, .T. ) ;
#21898 = AXIS2_PLACEMENT_3D ( 'NONE', #31092, #6398, #45191 ) ;
#21900 = CARTESIAN_POINT ( 'NONE',  ( 752.4576283171824116, -285.0783235625958127, 317.7880784355627952 ) ) ;
#21899 = CARTESIAN_POINT ( 'NONE',  ( 814.5518280994195948, -399.7255117493283478, 332.4837098697145166 ) ) ;
#21901 = ADVANCED_FACE ( 'NONE', ( #12824 ), #26905, .F. ) ;
#21902 = CARTESIAN_POINT ( 'NONE',  ( 813.9316612368132837, -55.44195992623293989, 348.6739635108323228 ) ) ;
#21903 = CARTESIAN_POINT ( 'NONE',  ( 755.8894580844503253, -279.8272453906071746, -332.3691319403863531 ) ) ;
#21904 = CARTESIAN_POINT ( 'NONE',  ( 785.3141322388236176, -285.7255117493286889, -364.4286716492789537 ) ) ;
#21905 = CARTESIAN_POINT ( 'NONE',  ( 797.6776695296629214, -115.5436935675110988, -357.6776695296636603 ) ) ;
#21906 = DIRECTION ( 'NONE',  ( -1.000000000000000000, -0.000000000000000000, 0.000000000000000000 ) ) ;
#21907 = ORIENTED_EDGE ( 'NONE', *, *, #2430, .F. ) ;
#21908 = CARTESIAN_POINT ( 'NONE',  ( 787.4397851343537695, -381.7255117493284615, 374.2001403089903988 ) ) ;
#21910 = DIRECTION ( 'NONE',  ( 0.000000000000000000, 0.000000000000000000, 1.000000000000000000 ) ) ;
#21909 = LINE ( 'NONE', #25813, #24079 ) ;
#21911 = CARTESIAN_POINT ( 'NONE',  ( 745.7194118038753459, -85.64542720878952764, -348.7631598425976449 ) ) ;
#21912 = LINE ( 'NONE', #4579, #42561 ) ;
#21913 = DIRECTION ( 'NONE',  ( 0.000000000000000000, 1.000000000000000000, 0.000000000000000000 ) ) ;
#21914 = CARTESIAN_POINT ( 'NONE',  ( 759.0159684113467620, -256.9181544815163534, 325.8855110935213020 ) ) ;
#21915 = CARTESIAN_POINT ( 'NONE',  ( 791.9812246680005501, -164.6346026584200217, 361.9419747391813189 ) ) ;
#21916 = VERTEX_POINT ( 'NONE', #24570 ) ;
#21917 = CARTESIAN_POINT ( 'NONE',  ( 796.9462024416508257, -108.4527844766020053, -308.9653473494370246 ) ) ;
#21918 = CARTESIAN_POINT ( 'NONE',  ( 786.6156483768007774, -313.4419599262320730, 315.5913626894246136 ) ) ;
#21919 = CIRCLE ( 'NONE', #33706, 8.024999999999948841 ) ;
#21920 = DIRECTION ( 'NONE',  ( 1.000000000000000000, 0.000000000000000000, 0.000000000000000000 ) ) ;
#21921 = CARTESIAN_POINT ( 'NONE',  ( 745.5313806188320314, -39.28179084515331709, 333.7943932421247268 ) ) ;
#21922 = ADVANCED_FACE ( 'NONE', ( #41701 ), #16761, .T. ) ;
#21924 = CIRCLE ( 'NONE', #40363, 2.749999999999919176 ) ;
#21923 = CARTESIAN_POINT ( 'NONE',  ( 745.7998596910086917, -245.3618753856925139, -332.5602148656461168 ) ) ;
#21925 = CARTESIAN_POINT ( 'NONE',  ( 810.7187646348534145, -210.4527844766016926, 356.7737145352016341 ) ) ;
#21926 = CARTESIAN_POINT ( 'NONE',  ( 754.8072714833581358, -124.8164208402383508, 338.1981804954720587 ) ) ;
#21927 = CARTESIAN_POINT ( 'NONE',  ( -775.4999999999993179, -365.3551492539851893, -8.132432514707076621 ) ) ;
#21928 = CARTESIAN_POINT ( 'NONE',  ( 791.1614460488616487, -299.2601417444139997, -373.5763878283158874 ) ) ;
#21929 = CIRCLE ( 'NONE', #7191, 7.999999999999896083 ) ;
#21930 = CARTESIAN_POINT ( 'NONE',  ( 760.0363995740630116, -442.9181544815157849, 368.7758568127991907 ) ) ;
#21931 = CARTESIAN_POINT ( 'NONE',  ( 772.5602148656447525, -321.7255117493286320, -305.7998596910095443 ) ) ;
#21932 = CARTESIAN_POINT ( 'NONE',  ( -775.4999999999993179, -512.9681489794448908, -339.9999999999999432 ) ) ;
#21933 = CARTESIAN_POINT ( 'NONE',  ( 769.1273215169530886, -406.7146871989590409, 317.4527132478988847 ) ) ;
#21934 = EDGE_LOOP ( 'NONE', ( #9569, #44604, #10445, #40787 ) ) ;
#21935 = DIRECTION ( 'NONE',  ( -0.000000000000000000, 1.000000000000000000, -0.000000000000000000 ) ) ;
#21936 = CARTESIAN_POINT ( 'NONE',  ( 800.2193346964447755, -426.9982390220554862, -355.1360043628815788 ) ) ;
#21937 = AXIS2_PLACEMENT_3D ( 'NONE', #43091, #4072, #39653 ) ;
#21938 = CARTESIAN_POINT ( 'NONE',  ( 799.4546378042377910, -57.07832356259658013, 356.1575198192848006 ) ) ;
#21939 = CARTESIAN_POINT ( 'NONE',  ( 764.3348316497523456, -70.71468719896014932, -308.6759233522265617 ) ) ;
#21940 = CARTESIAN_POINT ( 'NONE',  ( 815.1787889125755555, -198.8965053807779384, 343.7953271457877804 ) ) ;
#21941 = CARTESIAN_POINT ( 'NONE',  ( 803.4237431249931660, -39.18005720387496638, 331.2633955100225194 ) ) ;
#21942 = EDGE_CURVE ( 'NONE', #2273, #3542, #10056, .T. ) ;
#21943 = ORIENTED_EDGE ( 'NONE', *, *, #22712, .T. ) ;
#21944 = CARTESIAN_POINT ( 'NONE',  ( 799.4546378042377910, -249.0783235625959549, -356.1575198192848006 ) ) ;
#21945 = CARTESIAN_POINT ( 'NONE',  ( 755.3201227861273992, -243.7255117493287742, 345.3687786644892981 ) ) ;
#21946 = ADVANCED_FACE ( 'NONE', ( #31529 ), #13067, .T. ) ;
#21947 = CARTESIAN_POINT ( 'NONE',  ( 766.5853460496234675, -37.98741447168752927, -372.3518521366060554 ) ) ;
#21948 = CARTESIAN_POINT ( 'NONE',  ( 804.6798772138710092, -351.7255117493284615, 334.6312213355106451 ) ) ;
#21949 = CARTESIAN_POINT ( 'NONE',  ( 807.9206849184947714, -452.9681489794447202, -338.7201299304387021 ) ) ;
#21950 = ORIENTED_EDGE ( 'NONE', *, *, #5210, .F. ) ;
#21951 = CARTESIAN_POINT ( 'NONE',  ( 787.6308680596127942, -35.26014174441480264, 364.1105419155492768 ) ) ;
#21952 = CARTESIAN_POINT ( 'NONE',  ( 745.1792804349281596, -326.1908817542433781, -343.7566961878542884 ) ) ;
#21953 = CARTESIAN_POINT ( 'NONE',  ( 800.9747183278959710, -276.9982390220559978, 311.9810565676471583 ) ) ;
#21954 = CARTESIAN_POINT ( 'NONE',  ( 756.1443688327750579, 2.376221891948710585, 314.3581564841659315 ) ) ;
#21955 = CARTESIAN_POINT ( 'NONE',  ( 796.9571628226829034, -191.4636090269709996, -321.2382568024804641 ) ) ;
#21956 = CARTESIAN_POINT ( 'NONE',  ( 774.6312213355099630, -191.3618753856925991, -364.6798772138717482 ) ) ;
#21957 = CARTESIAN_POINT ( 'NONE',  ( 788.7366044899766848, -347.9073299311467053, -316.5762568750059813 ) ) ;
#21958 = ORIENTED_EDGE ( 'NONE', *, *, #44243, .T. ) ;
#21959 = CARTESIAN_POINT ( 'NONE',  ( 793.2243759319678702, 21.46713098285774279, -318.4439275373583200 ) ) ;
#21960 = ORIENTED_EDGE ( 'NONE', *, *, #27442, .F. ) ;
#21961 = CIRCLE ( 'NONE', #16784, 9.999999999999982236 ) ;
#21962 = CARTESIAN_POINT ( 'NONE',  ( 811.0346526505616112, -278.6346026584196807, 323.0537975583477532 ) ) ;
#21963 = DIRECTION ( 'NONE',  ( -1.000000000000000000, -0.000000000000000000, -0.000000000000000000 ) ) ;
#21964 = DIRECTION ( 'NONE',  ( 1.000000000000000000, 0.000000000000000000, 0.000000000000000000 ) ) ;
#21965 = CARTESIAN_POINT ( 'NONE',  ( 790.9844846989617508, -142.3726999360620766, 317.2208543904092721 ) ) ;
#21966 = CARTESIAN_POINT ( 'NONE',  ( 788.8264449731200330, -45.18005720387493085, 363.6646147819171233 ) ) ;
#21967 = ORIENTED_EDGE ( 'NONE', *, *, #15575, .T. ) ;
#21968 = CARTESIAN_POINT ( 'NONE',  ( 799.9636004259356241, -406.9181544815157849, -311.2241431872006956 ) ) ;
#21969 = CARTESIAN_POINT ( 'NONE',  ( 763.2262854647970016, -8.634602658420517329, -309.2812353651462445 ) ) ;
#21970 = CARTESIAN_POINT ( 'NONE',  ( 815.3608509340175488, -266.7363362996981095, 341.2497674668889545 ) ) ;
#21971 = CARTESIAN_POINT ( 'NONE',  ( 756.7813123517142913, -235.9874144716868898, 329.9779781133712504 ) ) ;
#21972 = CARTESIAN_POINT ( 'NONE',  ( 781.7834795799800531, -370.8164208402375834, -315.0636971347436202 ) ) ;
#21973 = CARTESIAN_POINT ( 'NONE',  ( -180.7583438952258348, 394.6698570112193920, -274.9999999999999432 ) ) ;
#21974 = CARTESIAN_POINT ( 'NONE',  ( 756.5762568750052424, -3.180057203875080063, 348.7366044899774238 ) ) ;
#21975 = CARTESIAN_POINT ( 'NONE',  ( 773.4516893846965786, -259.6454272087890445, -315.8398074228977066 ) ) ;
#21976 = CARTESIAN_POINT ( 'NONE',  ( 754.9967657858570647, -49.54369356751129061, 365.0032342141425374 ) ) ;
#21977 = CARTESIAN_POINT ( 'NONE',  ( 811.0346526505616112, -110.6346026584201638, 323.0537975583477532 ) ) ;
#21978 = CARTESIAN_POINT ( 'NONE',  ( 999.9999999999992042, 239.9999999999998863, 360.0000000000000000 ) ) ;
#21979 = CARTESIAN_POINT ( 'NONE',  ( 745.1792804349281596, -398.1908817542431507, 343.7566961878542884 ) ) ;
#21980 = DIRECTION ( 'NONE',  ( 0.000000000000000000, 0.000000000000000000, 1.000000000000000000 ) ) ;
#21981 = CARTESIAN_POINT ( 'NONE',  ( 777.4774526936600978, -322.2709662947830225, 304.7301800767027657 ) ) ;
#21982 = CARTESIAN_POINT ( 'NONE',  ( 781.8018195045266339, -334.2709662947829656, -365.1927285166406705 ) ) ;
#21983 = DIRECTION ( 'NONE',  ( 0.000000000000000000, 0.000000000000000000, 1.000000000000000000 ) ) ;
#21984 = CARTESIAN_POINT ( 'NONE',  ( 804.9363028652555840, -424.2709662947829088, 338.2165204200192079 ) ) ;
#21985 = CARTESIAN_POINT ( 'NONE',  ( 790.0220218866281812, -199.0999726633346825, 363.2186876482849129 ) ) ;
#21986 = CARTESIAN_POINT ( 'NONE',  ( 750.9282345327678740, -64.91815448151686496, -319.8311093483690115 ) ) ;
#21987 = CARTESIAN_POINT ( 'NONE',  ( 804.9511171171677688, -125.8055962898690581, -335.8780910478229202 ) ) ;
#21988 = CARTESIAN_POINT ( 'NONE',  ( 751.2241431872005251, -112.1692326535054889, 359.9636004259367610 ) ) ;
#21989 = CARTESIAN_POINT ( 'NONE',  ( 804.9363028652555840, -448.2709662947827951, 338.2165204200192079 ) ) ;
#21990 = CONICAL_SURFACE ( 'NONE', #27129, 8.024999999999948841, 0.7853981633963380560 ) ;
#21991 = CARTESIAN_POINT ( 'NONE',  ( 797.6776695296629214, -451.5436935675099903, 357.6776695296636603 ) ) ;
#21993 = ORIENTED_EDGE ( 'NONE', *, *, #26982, .T. ) ;
#21992 = CARTESIAN_POINT ( 'NONE',  ( 756.7813123517142913, -139.9874144716872024, -329.9779781133712504 ) ) ;
#21994 = CARTESIAN_POINT ( 'NONE',  ( 797.8594530101008786, -109.5436935675110988, -322.1405469898980982 ) ) ;
#21995 = CARTESIAN_POINT ( 'NONE',  ( 779.4709603349208464, -384.3510508353227806, -314.7162404726379918 ) ) ;
#21997 = CARTESIAN_POINT ( 'NONE',  ( 805.1927285166399315, -232.8164208402379529, 341.8018195045277707 ) ) ;
#21996 = CARTESIAN_POINT ( 'NONE',  ( 804.9363028652555840, -280.2709662947833067, 338.2165204200192079 ) ) ;
#21998 = DIRECTION ( 'NONE',  ( 0.000000000000000000, 0.000000000000000000, 1.000000000000000000 ) ) ;
#21999 = ORIENTED_EDGE ( 'NONE', *, *, #18455, .T. ) ;
#22000 = CARTESIAN_POINT ( 'NONE',  ( 792.1044303154645831, -420.4527844766009252, 317.8323909638837677 ) ) ;
#22001 = VERTEX_POINT ( 'NONE', #45394 ) ;
#22002 = CARTESIAN_POINT ( 'NONE',  ( 748.9653473494365699, -194.6346026584199080, 356.9462024416520762 ) ) ;
#22003 = CARTESIAN_POINT ( 'NONE',  ( 786.5483106153019435, -271.6454272087889876, 364.1601925771022366 ) ) ;
#22004 = ORIENTED_EDGE ( 'NONE', *, *, #23244, .F. ) ;
#22005 = CARTESIAN_POINT ( 'NONE',  ( 784.1219089521767955, -69.28179084515321051, -315.0488828828318333 ) ) ;
#22006 = CARTESIAN_POINT ( 'NONE',  ( 764.3348316497523456, -214.7146871989597230, 308.6759233522265617 ) ) ;
#22007 = CARTESIAN_POINT ( 'NONE',  ( 781.8018195045267476, -238.2709662947833920, -365.1927285166407273 ) ) ;
#22008 = VERTEX_POINT ( 'NONE', #24126 ) ;
#22009 = CARTESIAN_POINT ( 'NONE',  ( 755.0636971347428243, -388.2709662947829656, -341.7834795799807353 ) ) ;
#22010 = CARTESIAN_POINT ( 'NONE',  ( 764.8639956371174549, -56.08914811296580893, -319.7806653035542013 ) ) ;
#22011 = CARTESIAN_POINT ( 'NONE',  ( 756.1348686366196716, -257.2601417444141134, 347.5531968255698416 ) ) ;
#22012 = PLANE ( 'NONE',  #36582 ) ;
#22013 = LINE ( 'NONE', #21546, #27066 ) ;
#22014 = CARTESIAN_POINT ( 'NONE',  ( 765.0180583372156207, -0.9982390220569063999, -360.0135310231089534 ) ) ;
#22015 = CARTESIAN_POINT ( 'NONE',  ( 999.9999999999992042, -600.0000000000001137, -360.0000000000000000 ) ) ;
#22016 = VERTEX_POINT ( 'NONE', #31061 ) ;
#22017 = CARTESIAN_POINT ( 'NONE',  ( 757.7880784355613741, -306.0090635724252479, -312.4576283171834916 ) ) ;
#22018 = CARTESIAN_POINT ( 'NONE',  ( 797.8822607201568644, -174.5545181178801784, 370.1134526219340160 ) ) ;
#22019 = VECTOR ( 'NONE', #10628, 1000.000000000000000 ) ;
#22021 = CARTESIAN_POINT ( 'NONE',  ( 797.8594530101008786, -253.5436935675104735, -322.1405469898980982 ) ) ;
#22020 = CARTESIAN_POINT ( 'NONE',  ( -773.4999999999993179, 26.27639943461401018, 900.0000000000001137 ) ) ;
#22022 = DIRECTION ( 'NONE',  ( 0.000000000000000000, 0.000000000000000000, 1.000000000000000000 ) ) ;
#22023 = CARTESIAN_POINT ( 'NONE',  ( 780.5236548040995785, -164.7363362996983938, -314.9735926884559944 ) ) ;
#22024 = CARTESIAN_POINT ( 'NONE',  ( 772.4837098697144029, -23.36187538569318889, 374.5518280994205611 ) ) ;
#22025 = CARTESIAN_POINT ( 'NONE',  ( 784.4999999999993179, -365.3551492539851893, -18.13243251470705886 ) ) ;
#22026 = CARTESIAN_POINT ( 'NONE',  ( 749.8865473780648472, -20.53286901714212931, -322.1177392798429082 ) ) ;
#22027 = CARTESIAN_POINT ( 'NONE',  ( 814.5518280994195948, -351.7255117493284615, -332.4837098697145166 ) ) ;
#22028 = CARTESIAN_POINT ( 'NONE',  ( -78.83651009197140525, 260.0000000000000568, -197.2499999999937756 ) ) ;
#22029 = CARTESIAN_POINT ( 'NONE',  ( 762.3223304703356007, -7.543693567511430942, 322.3223304703362828 ) ) ;
#22030 = CARTESIAN_POINT ( 'NONE',  ( 810.4231160770870019, -288.5545181178798657, 321.9338519418446936 ) ) ;
#22031 = CARTESIAN_POINT ( 'NONE',  ( 778.7502325331095108, -240.3510508353232069, -304.6391490659818828 ) ) ;
#22032 = CARTESIAN_POINT ( 'NONE',  ( 763.0537975583475827, -216.4527844766016926, 371.0346526505627480 ) ) ;
#22033 = CARTESIAN_POINT ( 'NONE',  ( 764.3348316497523456, -430.7146871989590409, -308.6759233522265617 ) ) ;
#22034 = CARTESIAN_POINT ( 'NONE',  ( 779.9999999999992042, 16.45630643248849267, -339.9999999999999432 ) ) ;
#22035 = ORIENTED_EDGE ( 'NONE', *, *, #22712, .F. ) ;
#22036 = CARTESIAN_POINT ( 'NONE',  ( 781.8018195045266339, -334.2709662947829656, 365.1927285166406705 ) ) ;
#22037 = CARTESIAN_POINT ( 'NONE',  ( 804.8461984189677878, -98.19088175424404596, 336.9566956441385628 ) ) ;
#22038 = CARTESIAN_POINT ( 'NONE',  ( 786.6156483768007774, 22.55804007376682918, -315.5913626894246136 ) ) ;
#22039 = CARTESIAN_POINT ( 'NONE',  ( 989.9999999999992042, 249.9999999999998863, 360.0000000000000000 ) ) ;
#22040 = CARTESIAN_POINT ( 'NONE',  ( -784.4999999999993179, -544.8427095258973623, -369.9999999999999432 ) ) ;
#22042 = CARTESIAN_POINT ( 'NONE',  ( 804.9363028652555840, -376.2709662947829656, 338.2165204200192079 ) ) ;
#22041 = CARTESIAN_POINT ( 'NONE',  ( 793.2243759319678702, -146.5328690171417350, 318.4439275373583200 ) ) ;
#22043 = ORIENTED_EDGE ( 'NONE', *, *, #40217, .T. ) ;
#22044 = CARTESIAN_POINT ( 'NONE',  ( 793.2243759319678702, -290.5328690171412518, -318.4439275373583200 ) ) ;
#22045 = CARTESIAN_POINT ( 'NONE',  ( 756.3353852180819104, -173.9073299311472169, 331.1735550268788302 ) ) ;
#22046 = EDGE_CURVE ( 'NONE', #22721, #2036, #37987, .T. ) ;
#22047 = CARTESIAN_POINT ( 'NONE',  ( 801.9858362298568863, -339.0783235625956422, -312.7379699480935642 ) ) ;
#22048 = FACE_BOUND ( 'NONE', #35186, .T. ) ;
#22049 = CARTESIAN_POINT ( 'NONE',  ( 782.4968714119720516, 13.18357915976123174, 305.0891759886411023 ) ) ;
#22050 = ORIENTED_EDGE ( 'NONE', *, *, #24651, .F. ) ;
#22051 = CARTESIAN_POINT ( 'NONE',  ( 755.5713283507202505, -317.3618753856922581, 334.6858677611754729 ) ) ;
#22052 = CIRCLE ( 'NONE', #22766, 2.749999999999863665 ) ;
#22053 = CARTESIAN_POINT ( 'NONE',  ( 757.2208543904082489, -88.71468719896009247, -350.9844846989624330 ) ) ;
#22054 = CARTESIAN_POINT ( 'NONE',  ( 801.9419747391806368, -450.4527844766009821, 351.9812246680014027 ) ) ;
#22055 = CARTESIAN_POINT ( 'NONE',  ( 754.9967657858570647, -145.5436935675109851, -365.0032342141425374 ) ) ;
#22056 = EDGE_LOOP ( 'NONE', ( #28594, #29289 ) ) ;
#22057 = CARTESIAN_POINT ( 'NONE',  ( 762.3223304703356007, -127.5436935675110561, -322.3223304703362828 ) ) ;
#22058 = EDGE_LOOP ( 'NONE', ( #16856, #45118, #43573, #30329 ) ) ;
#22059 = CARTESIAN_POINT ( 'NONE',  ( 776.9254006560222479, -428.1908817542430938, -314.8983024940802125 ) ) ;
#22060 = CARTESIAN_POINT ( 'NONE',  ( 803.6646147819161570, 6.092670068852159559, 348.8264449731210561 ) ) ;
#22061 = CARTESIAN_POINT ( 'NONE',  ( 802.7791456095903868, -148.7146871989598935, 329.0155153010375102 ) ) ;
#22064 = CARTESIAN_POINT ( 'NONE',  ( 751.2241431872005251, -400.1692326535045936, 359.9636004259367610 ) ) ;
#22063 = DIRECTION ( 'NONE',  ( 0.000000000000000000, 1.000000000000000000, 0.000000000000000000 ) ) ;
#22062 = FACE_OUTER_BOUND ( 'NONE', #26478, .T. ) ;
#22065 = ORIENTED_EDGE ( 'NONE', *, *, #14268, .T. ) ;
#22066 = ADVANCED_FACE ( 'NONE', ( #41465, #16984 ), #23885, .T. ) ;
#22067 = CARTESIAN_POINT ( 'NONE',  ( 790.9844846989617508, -406.3726999360612808, -317.2208543904092721 ) ) ;
#22068 = FACE_OUTER_BOUND ( 'NONE', #38837, .T. ) ;
#22069 = CARTESIAN_POINT ( 'NONE',  ( 810.4231160770870019, -216.5545181178800931, -321.9338519418446936 ) ) ;
#22070 = CARTESIAN_POINT ( 'NONE',  ( 749.5768839229115201, -84.55451811788046257, 358.0661480581553064 ) ) ;
#22072 = DIRECTION ( 'NONE',  ( -0.000000000000000000, -0.000000000000000000, 1.000000000000000000 ) ) ;
#22071 = CARTESIAN_POINT ( 'NONE',  ( -208.8365100919714052, 260.0000000000001137, -199.9999999999926956 ) ) ;
#22073 = CARTESIAN_POINT ( 'NONE',  ( 760.5453621957607311, -333.0783235625956991, -323.8424801807151425 ) ) ;
#22074 = CARTESIAN_POINT ( 'NONE',  ( 789.9999999999992042, 240.0000000000000853, -360.0000000000000000 ) ) ;
#22075 = CARTESIAN_POINT ( 'NONE',  ( 815.3608509340175488, -194.7363362996982517, -341.2497674668889545 ) ) ;
#22076 = CARTESIAN_POINT ( 'NONE',  ( 794.9999999999993179, 197.3292319334027241, -273.4704985657796783 ) ) ;
#22077 = FACE_BOUND ( 'NONE', #30290, .T. ) ;
#22078 = CARTESIAN_POINT ( 'NONE',  ( 799.2566176426618085, -408.0090635724249069, 324.0069404352559559 ) ) ;
#22079 = CIRCLE ( 'NONE', #4029, 7.999999999999785061 ) ;
#22080 = CARTESIAN_POINT ( 'NONE',  ( 804.7487373415286811, -235.5436935675107293, -364.7487373415288516 ) ) ;
#22081 = CARTESIAN_POINT ( 'NONE',  ( 571.1634899080285095, 259.9999999999999432, -199.9999999999981526 ) ) ;
#22082 = CARTESIAN_POINT ( 'NONE',  ( 805.1927285166397041, -16.81642084023866701, -341.8018195045277707 ) ) ;
#22083 = AXIS2_PLACEMENT_3D ( 'NONE', #44117, #44821, #2080 ) ;
#22084 = CARTESIAN_POINT ( 'NONE',  ( 760.0363995740630116, -178.9181544815165239, 368.7758568127991907 ) ) ;
#22085 = CARTESIAN_POINT ( 'NONE',  ( 758.0141637701419768, -87.07832356259646645, -367.2620300519063790 ) ) ;
#22086 = CARTESIAN_POINT ( 'NONE',  ( 782.4968714119720516, -130.8164208402383224, 305.0891759886411023 ) ) ;
#22087 = CARTESIAN_POINT ( 'NONE',  ( 746.8695393053150156, -389.9073299311465348, -327.6429770376306010 ) ) ;
#22088 = LINE ( 'NONE', #3859, #29830 ) ;
#22089 = DIRECTION ( 'NONE',  ( 0.7071067811865753283, 0.000000000000000000, -0.7071067811865198172 ) ) ;
#22090 = CARTESIAN_POINT ( 'NONE',  ( 781.8018195045266339, -214.2709662947834488, 365.1927285166406705 ) ) ;
#22091 = CARTESIAN_POINT ( 'NONE',  ( 746.4236121716829757, -447.8272453906067199, 328.8385539511384650 ) ) ;
#22092 = CARTESIAN_POINT ( 'NONE',  ( 754.0944755984390895, -423.6237781080499190, -364.1009440267246760 ) ) ;
#22093 = CARTESIAN_POINT ( 'NONE',  ( 813.5763878283155464, -3.827245390607979303, -351.1614460488615350 ) ) ;
#22094 = LINE ( 'NONE', #4767, #21056 ) ;
#22095 = CARTESIAN_POINT ( 'NONE',  ( 800.1688906516307043, -34.16923265350572336, 369.0717654672308186 ) ) ;
#22096 = ADVANCED_FACE ( 'NONE', ( #28051 ), #2893, .F. ) ;
#22097 = CARTESIAN_POINT ( 'NONE',  ( 758.6633372737375112, -188.5328690171416497, -326.9102291470432533 ) ) ;
#22098 = CARTESIAN_POINT ( 'NONE',  ( 785.3141322388236176, -21.72551174932956641, 364.4286716492789537 ) ) ;
#22099 = CARTESIAN_POINT ( 'NONE',  ( 814.8230680027162407, -173.8055962898689302, -333.7305795820267917 ) ) ;
#22100 = CARTESIAN_POINT ( 'NONE',  ( 793.4146539503750546, -337.9874144716865771, 307.6481478633938877 ) ) ;
#22101 = CARTESIAN_POINT ( 'NONE',  ( 802.1676090361155502, -158.6346026584200217, 327.8955696845344505 ) ) ;
#22102 = ORIENTED_EDGE ( 'NONE', *, *, #35748, .F. ) ;
#22103 = CARTESIAN_POINT ( 'NONE',  ( 754.0944755984390895, -423.6237781080499190, 364.1009440267246760 ) ) ;
#22104 = CARTESIAN_POINT ( 'NONE',  ( 764.8639956371174549, -152.0891481129655460, -319.7806653035542013 ) ) ;
#22105 = CARTESIAN_POINT ( 'NONE',  ( 785.3687786644884454, -347.3618753856922012, 315.3201227861279676 ) ) ;
#22106 = CARTESIAN_POINT ( 'NONE',  ( 751.9810565676468741, -26.08914811296592262, -360.9747183278973921 ) ) ;
#22107 = ORIENTED_EDGE ( 'NONE', *, *, #20475, .F. ) ;
#22108 = CARTESIAN_POINT ( 'NONE',  ( 750.9282345327678740, -448.9181544815156144, -319.8311093483690115 ) ) ;
#22109 = VERTEX_POINT ( 'NONE', #6362 ) ;
#22110 = CARTESIAN_POINT ( 'NONE',  ( 784.1219089521767955, -309.2817908451525568, -315.0488828828318333 ) ) ;
#22112 = CARTESIAN_POINT ( 'NONE',  ( 772.4468031744293057, -369.8272453906068904, 363.8651313633793620 ) ) ;
#22111 = CARTESIAN_POINT ( 'NONE',  ( 803.4237431249931660, -63.18005720387488822, 331.2633955100225194 ) ) ;
#22113 = CARTESIAN_POINT ( 'NONE',  ( 801.9419747391806368, -306.4527844766013800, -351.9812246680014027 ) ) ;
#22115 = CARTESIAN_POINT ( 'NONE',  ( 746.7653713866222915, -281.2601417444139997, 351.0478386215610271 ) ) ;
#22114 = CARTESIAN_POINT ( 'NONE',  ( 767.7687537140311633, -407.9073299311465348, 372.7932403749916830 ) ) ;
#22116 = CARTESIAN_POINT ( 'NONE',  ( 811.6461892240364477, -100.7146871989600356, 324.1737431748509835 ) ) ;
#22117 = CARTESIAN_POINT ( 'NONE',  ( 776.9254006560222479, -284.1908817542434917, -314.8983024940802125 ) ) ;
#22118 = CARTESIAN_POINT ( 'NONE',  ( 755.3201227861273992, -291.7255117493285752, -345.3687786644892981 ) ) ;
#22119 = DIRECTION ( 'NONE',  ( 1.000000000000000000, -1.880165489482579047E-16, 0.000000000000000000 ) ) ;
#22120 = CARTESIAN_POINT ( 'NONE',  ( 804.4286716492782716, -161.3618753856927697, -345.3141322388244703 ) ) ;
#22121 = CARTESIAN_POINT ( 'NONE',  ( 794.9999999999993179, 205.0000000000000568, 255.0000000000000000 ) ) ;
#22122 = VERTEX_POINT ( 'NONE', #6582 ) ;
#22123 = CARTESIAN_POINT ( 'NONE',  ( 814.5518280994195948, -423.7255117493281205, 332.4837098697145734 ) ) ;
#22125 = FACE_OUTER_BOUND ( 'NONE', #26514, .T. ) ;
#22124 = CARTESIAN_POINT ( 'NONE',  ( 959.5497976682736407, 120.6654763175833693, -209.9999999999999716 ) ) ;
#22126 = CARTESIAN_POINT ( 'NONE',  ( 748.6759233522253680, -88.37269993606226137, -324.3348316497537098 ) ) ;
#22127 = CARTESIAN_POINT ( 'NONE',  ( 779.9999999999990905, 18.49609980828599376, 309.9999999999999432 ) ) ;
#22128 = FACE_OUTER_BOUND ( 'NONE', #8151, .T. ) ;
#22129 = CARTESIAN_POINT ( 'NONE',  ( 804.1105419155481968, -291.8272453906071746, 347.6308680596136469 ) ) ;
#22130 = CARTESIAN_POINT ( 'NONE',  ( 804.6798772138708955, -159.7255117493291436, 334.6312213355107019 ) ) ;
#22131 = ORIENTED_EDGE ( 'NONE', *, *, #10900, .T. ) ;
#22132 = CARTESIAN_POINT ( 'NONE',  ( 808.0189434323515343, -110.0891481129656597, -319.0252816721025511 ) ) ;
#22133 = CARTESIAN_POINT ( 'NONE',  ( 783.0433043558608688, -312.8965053807775689, 315.1538015810313027 ) ) ;
#22134 = CARTESIAN_POINT ( 'NONE',  ( 441.1634899080286232, 259.9999999999999432, -208.0249999999972488 ) ) ;
#22135 = EDGE_CURVE ( 'NONE', #45115, #2619, #45631, .T. ) ;
#22136 = CARTESIAN_POINT ( 'NONE',  ( 804.1009440267234822, -23.46360902697155026, 314.0944755984392600 ) ) ;
#22137 = CARTESIAN_POINT ( 'NONE',  ( 767.6429770376289525, -249.1800572038742416, -306.8695393053162093 ) ) ;
#22138 = EDGE_CURVE ( 'NONE', #18205, #38597, #41242, .T. ) ;
#22139 = CARTESIAN_POINT ( 'NONE',  ( 774.6858677611749044, -129.7255117493292289, 315.5713283507209894 ) ) ;
#22140 = CARTESIAN_POINT ( 'NONE',  ( 759.9999999999992042, 205.0000000000000568, 360.0000000000000000 ) ) ;
#22141 = CARTESIAN_POINT ( 'NONE',  ( 813.2346286133761168, -317.2601417444139429, -328.9521613784389160 ) ) ;
#22142 = CARTESIAN_POINT ( 'NONE',  ( 793.0897708529556667, -30.55451811788062244, 361.3366627262616362 ) ) ;
#22143 = CARTESIAN_POINT ( 'NONE',  ( 814.2001403089898304, -329.3618753856922581, -347.4397851343538264 ) ) ;
#22144 = DIRECTION ( 'NONE',  ( -0.000000000000000000, -0.000000000000000000, -1.000000000000000000 ) ) ;
#22145 = CARTESIAN_POINT ( 'NONE',  ( 805.0264073115434940, -414.3510508353227237, 339.4763451958999099 ) ) ;
#22146 = ORIENTED_EDGE ( 'NONE', *, *, #28278, .T. ) ;
#22147 = CARTESIAN_POINT ( 'NONE',  ( 762.1405469898971887, -409.5436935675101040, -357.8594530101015607 ) ) ;
#22148 = EDGE_CURVE ( 'NONE', #31022, #25758, #10496, .T. ) ;
#22149 = CARTESIAN_POINT ( 'NONE',  ( 797.6776695296629214, -211.5436935675107861, -357.6776695296636603 ) ) ;
#22150 = CARTESIAN_POINT ( 'NONE',  ( 815.1787889125755555, -78.89650538077832209, -343.7953271457877804 ) ) ;
#22151 = FACE_OUTER_BOUND ( 'NONE', #37669, .T. ) ;
#22152 = CARTESIAN_POINT ( 'NONE',  ( 754.0944755984390895, -231.6237781080504874, 364.1009440267246760 ) ) ;
#22153 = CARTESIAN_POINT ( 'NONE',  ( 797.8594530101009923, -61.54369356751124798, 322.1405469898982119 ) ) ;
#22154 = ORIENTED_EDGE ( 'NONE', *, *, #18208, .F. ) ;
#22155 = CARTESIAN_POINT ( 'NONE',  ( 764.0069404352550464, -231.0783235625960401, -359.2566176426627180 ) ) ;
#22156 = CARTESIAN_POINT ( 'NONE',  ( 781.7834795799800531, -226.8164208402380098, 315.0636971347436202 ) ) ;
#22157 = CARTESIAN_POINT ( 'NONE',  ( 813.9316612368132837, -79.44195992623286884, -348.6739635108323228 ) ) ;
#22158 = CARTESIAN_POINT ( 'NONE',  ( 796.3364271039121149, -452.9681489794448339, -359.1033184105688747 ) ) ;
#22159 = EDGE_CURVE ( 'NONE', #23669, #37975, #27594, .T. ) ;
#22160 = EDGE_LOOP ( 'NONE', ( #15573, #36687, #1354, #8308 ) ) ;
#22161 = CARTESIAN_POINT ( 'NONE',  ( 781.2370466360911223, -332.7363362996979390, -304.9990715423533629 ) ) ;
#22162 = EDGE_CURVE ( 'NONE', #2619, #37165, #45412, .T. ) ;
#22163 = CARTESIAN_POINT ( 'NONE',  ( 751.6929314249750860, -294.9982390220559978, 318.8095938919659034 ) ) ;
#22164 = CARTESIAN_POINT ( 'NONE',  ( 810.1134526219336749, -8.532869017142163059, 357.8822607201570349 ) ) ;
#22165 = CARTESIAN_POINT ( 'NONE',  ( 805.2837595273609850, -170.7363362996983938, -340.5290396650784714 ) ) ;
#22166 = CARTESIAN_POINT ( 'NONE',  ( 767.8955696845333705, -168.4527844766018347, -362.1676090361162323 ) ) ;
#22167 = CARTESIAN_POINT ( 'NONE',  ( 788.7366044899766848, -371.9073299311465917, -316.5762568750059813 ) ) ;
#22168 = ORIENTED_EDGE ( 'NONE', *, *, #11776, .F. ) ;
#22169 = EDGE_LOOP ( 'NONE', ( #1981, #41371, #36354, #7124 ) ) ;
#22170 = CARTESIAN_POINT ( 'NONE',  ( 777.5031285880264704, -310.8164208402377540, 374.9108240113588408 ) ) ;
#22171 = LINE ( 'NONE', #40193, #32183 ) ;
#22172 = CARTESIAN_POINT ( 'NONE',  ( 800.7704444035546203, -364.1692326535046504, 326.0291762391768771 ) ) ;
#22173 = LINE ( 'NONE', #15491, #44524 ) ;
#22174 = CARTESIAN_POINT ( 'NONE',  ( 796.9571628226829034, -191.4636090269709996, 321.2382568024804641 ) ) ;
#22175 = CARTESIAN_POINT ( 'NONE',  ( 792.1044303154645831, -60.45278447660215448, 317.8323909638837677 ) ) ;
#22176 = EDGE_LOOP ( 'NONE', ( #4407, #40305, #37332, #26136 ) ) ;
#22177 = CARTESIAN_POINT ( 'NONE',  ( 811.3240766477731540, -412.3726999360612808, -355.6651683502462902 ) ) ;
#22178 = EDGE_CURVE ( 'NONE', #16297, #32451, #38688, .T. ) ;
#22179 = CARTESIAN_POINT ( 'NONE',  ( 796.7737145352015204, 3.365397341579444479, -370.7187646348536987 ) ) ;
#22180 = CARTESIAN_POINT ( 'NONE',  ( 807.2620300519052989, -264.0090635724253616, 318.0141637701419768 ) ) ;
#22181 = CARTESIAN_POINT ( 'NONE',  ( 763.2154366446407039, -237.6237781080505442, 321.4292242960311228 ) ) ;
#22182 = CARTESIAN_POINT ( 'NONE',  ( 785.3141322388236176, -405.7255117493283478, -364.4286716492789537 ) ) ;
#22183 = CARTESIAN_POINT ( 'NONE',  ( 786.4999999999993179, -513.1383975375929367, -349.9999999999999432 ) ) ;
#22184 = EDGE_CURVE ( 'NONE', #15471, #6074, #9599, .T. ) ;
#22185 = CARTESIAN_POINT ( 'NONE',  ( 801.5560724626406000, -456.5545181178792404, 326.7756240680316182 ) ) ;
#22186 = FACE_OUTER_BOUND ( 'NONE', #10555, .T. ) ;
#22187 = CARTESIAN_POINT ( 'NONE',  ( 799.2566176426618085, -240.0090635724253900, -324.0069404352559559 ) ) ;
#22188 = EDGE_CURVE ( 'NONE', #12298, #10740, #40978, .T. ) ;
#22189 = CARTESIAN_POINT ( 'NONE',  ( 787.4397851343537695, -45.72551174932949181, 374.2001403089903988 ) ) ;
#22190 = CARTESIAN_POINT ( 'NONE',  ( 796.7737145352015204, -116.6346026584201780, 370.7187646348536987 ) ) ;
#22191 = CARTESIAN_POINT ( 'NONE',  ( -37.63011601220122770, -512.9681489794448908, -327.9999999999999432 ) ) ;
#22192 = DIRECTION ( 'NONE',  ( -0.000000000000000000, 1.000000000000000000, 0.000000000000000000 ) ) ;
#22193 = CARTESIAN_POINT ( 'NONE',  ( 745.7194118038753459, -373.6454272087887034, 348.7631598425976449 ) ) ;
#22194 = FACE_OUTER_BOUND ( 'NONE', #34137, .T. ) ;
#22195 = CARTESIAN_POINT ( 'NONE',  ( 749.2812353651451076, -366.4527844766012095, 323.2262854647983090 ) ) ;
#22196 = EDGE_CURVE ( 'NONE', #16704, #33515, #37771, .T. ) ;
#22197 = CARTESIAN_POINT ( 'NONE',  ( 791.9812246680005501, -308.6346026584195670, -361.9419747391813189 ) ) ;
#22198 = PRODUCT_RELATED_PRODUCT_CATEGORY ( 'part', '', ( #21103 ) ) ;
#22199 = CARTESIAN_POINT ( 'NONE',  ( 774.6858677611749044, -417.7255117493283478, 315.5713283507209894 ) ) ;
#22200 = CARTESIAN_POINT ( 'NONE',  ( 766.9102291470427417, -186.5545181178801215, 318.6633372737382501 ) ) ;
#22201 = CARTESIAN_POINT ( 'NONE',  ( 762.1177392798416577, -66.55451811788050520, -309.8865473780659272 ) ) ;
#22202 = CARTESIAN_POINT ( 'NONE',  ( 757.2208543904082489, -136.7146871989600072, -350.9844846989624330 ) ) ;
#22203 = CARTESIAN_POINT ( 'NONE',  ( 778.7502325331095108, -120.3510508353236048, 304.6391490659818828 ) ) ;
#22204 = CARTESIAN_POINT ( 'NONE',  ( 757.8323909638828582, -434.6346026584190554, 352.1044303154654358 ) ) ;
#22205 = CARTESIAN_POINT ( 'NONE',  ( 803.6646147819161570, -41.90732993114767169, -348.8264449731210561 ) ) ;
#22206 = CARTESIAN_POINT ( 'NONE',  ( 773.3843516231979720, -133.4419599262326699, -364.4086373105754433 ) ) ;
#22207 = CARTESIAN_POINT ( 'NONE',  ( 797.8594530101008786, -85.54369356751118403, -322.1405469898980982 ) ) ;
#22208 = CARTESIAN_POINT ( 'NONE',  ( 805.1016975059191054, -438.8965053807771710, -343.0745993439771837 ) ) ;
#22210 = CARTESIAN_POINT ( 'NONE',  ( 754.8072714833583632, -244.8164208402379245, 338.1981804954721156 ) ) ;
#22209 = CARTESIAN_POINT ( 'NONE',  ( 804.6798772138708955, -255.7255117493287742, 334.6312213355107019 ) ) ;
#22211 = FACE_OUTER_BOUND ( 'NONE', #27112, .T. ) ;
#22212 = ORIENTED_EDGE ( 'NONE', *, *, #26992, .T. ) ;
#22213 = CARTESIAN_POINT ( 'NONE',  ( 787.6308680596127942, 12.73985825558503926, 364.1105419155492768 ) ) ;
#22214 = ORIENTED_EDGE ( 'NONE', *, *, #26932, .T. ) ;
#22215 = CARTESIAN_POINT ( 'NONE',  ( 758.8095938919644823, -200.0891481129653471, 311.6929314249762797 ) ) ;
#22216 = CARTESIAN_POINT ( 'NONE',  ( 766.0291762391763086, -274.9181544815161828, 360.7704444035551319 ) ) ;
#22217 = EDGE_LOOP ( 'NONE', ( #43972, #8620, #28755, #5742 ) ) ;
#22218 = CARTESIAN_POINT ( 'NONE',  ( 805.2837595273609850, -74.73633629969866377, -340.5290396650784714 ) ) ;
#22219 = CARTESIAN_POINT ( 'NONE',  ( 744.8212110874229666, -210.8965053807778816, 336.2046728542121627 ) ) ;
#22220 = CARTESIAN_POINT ( 'NONE',  ( 788.8264449731201466, -285.1800572038741279, -363.6646147819170665 ) ) ;
#22221 = ORIENTED_EDGE ( 'NONE', *, *, #1890, .T. ) ;
#22222 = CARTESIAN_POINT ( 'NONE',  ( 771.2633955100217236, -383.9073299311466485, -363.4237431249939618 ) ) ;
#22223 = CARTESIAN_POINT ( 'NONE',  ( 803.4237431249931660, -63.18005720387488822, -331.2633955100225194 ) ) ;
#22224 = CARTESIAN_POINT ( 'NONE',  ( 764.0069404352550464, -255.0783235625958980, 359.2566176426627180 ) ) ;
#22225 = CARTESIAN_POINT ( 'NONE',  ( 51.16348990802859475, 260.0000000000000568, -191.9749999999945089 ) ) ;
#22226 = CARTESIAN_POINT ( 'NONE',  ( 51.16348990802859475, 240.0000000000000568, -202.7499999999943441 ) ) ;
#22227 = CARTESIAN_POINT ( 'NONE',  ( 786.2694204179717872, -21.28179084515337749, -305.1769319972829067 ) ) ;
#22228 = DIRECTION ( 'NONE',  ( -1.000000000000000000, 0.000000000000000000, 0.000000000000000000 ) ) ;
#22229 = EDGE_LOOP ( 'NONE', ( #17177, #41581, #19717, #4408, #25103, #42498, #36927, #13384, #12970, #6093, #29278, #23616 ) ) ;
#22230 = CARTESIAN_POINT ( 'NONE',  ( 773.7305795820266212, -297.2817908451526137, -374.8230680027170365 ) ) ;
#22231 = CARTESIAN_POINT ( 'NONE',  ( 766.4474001241216001, -163.0999726633347677, 307.3154664389482491 ) ) ;
#22233 = CARTESIAN_POINT ( 'NONE',  ( 759.7806653035534055, -246.9982390220560546, -324.8639956371180801 ) ) ;
#22232 = LINE ( 'NONE', #35413, #29795 ) ;
#22234 = DIRECTION ( 'NONE',  ( 0.000000000000000000, 0.000000000000000000, 1.000000000000000000 ) ) ;
#22235 = CARTESIAN_POINT ( 'NONE',  ( 759.0159684113467620, -136.9181544815166376, -325.8855110935213020 ) ) ;
#22236 = MECHANICAL_DESIGN_GEOMETRIC_PRESENTATION_REPRESENTATION (  '', ( #42162 ), #2316 ) ;
#22237 = FACE_BOUND ( 'NONE', #3321, .T. ) ;
#22238 = CARTESIAN_POINT ( 'NONE',  ( 783.7566961878529810, -24.89650538077847486, -305.1792804349288417 ) ) ;
#22239 = CARTESIAN_POINT ( 'NONE',  ( 746.8695393053151292, -341.9073299311466485, -327.6429770376306578 ) ) ;
#22240 = LINE ( 'NONE', #15552, #20936 ) ;
#22241 = CARTESIAN_POINT ( 'NONE',  ( 762.1405469898971887, -1.543693567511449150, 357.8594530101015607 ) ) ;
#22242 = CARTESIAN_POINT ( 'NONE',  ( 776.2046728542105711, -284.1908817542434917, 304.8212110874238761 ) ) ;
#22243 = CARTESIAN_POINT ( 'NONE',  ( 761.9338519418445230, -230.5328690171415076, -370.4231160770881957 ) ) ;
#22244 = CARTESIAN_POINT ( 'NONE',  ( 772.5602148656447525, -273.7255117493288026, 305.7998596910095443 ) ) ;
#22245 = CARTESIAN_POINT ( 'NONE',  ( 773.7943932421234194, -431.8055962898681059, -305.5313806188329409 ) ) ;
#22246 = FACE_BOUND ( 'NONE', #36587, .T. ) ;
#22247 = ORIENTED_EDGE ( 'NONE', *, *, #19948, .T. ) ;
#22248 = CARTESIAN_POINT ( 'NONE',  ( 755.3201227861273992, -339.7255117493285184, 345.3687786644892981 ) ) ;
#22249 = CARTESIAN_POINT ( 'NONE',  ( 786.5483106153019435, -79.64542720878957027, 364.1601925771022366 ) ) ;
#22250 = CARTESIAN_POINT ( 'NONE',  ( 805.0264073115434940, -6.351050835323991173, -339.4763451958999099 ) ) ;
#22251 = LINE ( 'NONE', #24814, #32845 ) ;
#22252 = DIRECTION ( 'NONE',  ( -1.880165489482579047E-16, -1.000000000000000000, -0.000000000000000000 ) ) ;
#22253 = CARTESIAN_POINT ( 'NONE',  ( 815.1787889125755555, -126.8965053807781516, 343.7953271457877804 ) ) ;
#22255 = CARTESIAN_POINT ( 'NONE',  ( 785.3687786644884454, -395.3618753856918602, 315.3201227861279676 ) ) ;
#22254 = CARTESIAN_POINT ( 'NONE',  ( 772.3691319403857278, -143.2601417444144829, 315.8894580844506663 ) ) ;
#22256 = ORIENTED_EDGE ( 'NONE', *, *, #45035, .T. ) ;
#22257 = CARTESIAN_POINT ( 'NONE',  ( 792.1044303154645831, -36.45278447660223975, -317.8323909638837677 ) ) ;
#22258 = CARTESIAN_POINT ( 'NONE',  ( 760.5453621957607311, -309.0783235625957559, -323.8424801807151425 ) ) ;
#22259 = CARTESIAN_POINT ( 'NONE',  ( 757.8323909638827445, -146.6346026584200217, 352.1044303154654358 ) ) ;
#22260 = CARTESIAN_POINT ( 'NONE',  ( 761.9338519418445230, -326.5328690171411381, -370.4231160770881957 ) ) ;
#22261 = PLANE ( 'NONE',  #32282 ) ;
#22262 = CARTESIAN_POINT ( 'NONE',  ( 814.5518280994195948, 8.274488250670337663, 332.4837098697145734 ) ) ;
#22263 = ORIENTED_EDGE ( 'NONE', *, *, #30653, .T. ) ;
#22264 = CARTESIAN_POINT ( 'NONE',  ( 802.1676090361156639, -374.6346026584192828, 327.8955696845344505 ) ) ;
#22265 = CARTESIAN_POINT ( 'NONE',  ( 784.0799538623451781, -83.80559628986920018, -364.6971507214555572 ) ) ;
#22266 = ORIENTED_EDGE ( 'NONE', *, *, #24740, .F. ) ;
#22267 = CARTESIAN_POINT ( 'NONE',  ( 800.2193346964447755, -450.9982390220554294, 355.1360043628815788 ) ) ;
#22268 = CARTESIAN_POINT ( 'NONE',  ( 745.4481719005789273, -195.7255117493289731, -347.5162901302853129 ) ) ;
#22269 = ORIENTED_EDGE ( 'NONE', *, *, #32364, .F. ) ;
#22270 = AXIS2_PLACEMENT_3D ( 'NONE', #33599, #30134, #41223 ) ;
#22271 = CARTESIAN_POINT ( 'NONE',  ( 805.1927285166399315, -184.8164208402381234, -341.8018195045277707 ) ) ;
#22272 = ORIENTED_EDGE ( 'NONE', *, *, #10052, .F. ) ;
#22273 = CARTESIAN_POINT ( 'NONE',  ( 766.9102291470427417, -426.5545181178794678, -318.6633372737382501 ) ) ;
#22274 = CARTESIAN_POINT ( 'NONE',  ( 756.3353852180819104, -5.907329931147798696, 331.1735550268788302 ) ) ;
#22275 = CARTESIAN_POINT ( 'NONE',  ( 792.3570229623688874, -237.1800572038742985, 373.1304606946836202 ) ) ;
#22276 = CARTESIAN_POINT ( 'NONE',  ( 786.6156483768007774, -169.4419599262325562, 315.5913626894246136 ) ) ;
#22279 = CARTESIAN_POINT ( 'NONE',  ( 813.9316612368132837, -415.4419599262318457, 348.6739635108323228 ) ) ;
#22278 = CARTESIAN_POINT ( 'NONE',  ( -598.8365100919716042, 230.0000000000001421, -197.2499999999901092 ) ) ;
#22277 = DIRECTION ( 'NONE',  ( 0.3826814224632300032, 0.000000000000000000, 0.9238803650373347276 ) ) ;
#22280 = ORIENTED_EDGE ( 'NONE', *, *, #34823, .T. ) ;
#22281 = CARTESIAN_POINT ( 'NONE',  ( 800.9840315886518738, -436.9181544815157281, -354.1144889064786412 ) ) ;
#22282 = DIRECTION ( 'NONE',  ( 0.000000000000000000, 0.000000000000000000, 1.000000000000000000 ) ) ;
#22283 = CARTESIAN_POINT ( 'NONE',  ( 814.4686193811664907, -219.2817908451527558, -346.2056067578752732 ) ) ;
#22284 = CARTESIAN_POINT ( 'NONE',  ( 754.3581564841646241, -65.46360902697142592, 316.1443688327762516 ) ) ;
#22286 = LINE ( 'NONE', #1283, #40295 ) ;
#22285 = CARTESIAN_POINT ( 'NONE',  ( -728.8365100919714905, 260.0000000000001705, -199.9999999999890861 ) ) ;
#22287 = CARTESIAN_POINT ( 'NONE',  ( 793.2243759319678702, -338.5328690171411381, -318.4439275373583200 ) ) ;
#22288 = DIRECTION ( 'NONE',  ( 0.000000000000000000, 0.000000000000000000, 1.000000000000000000 ) ) ;
#22289 = CARTESIAN_POINT ( 'NONE',  ( 773.7305795820266212, -201.2817908451528126, -374.8230680027170365 ) ) ;
#22290 = DIRECTION ( 'NONE',  ( -1.000000000000000000, 0.000000000000000000, 0.000000000000000000 ) ) ;
#22291 = DIRECTION ( 'NONE',  ( -1.000000000000000000, -0.000000000000000000, 0.000000000000000000 ) ) ;
#22292 = CARTESIAN_POINT ( 'NONE',  ( 776.9254006560222479, -404.1908817542431507, 314.8983024940802125 ) ) ;
#22293 = CARTESIAN_POINT ( 'NONE',  ( 814.5518280994195948, -255.7255117493287742, -332.4837098697145166 ) ) ;
#22294 = CARTESIAN_POINT ( 'NONE',  ( 755.3028492785439312, -231.2817908451527558, 335.9200461376539693 ) ) ;
#22295 = CARTESIAN_POINT ( 'NONE',  ( 794.9999999999993179, 239.9999999999998863, -235.0000000000000000 ) ) ;
#22296 = CARTESIAN_POINT ( 'NONE',  ( 774.6312213355099630, -23.36187538569318889, -364.6798772138717482 ) ) ;
#22297 = CARTESIAN_POINT ( 'NONE',  ( 764.1737431748507561, -178.3726999360619629, 371.6461892240376415 ) ) ;
#22298 = CARTESIAN_POINT ( 'NONE',  ( 801.9858362298568863, -147.0783235625962959, -312.7379699480935642 ) ) ;
#22299 = CARTESIAN_POINT ( 'NONE',  ( 808.0189434323515343, -110.0891481129656597, 319.0252816721025511 ) ) ;
#22300 = CARTESIAN_POINT ( 'NONE',  ( 767.6429770376289525, -369.1800572038739574, -306.8695393053162093 ) ) ;
#22301 = LINE ( 'NONE', #1064, #36465 ) ;
#22302 = CARTESIAN_POINT ( 'NONE',  ( 999.9999999999992042, -599.0000000000001137, -359.0000000000000000 ) ) ;
#22303 = CARTESIAN_POINT ( 'NONE',  ( 762.3223304703356007, -223.5436935675107577, 322.3223304703362828 ) ) ;
#22304 = CARTESIAN_POINT ( 'NONE',  ( 783.0745993439762742, -32.19088175424425913, 365.1016975059196739 ) ) ;
#22305 = CARTESIAN_POINT ( 'NONE',  ( 757.8323909638827445, -386.6346026584191691, -352.1044303154654358 ) ) ;
#22306 = CARTESIAN_POINT ( 'NONE',  ( 795.1271208383656131, -452.8379544210779954, -371.6178728169206238 ) ) ;
#22307 = LINE ( 'NONE', #42883, #29181 ) ;
#22308 = CARTESIAN_POINT ( 'NONE',  ( 754.0944755984390895, -15.62377810805123524, 364.1009440267246760 ) ) ;
#22309 = VERTEX_POINT ( 'NONE', #20210 ) ;
#22310 = CARTESIAN_POINT ( 'NONE',  ( 802.7791456095903868, -172.7146871989598083, -329.0155153010375102 ) ) ;
#22311 = CARTESIAN_POINT ( 'NONE',  ( 788.7366044899766848, -35.90732993114770011, 316.5762568750059813 ) ) ;
#22312 = CARTESIAN_POINT ( 'NONE',  ( 812.6845335610512393, -223.9874144716869182, -353.5525998758768651 ) ) ;
#22313 = CARTESIAN_POINT ( 'NONE',  ( 744.8212110874229666, -354.8965053807774552, 336.2046728542121627 ) ) ;
#22314 = EDGE_LOOP ( 'NONE', ( #4901, #26632, #35334, #17867 ) ) ;
#22315 = CARTESIAN_POINT ( 'NONE',  ( 801.9419747391806368, -138.4527844766019200, -351.9812246680014027 ) ) ;
#22316 = CARTESIAN_POINT ( 'NONE',  ( 804.9363028652555840, -352.2709662947830225, 338.2165204200192079 ) ) ;
#22317 = CARTESIAN_POINT ( 'NONE',  ( 814.5518280994195948, -63.72551174932939233, -332.4837098697145734 ) ) ;
#22318 = CIRCLE ( 'NONE', #29004, 2.749999999999863665 ) ;
#22319 = VERTEX_POINT ( 'NONE', #34294 ) ;
#22320 = CARTESIAN_POINT ( 'NONE',  ( 763.0428371773158460, -11.46360902697159290, -358.7617431975195359 ) ) ;
#22321 = EDGE_LOOP ( 'NONE', ( #39398, #33969, #33519, #33762 ) ) ;
#22322 = CARTESIAN_POINT ( 'NONE',  ( 757.4527132478984868, -328.3726999360615650, -329.1273215169538844 ) ) ;
#22324 = CARTESIAN_POINT ( 'NONE',  ( 784.1219089521767955, -381.2817908451523294, 315.0488828828318333 ) ) ;
#22323 = CARTESIAN_POINT ( 'NONE',  ( 757.8323909638827445, -74.63460265842032015, 352.1044303154654358 ) ) ;
#22325 = CARTESIAN_POINT ( 'NONE',  ( 788.7366044899766848, -299.9073299311468759, -316.5762568750059813 ) ) ;
#22327 = CARTESIAN_POINT ( 'NONE',  ( 783.7566961878529810, -312.8965053807775689, 305.1792804349288417 ) ) ;
#22326 = CARTESIAN_POINT ( 'NONE',  ( 763.2262854647970016, -392.6346026584193396, 309.2812353651462445 ) ) ;
#22328 = CARTESIAN_POINT ( 'NONE',  ( 773.4516893846965786, -283.6454272087889308, -315.8398074228977066 ) ) ;
#22329 = CARTESIAN_POINT ( 'NONE',  ( 774.6858677611749044, -297.7255117493286889, -315.5713283507209894 ) ) ;
#22330 = FACE_BOUND ( 'NONE', #5229, .T. ) ;
#22331 = CARTESIAN_POINT ( 'NONE',  ( 797.6776695296629214, -139.5436935675110135, -357.6776695296636603 ) ) ;
#22332 = CARTESIAN_POINT ( 'NONE',  ( 998.9999999999992042, 249.9999999999998863, -360.0000000000000000 ) ) ;
#22333 = CARTESIAN_POINT ( 'NONE',  ( 755.2512626584698410, -415.5436935675102177, 315.2512626584710915 ) ) ;
#22335 = CARTESIAN_POINT ( 'NONE',  ( 939.9999999999992042, 62.85347435602262323, 357.4246812887967621 ) ) ;
#22334 = CARTESIAN_POINT ( 'NONE',  ( 989.9999999999992042, 469.9999999999999432, -210.0000000000000000 ) ) ;
#22336 = CARTESIAN_POINT ( 'NONE',  ( 762.1177392798416577, -90.55451811788041994, -309.8865473780659272 ) ) ;
#22337 = DIRECTION ( 'NONE',  ( 1.000000000000000000, 0.000000000000000000, 0.000000000000000000 ) ) ;
#22338 = DIRECTION ( 'NONE',  ( 0.000000000000000000, 0.000000000000000000, 1.000000000000000000 ) ) ;
#22339 = ADVANCED_FACE ( 'NONE', ( #2664 ), #13294, .T. ) ;
#22340 = CARTESIAN_POINT ( 'NONE',  ( 759.0159684113467620, -280.9181544815162965, 325.8855110935213020 ) ) ;
#22341 = CARTESIAN_POINT ( 'NONE',  ( 771.2633955100217236, -143.9073299311473590, 363.4237431249939618 ) ) ;
#22342 = VERTEX_POINT ( 'NONE', #25044 ) ;
#22343 = CARTESIAN_POINT ( 'NONE',  ( 813.1304606946831655, -137.9073299311473875, -352.3570229623691716 ) ) ;
#22344 = CARTESIAN_POINT ( 'NONE',  ( 789.9200121543843807, -337.9874144716865771, 317.0176451133914384 ) ) ;
#22345 = CARTESIAN_POINT ( 'NONE',  ( 879.9999999999992042, 99.99999999999984368, -360.0000000000000000 ) ) ;
#22346 = CARTESIAN_POINT ( 'NONE',  ( 772.3691319403857278, -431.2601417444136018, -315.8894580844506663 ) ) ;
#22347 = CARTESIAN_POINT ( 'NONE',  ( 745.7194118038753459, -61.64542720878961291, 348.7631598425976449 ) ) ;
#22348 = CARTESIAN_POINT ( 'NONE',  ( 767.7687537140311633, -263.9073299311469327, -372.7932403749916830 ) ) ;
#22349 = CARTESIAN_POINT ( 'NONE',  ( 745.4481719005789273, -195.7255117493289731, 347.5162901302853129 ) ) ;
#22350 = CARTESIAN_POINT ( 'NONE',  ( 781.7834795799800531, -130.8164208402383224, 315.0636971347436202 ) ) ;
#22351 = CIRCLE ( 'NONE', #15735, 2.749999999999808153 ) ;
#22352 = ORIENTED_EDGE ( 'NONE', *, *, #36529, .T. ) ;
#22353 = CARTESIAN_POINT ( 'NONE',  ( 801.9858362298568863, -291.0783235625957559, -312.7379699480935642 ) ) ;
#22354 = CARTESIAN_POINT ( 'NONE',  ( 790.0220218866281812, -7.099972663335241130, 363.2186876482849129 ) ) ;
#22355 = CARTESIAN_POINT ( 'NONE',  ( 808.0189434323515343, -350.0891481129648923, -319.0252816721025511 ) ) ;
#22356 = DIRECTION ( 'NONE',  ( -0.000000000000000000, 1.000000000000000000, -0.000000000000000000 ) ) ;
#22357 = CARTESIAN_POINT ( 'NONE',  ( 799.4546378042377910, -393.0783235625954717, 356.1575198192848006 ) ) ;
#22358 = ORIENTED_EDGE ( 'NONE', *, *, #25547, .F. ) ;
#22359 = CARTESIAN_POINT ( 'NONE',  ( 755.3201227861273992, -411.7255117493282910, -345.3687786644892981 ) ) ;
#22360 = EDGE_CURVE ( 'NONE', #33022, #38320, #39153, .T. ) ;
#22361 = CARTESIAN_POINT ( 'NONE',  ( 815.0009284576459549, -126.3510508353236048, -338.7629533639073429 ) ) ;
#22362 = FACE_OUTER_BOUND ( 'NONE', #4560, .T. ) ;
#22363 = CARTESIAN_POINT ( 'NONE',  ( 813.9316612368132837, -223.4419599262323857, 348.6739635108323228 ) ) ;
#22364 = CARTESIAN_POINT ( 'NONE',  ( 804.4286716492782716, -65.36187538569306810, 345.3141322388244703 ) ) ;
#22365 = VECTOR ( 'NONE', #26913, 1000.000000000000000 ) ;
#22366 = CARTESIAN_POINT ( 'NONE',  ( 755.0488828828309806, -233.8055962898687028, -344.1219089521771934 ) ) ;
#22367 = CARTESIAN_POINT ( 'NONE',  ( 755.0636971347428243, -244.2709662947834204, 341.7834795799807353 ) ) ;
#22368 = CARTESIAN_POINT ( 'NONE',  ( 791.1614460488616487, -59.26014174441473870, -373.5763878283158874 ) ) ;
#22369 = CARTESIAN_POINT ( 'NONE',  ( -949.5497976682736407, 120.6654763175833693, -209.9999999999999716 ) ) ;
#22370 = ORIENTED_EDGE ( 'NONE', *, *, #45621, .T. ) ;
#22371 = VERTEX_POINT ( 'NONE', #28518 ) ;
#22372 = CARTESIAN_POINT ( 'NONE',  ( 802.2119215644370342, -342.0090635724251342, -367.5423716828165084 ) ) ;
#22373 = CARTESIAN_POINT ( 'NONE',  ( 811.0346526505617248, -302.6346026584195670, 323.0537975583478101 ) ) ;
#22374 = ADVANCED_FACE ( 'NONE', ( #7728 ), #35434, .F. ) ;
#22375 = CARTESIAN_POINT ( 'NONE',  ( 815.0009284576459549, -30.35105083532391390, 338.7629533639073429 ) ) ;
#22376 = CARTESIAN_POINT ( 'NONE',  ( 804.1105419155481968, -171.8272453906074304, -347.6308680596136469 ) ) ;
#22377 = CARTESIAN_POINT ( 'NONE',  ( 759.7806653035534055, -198.9982390220562252, -324.8639956371180801 ) ) ;
#22378 = AXIS2_PLACEMENT_3D ( 'NONE', #25311, #39424, #35948 ) ;
#22379 = CARTESIAN_POINT ( 'NONE',  ( 755.5713283507202505, -389.3618753856919739, -334.6858677611754729 ) ) ;
#22380 = EDGE_LOOP ( 'NONE', ( #10678, #6936, #31238, #31362, #13577, #43835, #30123, #19668, #33749, #45544, #9777, #8372 ) ) ;
#22381 = AXIS2_PLACEMENT_3D ( 'NONE', #38098, #9459, #41551 ) ;
#22382 = ORIENTED_EDGE ( 'NONE', *, *, #10459, .F. ) ;
#22383 = CARTESIAN_POINT ( 'NONE',  ( 745.0891759886404770, -316.2709662947832499, 342.4968714119734159 ) ) ;
#22384 = DIRECTION ( 'NONE',  ( 0.000000000000000000, -0.3826834323650838421, -0.9238795325112891810 ) ) ;
#22385 = CARTESIAN_POINT ( 'NONE',  ( 763.8424801807145741, -210.0090635724255321, 320.5453621957614700 ) ) ;
#22386 = CARTESIAN_POINT ( 'NONE',  ( 311.1634899080286232, 260.0000000000000000, -199.9999999999963336 ) ) ;
#22387 = ADVANCED_FACE ( 'NONE', ( #42614 ), #334, .F. ) ;
#22388 = CARTESIAN_POINT ( 'NONE',  ( 773.4516893846965786, -187.6454272087892434, 315.8398074228977066 ) ) ;
#22389 = CARTESIAN_POINT ( 'NONE',  ( 804.4286716492782716, -41.36187538569314626, 345.3141322388244703 ) ) ;
#22390 = EDGE_LOOP ( 'NONE', ( #40021, #9608, #24146, #20828 ) ) ;
#22391 = CARTESIAN_POINT ( 'NONE',  ( 771.3260364891663130, -427.6454272087885897, -306.0683387631859773 ) ) ;
#22392 = CARTESIAN_POINT ( 'NONE',  ( 777.5031285880264704, -46.81642084023858530, -374.9108240113588408 ) ) ;
#22393 = CARTESIAN_POINT ( 'NONE',  ( 783.0433043558608688, -216.8965053807778816, 315.1538015810313027 ) ) ;
#22394 = CARTESIAN_POINT ( 'NONE',  ( 765.0180583372156207, -384.9982390220556567, -360.0135310231089534 ) ) ;
#22395 = CARTESIAN_POINT ( 'NONE',  ( 771.1735550268780344, -9.180057203875058747, -316.3353852180828198 ) ) ;
#22396 = AXIS2_PLACEMENT_3D ( 'NONE', #1659, #22906, #22688 ) ;
#22397 = CARTESIAN_POINT ( 'NONE',  ( 796.9462024416508257, -420.4527844766009252, 308.9653473494370246 ) ) ;
#22398 = CARTESIAN_POINT ( 'NONE',  ( 989.9999999999992042, -414.5899773927342835, -209.9999999999999716 ) ) ;
#22399 = CARTESIAN_POINT ( 'NONE',  ( 796.9571628226829034, -263.4636090269708006, -321.2382568024804641 ) ) ;
#22400 = CARTESIAN_POINT ( 'NONE',  ( 800.9747183278959710, -180.9982390220563389, -311.9810565676471583 ) ) ;
#22401 = CARTESIAN_POINT ( 'NONE',  ( 814.2001403089898304, -65.36187538569306810, 347.4397851343538264 ) ) ;
#22402 = CARTESIAN_POINT ( 'NONE',  ( 782.4968714119720516, -106.8164208402383935, 305.0891759886411023 ) ) ;
#22403 = LINE ( 'NONE', #5097, #37260 ) ;
#22404 = DIRECTION ( 'NONE',  ( -0.000000000000000000, -0.000000000000000000, -1.000000000000000000 ) ) ;
#22405 = ADVANCED_FACE ( 'NONE', ( #43056 ), #1012, .T. ) ;
#22406 = CARTESIAN_POINT ( 'NONE',  ( 766.4474001241216001, -379.0999726633341993, 307.3154664389482491 ) ) ;
#22407 = CARTESIAN_POINT ( 'NONE',  ( 745.5313806188320314, -399.2817908451522726, 333.7943932421247268 ) ) ;
#22408 = EDGE_CURVE ( 'NONE', #757, #4454, #43286, .T. ) ;
#22409 = DIRECTION ( 'NONE',  ( 0.000000000000000000, 0.000000000000000000, 1.000000000000000000 ) ) ;
#22410 = CARTESIAN_POINT ( 'NONE',  ( 782.4968714119720516, -346.8164208402376971, 305.0891759886411023 ) ) ;
#22411 = CARTESIAN_POINT ( 'NONE',  ( 767.8955696845333705, -312.4527844766012663, -362.1676090361162323 ) ) ;
#22412 = CARTESIAN_POINT ( 'NONE',  ( 801.9419747391806368, -450.4527844766009821, 351.9812246680014027 ) ) ;
#22413 = CIRCLE ( 'NONE', #6933, 10.00000000000000888 ) ;
#22414 = VECTOR ( 'NONE', #33606, 1000.000000000000000 ) ;
#22415 = CARTESIAN_POINT ( 'NONE',  ( 745.7194118038753459, -61.64542720878961291, -348.7631598425976449 ) ) ;
#22416 = CARTESIAN_POINT ( 'NONE',  ( 794.1144889064781864, -106.1692326535054889, -360.9840315886528401 ) ) ;
#22417 = CARTESIAN_POINT ( 'NONE',  ( 746.0683387631852383, -139.4419599262326699, 331.3260364891676204 ) ) ;
#22418 = CARTESIAN_POINT ( 'NONE',  ( 801.9419747391806368, -426.4527844766010389, 351.9812246680014027 ) ) ;
#22419 = CARTESIAN_POINT ( 'NONE',  ( 797.8594530101008786, -13.54369356751140785, -322.1405469898980982 ) ) ;
#22420 = CARTESIAN_POINT ( 'NONE',  ( 754.9735926884551418, -114.3510508353236617, -340.5236548041000333 ) ) ;
#22421 = CARTESIAN_POINT ( 'NONE',  ( 755.0636971347428243, -124.2709662947837899, -341.7834795799807353 ) ) ;
#22422 = CARTESIAN_POINT ( 'NONE',  ( 799.4546378042377910, -441.0783235625953580, -356.1575198192848006 ) ) ;
#22424 = CARTESIAN_POINT ( 'NONE',  ( 771.1735550268780344, -249.1800572038742700, 316.3353852180828198 ) ) ;
#22423 = CARTESIAN_POINT ( 'NONE',  ( 764.8639956371174549, -272.0891481129651197, 319.7806653035542013 ) ) ;
#22425 = CARTESIAN_POINT ( 'NONE',  ( -879.9999999999992042, 240.0000000000000853, -360.0000000000000000 ) ) ;
#22426 = ORIENTED_EDGE ( 'NONE', *, *, #30317, .F. ) ;
#22427 = CARTESIAN_POINT ( 'NONE',  ( 802.7791456095903868, 19.28531280103956647, 329.0155153010375102 ) ) ;
#22428 = AXIS2_PLACEMENT_3D ( 'NONE', #41312, #45006, #10342 ) ;
#22429 = EDGE_CURVE ( 'NONE', #4120, #36456, #14439, .T. ) ;
#22430 = VERTEX_POINT ( 'NONE', #18133 ) ;
#22431 = SHAPE_REPRESENTATION_RELATIONSHIP ( 'NONE' , 'NONE' ,  #2289, #44192 ) ;
#22432 = AXIS2_PLACEMENT_3D ( 'NONE', #43108, #4538, #31576 ) ;
#22433 = CARTESIAN_POINT ( 'NONE',  ( 746.8695393053151292, -197.9073299311472169, 327.6429770376306578 ) ) ;
#22434 = ADVANCED_FACE ( 'NONE', ( #11418 ), #28975, .F. ) ;
#22435 = CARTESIAN_POINT ( 'NONE',  ( 763.0428371773158460, -299.4636090269707438, 358.7617431975195359 ) ) ;
#22436 = CARTESIAN_POINT ( 'NONE',  ( 803.2186876482843445, -391.9874144716864066, 350.0220218866286928 ) ) ;
#22437 = VERTEX_POINT ( 'NONE', #573 ) ;
#22438 = CARTESIAN_POINT ( 'NONE',  ( 801.5560724626406000, -96.55451811788039151, -326.7756240680316182 ) ) ;
#22439 = CARTESIAN_POINT ( 'NONE',  ( 803.8556311672234642, -225.6237781080506011, 365.6418435158340117 ) ) ;
#22440 = CARTESIAN_POINT ( 'NONE',  ( 785.3141322388236176, -285.7255117493286889, -364.4286716492789537 ) ) ;
#22441 = ORIENTED_EDGE ( 'NONE', *, *, #1955, .T. ) ;
#22442 = CARTESIAN_POINT ( 'NONE',  ( 788.8264449731200330, -381.1800572038737869, -363.6646147819171233 ) ) ;
#22443 = CARTESIAN_POINT ( 'NONE',  ( 778.1981804954714335, -34.27096629478407408, -314.8072714833589885 ) ) ;
#22444 = CARTESIAN_POINT ( 'NONE',  ( 772.3691319403857278, -263.2601417444141134, 315.8894580844506663 ) ) ;
#22445 = ADVANCED_FACE ( 'NONE', ( #36349, #8186 ), #21807, .F. ) ;
#22446 = DIRECTION ( 'NONE',  ( -0.000000000000000000, 1.000000000000000000, 0.000000000000000000 ) ) ;
#22447 = FACE_BOUND ( 'NONE', #40169, .T. ) ;
#22448 = EDGE_CURVE ( 'NONE', #9510, #34870, #7972, .T. ) ;
#22449 = AXIS2_PLACEMENT_3D ( 'NONE', #5156, #11414, #19240 ) ;
#22450 = CARTESIAN_POINT ( 'NONE',  ( 797.8822607201568644, -30.55451811788062244, -370.1134526219340160 ) ) ;
#22451 = FACE_OUTER_BOUND ( 'NONE', #13332, .T. ) ;
#22452 = ORIENTED_EDGE ( 'NONE', *, *, #35629, .T. ) ;
#22453 = CARTESIAN_POINT ( 'NONE',  ( 814.4686193811664907, -291.2817908451525000, -346.2056067578752732 ) ) ;
#22454 = AXIS2_PLACEMENT_3D ( 'NONE', #29133, #8129, #32599 ) ;
#22455 = CARTESIAN_POINT ( 'NONE',  ( 757.7880784355613741, -162.0090635724256742, 312.4576283171834916 ) ) ;
#22457 = CARTESIAN_POINT ( 'NONE',  ( 767.8955696845333705, -288.4527844766014937, -362.1676090361162323 ) ) ;
#22456 = CARTESIAN_POINT ( 'NONE',  ( 187.1337867209877857, -185.0721577059061644, 75.19946970736494052 ) ) ;
#22458 = LINE ( 'NONE', #14879, #37071 ) ;
#22459 = CARTESIAN_POINT ( 'NONE',  ( 804.4086373105744769, -145.6454272087893287, -333.3843516231986541 ) ) ;
#22460 = CARTESIAN_POINT ( 'NONE',  ( 758.8095938919642549, -8.089148112965974136, 311.6929314249763365 ) ) ;
#22461 = FACE_OUTER_BOUND ( 'NONE', #18082, .T. ) ;
#22462 = CARTESIAN_POINT ( 'NONE',  ( 808.0189434323515343, -350.0891481129648923, -319.0252816721025511 ) ) ;
#22463 = CARTESIAN_POINT ( 'NONE',  ( 799.9999999999993179, -365.3551492539851893, -18.13243251470705886 ) ) ;
#22464 = CARTESIAN_POINT ( 'NONE',  ( 801.9419747391806368, -42.45278447660223264, 351.9812246680014027 ) ) ;
#22465 = CARTESIAN_POINT ( 'NONE',  ( 788.6739635108323228, -295.6454272087888739, 373.9316612368139090 ) ) ;
#22466 = CARTESIAN_POINT ( 'NONE',  ( 776.2433038121456548, -252.8965053807777394, -374.8207195650711014 ) ) ;
#22467 = CARTESIAN_POINT ( 'NONE',  ( 813.1304606946830518, -257.9073299311469896, 352.3570229623690580 ) ) ;
#22468 = CARTESIAN_POINT ( 'NONE',  ( 805.9055244015594326, -435.6237781080499190, -315.8990559732753240 ) ) ;
#22469 = PLANE ( 'NONE',  #21021 ) ;
#22470 = CIRCLE ( 'NONE', #9230, 10.00000000000000888 ) ;
#22471 = ORIENTED_EDGE ( 'NONE', *, *, #2953, .F. ) ;
#22472 = CARTESIAN_POINT ( 'NONE',  ( 771.1735550268778070, -345.1800572038739006, 316.3353852180827630 ) ) ;
#22473 = CARTESIAN_POINT ( 'NONE',  ( 790.0220218866281812, -79.09997266333503774, 363.2186876482849129 ) ) ;
#22474 = CARTESIAN_POINT ( 'NONE',  ( 805.1016975059191054, -30.89650538077846065, -343.0745993439771837 ) ) ;
#22475 = LINE ( 'NONE', #26176, #10717 ) ;
#22476 = LINE ( 'NONE', #5161, #20326 ) ;
#22477 = CARTESIAN_POINT ( 'NONE',  ( 766.5853460496234675, -133.9874144716872024, 372.3518521366060554 ) ) ;
#22478 = CARTESIAN_POINT ( 'NONE',  ( 757.8323909638827445, -386.6346026584191691, 352.1044303154654358 ) ) ;
#22479 = ORIENTED_EDGE ( 'NONE', *, *, #36240, .F. ) ;
#22480 = CARTESIAN_POINT ( 'NONE',  ( 784.0799538623451781, -323.8055962898684470, -364.6971507214555572 ) ) ;
#22481 = CARTESIAN_POINT ( 'NONE',  ( 781.8018195045266339, -142.2709662947837330, 365.1927285166406705 ) ) ;
#22482 = VECTOR ( 'NONE', #9249, 1000.000000000000000 ) ;
#22483 = CARTESIAN_POINT ( 'NONE',  ( 778.7502325331095108, -336.3510508353228943, -304.6391490659818828 ) ) ;
#22484 = FACE_OUTER_BOUND ( 'NONE', #45352, .T. ) ;
#22485 = CARTESIAN_POINT ( 'NONE',  ( 814.9108240113580450, 7.729033705215793582, 337.5031285880265273 ) ) ;
#22486 = ORIENTED_EDGE ( 'NONE', *, *, #28278, .F. ) ;
#22487 = CARTESIAN_POINT ( 'NONE',  ( 757.8323909638827445, -362.6346026584194533, 352.1044303154654358 ) ) ;
#22488 = CIRCLE ( 'NONE', #26189, 8.024999999999948841 ) ;
#22489 = EDGE_CURVE ( 'NONE', #24672, #13253, #30627, .T. ) ;
#22490 = CARTESIAN_POINT ( 'NONE',  ( 796.7845633553578182, -81.62377810805104161, -358.5707757039688204 ) ) ;
#22491 = ORIENTED_EDGE ( 'NONE', *, *, #2744, .T. ) ;
#22492 = DIRECTION ( 'NONE',  ( 1.000000000000000000, 0.000000000000000000, 0.000000000000000000 ) ) ;
#22493 = CARTESIAN_POINT ( 'NONE',  ( 801.1904061080336987, -188.0891481129653187, -368.3070685750235498 ) ) ;
#22494 = ORIENTED_EDGE ( 'NONE', *, *, #14195, .T. ) ;
#22495 = CARTESIAN_POINT ( 'NONE',  ( 800.2193346964446619, -186.9982390220563104, -355.1360043628816925 ) ) ;
#22496 = ORIENTED_EDGE ( 'NONE', *, *, #17335, .F. ) ;
#22497 = CARTESIAN_POINT ( 'NONE',  ( 799.2566176426618085, -432.0090635724247932, -324.0069404352559559 ) ) ;
#22498 = AXIS2_PLACEMENT_3D ( 'NONE', #35723, #18196, #8026 ) ;
#22499 = CARTESIAN_POINT ( 'NONE',  ( 771.1735550268778070, 14.81994279612486309, 316.3353852180827630 ) ) ;
#22500 = CARTESIAN_POINT ( 'NONE',  ( 756.7813123517142913, -163.9874144716871456, 329.9779781133712504 ) ) ;
#22501 = ADVANCED_FACE ( 'NONE', ( #42367 ), #39374, .T. ) ;
#22503 = LINE ( 'NONE', #12122, #448 ) ;
#22502 = FACE_OUTER_BOUND ( 'NONE', #29341, .T. ) ;
#22504 = AXIS2_PLACEMENT_3D ( 'NONE', #23383, #43953, #12097 ) ;
#22505 = ORIENTED_EDGE ( 'NONE', *, *, #37682, .T. ) ;
#22506 = CARTESIAN_POINT ( 'NONE',  ( 755.8894580844503253, -423.8272453906067199, -332.3691319403863531 ) ) ;
#22507 = CARTESIAN_POINT ( 'NONE',  ( -26.63011601220122060, -365.3551492539851893, -18.13243251470705886 ) ) ;
#22508 = CARTESIAN_POINT ( 'NONE',  ( 771.3260364891663130, -187.6454272087892434, -306.0683387631859773 ) ) ;
#22509 = CARTESIAN_POINT ( 'NONE',  ( 778.7629533639073998, -80.73633629969864955, 375.0009284576466371 ) ) ;
#22511 = CARTESIAN_POINT ( 'NONE',  ( 785.3687786644884454, -203.3618753856925991, -315.3201227861279676 ) ) ;
#22510 = CARTESIAN_POINT ( 'NONE',  ( 799.9999999999993179, -512.9681489794448908, -309.9999999999998863 ) ) ;
#22512 = CARTESIAN_POINT ( 'NONE',  ( 756.1348686366196716, -329.2601417444138860, -347.5531968255698416 ) ) ;
#22513 = DIRECTION ( 'NONE',  ( 0.000000000000000000, -0.000000000000000000, -1.000000000000000000 ) ) ;
#22514 = CARTESIAN_POINT ( 'NONE',  ( 748.6759233522253680, -232.3726999360617924, -324.3348316497537098 ) ) ;
#22515 = DIRECTION ( 'NONE',  ( -1.000000000000000000, -0.000000000000000000, 0.000000000000000000 ) ) ;
#22516 = DIRECTION ( 'NONE',  ( 1.892425610156518354E-16, 1.000000000000000000, -0.000000000000000000 ) ) ;
#22517 = CARTESIAN_POINT ( 'NONE',  ( 790.9844846989617508, -46.37269993606239638, -317.2208543904092721 ) ) ;
#22518 = CARTESIAN_POINT ( 'NONE',  ( 802.9823548866075953, -409.0999726633340288, 330.0799878456151077 ) ) ;
#22519 = VECTOR ( 'NONE', #32773, 1000.000000000000000 ) ;
#22520 = CARTESIAN_POINT ( 'NONE',  ( 748.9653473494365699, -242.6346026584197659, -356.9462024416520762 ) ) ;
#22521 = LINE ( 'NONE', #36849, #27566 ) ;
#22522 = CARTESIAN_POINT ( 'NONE',  ( 771.1735550268778070, -9.180057203875058747, -316.3353852180827630 ) ) ;
#22523 = AXIS2_PLACEMENT_3D ( 'NONE', #34775, #41958, #6145 ) ;
#22524 = CARTESIAN_POINT ( 'NONE',  ( 814.2805881961230625, -193.6454272087891582, 331.2368401574024119 ) ) ;
#22525 = CARTESIAN_POINT ( 'NONE',  ( 808.7758568127978833, -124.1692326535054463, -320.0363995740631822 ) ) ;
#22526 = CARTESIAN_POINT ( 'NONE',  ( 796.9462024416508257, -156.4527844766018916, 308.9653473494370246 ) ) ;
#22527 = CARTESIAN_POINT ( 'NONE',  ( 804.7487373415286811, -379.5436935675102745, -364.7487373415288516 ) ) ;
#22528 = VECTOR ( 'NONE', #6619, 1000.000000000000000 ) ;
#22529 = CARTESIAN_POINT ( 'NONE',  ( 767.9999999999992042, 240.0000000000000853, -360.0000000000000000 ) ) ;
#22530 = FACE_OUTER_BOUND ( 'NONE', #289, .T. ) ;
#22531 = CARTESIAN_POINT ( 'NONE',  ( 800.2193346964447755, -234.9982390220561683, 355.1360043628815788 ) ) ;
#22532 = CARTESIAN_POINT ( 'NONE',  ( 763.8424801807145741, -18.00906357242611477, 320.5453621957614700 ) ) ;
#22533 = CARTESIAN_POINT ( 'NONE',  ( 759.9864689768902508, -386.0891481129647786, -354.9819416627836404 ) ) ;
#22534 = VECTOR ( 'NONE', #43057, 1000.000000000000000 ) ;
#22535 = CARTESIAN_POINT ( 'NONE',  ( 778.7629533639073998, -8.736336299698871599, -375.0009284576466371 ) ) ;
#22536 = DIRECTION ( 'NONE',  ( 0.000000000000000000, -0.6594541114781790059, 0.7517448203044204691 ) ) ;
#22537 = CARTESIAN_POINT ( 'NONE',  ( 808.7758568127978833, -28.16923265350574468, 320.0363995740631822 ) ) ;
#22538 = ORIENTED_EDGE ( 'NONE', *, *, #4622, .T. ) ;
#22539 = VECTOR ( 'NONE', #45182, 1000.000000000000000 ) ;
#22540 = CARTESIAN_POINT ( 'NONE',  ( 789.9200121543843807, -241.9874144716869182, -317.0176451133914384 ) ) ;
#22541 = CARTESIAN_POINT ( 'NONE',  ( 757.8323909638827445, -26.63460265842045871, 352.1044303154654358 ) ) ;
#22542 = CIRCLE ( 'NONE', #9270, 8.024999999999948841 ) ;
#22543 = CARTESIAN_POINT ( 'NONE',  ( 811.6461892240364477, -220.7146871989596661, -324.1737431748509835 ) ) ;
#22544 = CARTESIAN_POINT ( 'NONE',  ( -598.8365100919716042, 260.0000000000001705, -199.9999999999899671 ) ) ;
#22545 = CARTESIAN_POINT ( 'NONE',  ( 764.3348316497523456, -334.7146871989593251, 308.6759233522265617 ) ) ;
#22546 = CARTESIAN_POINT ( 'NONE',  ( 794.9819416627830151, -84.99823902205663728, -319.9864689768909898 ) ) ;
#22547 = VERTEX_POINT ( 'NONE', #25505 ) ;
#22548 = CARTESIAN_POINT ( 'NONE',  ( 751.2241431872005251, -424.1692326535044799, 359.9636004259367610 ) ) ;
#22549 = CARTESIAN_POINT ( 'NONE',  ( 765.0180583372156207, -144.9982390220564525, -360.0135310231089534 ) ) ;
#22550 = CARTESIAN_POINT ( 'NONE',  ( 801.9419747391806368, -330.4527844766013231, 351.9812246680014027 ) ) ;
#22551 = CARTESIAN_POINT ( 'NONE',  ( 814.9108240113580450, -64.27096629478397460, -337.5031285880265273 ) ) ;
#22552 = CARTESIAN_POINT ( 'NONE',  ( 803.4237431249931660, -63.18005720387488822, -331.2633955100225194 ) ) ;
#22553 = ORIENTED_EDGE ( 'NONE', *, *, #15168, .T. ) ;
#22554 = CARTESIAN_POINT ( 'NONE',  ( 804.4086373105744769, -1.645427208789804308, -333.3843516231986541 ) ) ;
#22555 = AXIS2_PLACEMENT_3D ( 'NONE', #28484, #10702, #18557 ) ;
#22556 = ORIENTED_EDGE ( 'NONE', *, *, #28976, .F. ) ;
#22557 = CARTESIAN_POINT ( 'NONE',  ( 759.0159684113467620, -328.9181544815160692, -325.8855110935213020 ) ) ;
#22559 = CARTESIAN_POINT ( 'NONE',  ( 796.9571628226829034, -383.4636090269704596, 321.2382568024804641 ) ) ;
#22558 = CARTESIAN_POINT ( 'NONE',  ( 804.9363028652555840, -64.27096629478397460, 338.2165204200192079 ) ) ;
#22560 = VECTOR ( 'NONE', #40492, 1000.000000000000000 ) ;
#22563 = CARTESIAN_POINT ( 'NONE',  ( 747.3154664389472828, -307.9874144716866340, 326.4474001241230781 ) ) ;
#22562 = LINE ( 'NONE', #19327, #31400 ) ;
#22561 = CARTESIAN_POINT ( 'NONE',  ( 814.5518280994195948, -447.7255117493281205, 332.4837098697145166 ) ) ;
#22564 = CARTESIAN_POINT ( 'NONE',  ( 813.2346286133761168, -101.2601417444146250, 328.9521613784389160 ) ) ;
#22565 = CARTESIAN_POINT ( 'NONE',  ( 796.9571628226829034, -311.4636090269706870, -321.2382568024804641 ) ) ;
#22566 = CARTESIAN_POINT ( 'NONE',  ( 797.8594530101008786, -301.5436935675105588, -322.1405469898980982 ) ) ;
#22567 = CARTESIAN_POINT ( 'NONE',  ( 755.5713283507202505, -149.3618753856928265, -334.6858677611754729 ) ) ;
#22568 = CARTESIAN_POINT ( 'NONE',  ( 747.2067596250078623, -435.1800572038737869, 352.2312462859687230 ) ) ;
#22569 = VECTOR ( 'NONE', #14045, 1000.000000000000000 ) ;
#22571 = LINE ( 'NONE', #8503, #12296 ) ;
#22570 = CARTESIAN_POINT ( 'NONE',  ( 759.2380499001254748, 21.41625977839825978, 318.3449445151863415 ) ) ;
#22572 = CARTESIAN_POINT ( 'NONE',  ( 805.6418435158337843, -101.4636090269713264, -363.8556311672236916 ) ) ;
#22573 = DIRECTION ( 'NONE',  ( 0.000000000000000000, -1.000000000000000000, 0.000000000000000000 ) ) ;
#22574 = LINE ( 'NONE', #11962, #30432 ) ;
#22575 = VECTOR ( 'NONE', #17289, 1000.000000000000000 ) ;
#22576 = CARTESIAN_POINT ( 'NONE',  ( 779.4763451958990572, -296.7363362996979390, 365.0264073115438919 ) ) ;
#22577 = CARTESIAN_POINT ( 'NONE',  ( 774.6858677611749044, -177.7255117493290868, 315.5713283507209894 ) ) ;
#22578 = VERTEX_POINT ( 'NONE', #32669 ) ;
#22579 = CARTESIAN_POINT ( 'NONE',  ( 777.4774526936600978, -130.2709662947837614, -304.7301800767028226 ) ) ;
#22580 = CARTESIAN_POINT ( 'NONE',  ( 763.2154366446407039, -333.6237781080502600, 321.4292242960311228 ) ) ;
#22581 = CARTESIAN_POINT ( 'NONE',  ( 745.7194118038753459, -85.64542720878952764, 348.7631598425976449 ) ) ;
#22582 = CARTESIAN_POINT ( 'NONE',  ( 810.7187646348534145, -258.4527844766016074, -356.7737145352016341 ) ) ;
#22583 = DIRECTION ( 'NONE',  ( 0.000000000000000000, -0.6438296778008192334, 0.7651688349527138167 ) ) ;
#22584 = CARTESIAN_POINT ( 'NONE',  ( 781.7834795799800531, -106.8164208402383935, 315.0636971347436202 ) ) ;
#22585 = CARTESIAN_POINT ( 'NONE',  ( 751.2241431872005251, -328.1692326535048210, -359.9636004259367610 ) ) ;
#22586 = CARTESIAN_POINT ( 'NONE',  ( 787.4397851343537695, -93.72551174932934259, -374.2001403089903988 ) ) ;
#22587 = CARTESIAN_POINT ( 'NONE',  ( 801.5560724626406000, -24.55451811788064020, 326.7756240680316182 ) ) ;
#22588 = CARTESIAN_POINT ( 'NONE',  ( 796.9462024416508257, -348.4527844766012663, -308.9653473494370246 ) ) ;
#22589 = CARTESIAN_POINT ( 'NONE',  ( 794.9999999999993179, 205.0000000000000568, -255.0000000000000000 ) ) ;
#22590 = CARTESIAN_POINT ( 'NONE',  ( 775.9200461376533440, -407.8055962898681628, 315.3028492785443291 ) ) ;
#22591 = EDGE_LOOP ( 'NONE', ( #27916, #22888, #41951, #6375 ) ) ;
#22592 = VECTOR ( 'NONE', #44213, 1000.000000000000000 ) ;
#22593 = CARTESIAN_POINT ( 'NONE',  ( 762.1405469898971887, -217.5436935675107293, -357.8594530101015607 ) ) ;
#22594 = CARTESIAN_POINT ( 'NONE',  ( 815.1787889125755555, -102.8965053807782368, -343.7953271457877804 ) ) ;
#22595 = DIRECTION ( 'NONE',  ( -1.000000000000000000, -0.000000000000000000, -0.000000000000000000 ) ) ;
#22596 = CARTESIAN_POINT ( 'NONE',  ( 759.8311093483677041, -238.1692326535050768, 310.9282345327691814 ) ) ;
#22597 = CARTESIAN_POINT ( 'NONE',  ( 803.6646147819162707, -41.90732993114767879, 348.8264449731211130 ) ) ;
#22598 = EDGE_LOOP ( 'NONE', ( #16079, #9718, #13032 ) ) ;
#22599 = CARTESIAN_POINT ( 'NONE',  ( 756.1348686366196716, -233.2601417444141987, -347.5531968255698416 ) ) ;
#22600 = CARTESIAN_POINT ( 'NONE',  ( 803.6646147819161570, -233.9073299311470180, 348.8264449731210561 ) ) ;
#22601 = VECTOR ( 'NONE', #3624, 1000.000000000000114 ) ;
#22602 = CARTESIAN_POINT ( 'NONE',  ( 792.2312462859673587, 12.09267006885214180, -307.2067596250082602 ) ) ;
#22603 = CARTESIAN_POINT ( 'NONE',  ( 764.3348316497523456, -70.71468719896014932, -308.6759233522265617 ) ) ;
#22604 = ADVANCED_FACE ( 'NONE', ( #15117 ), #12957, .F. ) ;
#22605 = LINE ( 'NONE', #5064, #40876 ) ;
#22606 = VERTEX_POINT ( 'NONE', #29207 ) ;
#22607 = VERTEX_POINT ( 'NONE', #18810 ) ;
#22608 = CARTESIAN_POINT ( 'NONE',  ( 793.5525998758768083, -391.0999726633340288, -372.6845335610516941 ) ) ;
#22609 = CARTESIAN_POINT ( 'NONE',  ( 778.2165204200184689, -238.8164208402379813, -364.9363028652563230 ) ) ;
#22610 = CARTESIAN_POINT ( 'NONE',  ( 748.9653473494365699, -314.6346026584195101, 356.9462024416520762 ) ) ;
#22611 = CARTESIAN_POINT ( 'NONE',  ( 773.7943932421234194, -23.80559628986938847, 305.5313806188329409 ) ) ;
#22612 = CARTESIAN_POINT ( 'NONE',  ( 799.2566176426618085, -216.0090635724255037, -324.0069404352559559 ) ) ;
#22613 = CARTESIAN_POINT ( 'NONE',  ( 762.3223304703356007, -175.5436935675108998, -322.3223304703362828 ) ) ;
#22614 = CARTESIAN_POINT ( 'NONE',  ( 778.2165204200184689, -382.8164208402374697, -364.9363028652563230 ) ) ;
#22615 = EDGE_LOOP ( 'NONE', ( #34144, #15910, #5862, #39612 ) ) ;
#22616 = CARTESIAN_POINT ( 'NONE',  ( 791.9812246680005501, -452.6346026584191691, -361.9419747391813189 ) ) ;
#22617 = ORIENTED_EDGE ( 'NONE', *, *, #35689, .T. ) ;
#22618 = CARTESIAN_POINT ( 'NONE',  ( 787.4397851343537695, -333.7255117493286320, 374.2001403089903988 ) ) ;
#22619 = CARTESIAN_POINT ( 'NONE',  ( 928.0249999999991815, 219.9999999999998863, 360.0000000000000000 ) ) ;
#22620 = CARTESIAN_POINT ( 'NONE',  ( 760.5453621957607311, -357.0783235625956422, 323.8424801807151425 ) ) ;
#22621 = DIRECTION ( 'NONE',  ( 1.000000000000000000, 0.000000000000000000, 0.000000000000000000 ) ) ;
#22622 = AXIS2_PLACEMENT_3D ( 'NONE', #26542, #8993, #5519 ) ;
#22623 = CARTESIAN_POINT ( 'NONE',  ( -78.83651009197140525, 260.0000000000000568, -199.9999999999936051 ) ) ;
#22624 = CARTESIAN_POINT ( 'NONE',  ( 757.0176451133909268, -205.0999726633346256, 349.9200121543848354 ) ) ;
#22625 = CARTESIAN_POINT ( 'NONE',  ( 805.1927285166397041, -40.81642084023859951, 341.8018195045277707 ) ) ;
#22626 = EDGE_CURVE ( 'NONE', #9857, #12054, #22251, .T. ) ;
#22627 = ORIENTED_EDGE ( 'NONE', *, *, #4735, .F. ) ;
#22628 = CARTESIAN_POINT ( 'NONE',  ( 815.3608509340175488, -410.7363362996976548, -341.2497674668889545 ) ) ;
#22629 = CIRCLE ( 'NONE', #6395, 7.999999999999896083 ) ;
#22630 = CARTESIAN_POINT ( 'NONE',  ( 792.2312462859673587, -35.90732993114770011, -307.2067596250082602 ) ) ;
#22631 = CARTESIAN_POINT ( 'NONE',  ( 804.1601925771018387, -223.4419599262323857, 346.5483106153029098 ) ) ;
#22632 = CIRCLE ( 'NONE', #26331, 8.025000000000003908 ) ;
#22633 = CARTESIAN_POINT ( 'NONE',  ( 757.8323909638827445, -410.6346026584191122, -352.1044303154654358 ) ) ;
#22634 = CARTESIAN_POINT ( 'NONE',  ( 800.2193346964446619, 5.001760977943074948, -355.1360043628816925 ) ) ;
#22635 = CARTESIAN_POINT ( 'NONE',  ( 787.4397851343537695, -429.7255117493282910, 374.2001403089903988 ) ) ;
#22636 = LINE ( 'NONE', #40208, #30347 ) ;
#22637 = CARTESIAN_POINT ( 'NONE',  ( 799.2566176426618085, -264.0090635724253616, -324.0069404352559559 ) ) ;
#22638 = CARTESIAN_POINT ( 'NONE',  ( 747.2067596250078623, -171.1800572038745543, -352.2312462859687230 ) ) ;
#22639 = CIRCLE ( 'NONE', #38151, 6.118999999999985562 ) ;
#22640 = CARTESIAN_POINT ( 'NONE',  ( 772.5602148656447525, -33.72551174932952733, 305.7998596910095443 ) ) ;
#22641 = CARTESIAN_POINT ( 'NONE',  ( 792.3570229623688874, -93.18005720387481006, 373.1304606946836202 ) ) ;
#22642 = DIRECTION ( 'NONE',  ( 1.000000000000000000, -1.880165489482579047E-16, -0.000000000000000000 ) ) ;
#22643 = DIRECTION ( 'NONE',  ( 0.000000000000000000, -0.3826834323650838421, -0.9238795325112891810 ) ) ;
#22644 = FACE_OUTER_BOUND ( 'NONE', #22380, .T. ) ;
#22645 = CARTESIAN_POINT ( 'NONE',  ( 777.4774526936600978, -346.2709662947830793, 304.7301800767027657 ) ) ;
#22646 = CARTESIAN_POINT ( 'NONE',  ( 778.1981804954714335, -322.2709662947830225, -314.8072714833589885 ) ) ;
#22647 = ADVANCED_FACE ( 'NONE', ( #16233 ), #33331, .F. ) ;
#22648 = CARTESIAN_POINT ( 'NONE',  ( 804.9511171171677688, 18.19440371013048008, 335.8780910478229202 ) ) ;
#22649 = CARTESIAN_POINT ( 'NONE',  ( 793.5525998758768083, -103.0999726633349525, -372.6845335610516941 ) ) ;
#22650 = CARTESIAN_POINT ( 'NONE',  ( 793.2243759319678702, -122.5328690171417918, -318.4439275373583200 ) ) ;
#22651 = CARTESIAN_POINT ( 'NONE',  ( 793.4146539503750546, -145.9874144716871740, 307.6481478633938877 ) ) ;
#22652 = CARTESIAN_POINT ( 'NONE',  ( 778.2165204200184689, -430.8164208402374129, 364.9363028652563230 ) ) ;
#22653 = VECTOR ( 'NONE', #4811, 1000.000000000000000 ) ;
#22654 = CARTESIAN_POINT ( 'NONE',  ( 756.1443688327750579, -165.6237781080507716, 314.3581564841659315 ) ) ;
#22655 = CARTESIAN_POINT ( 'NONE',  ( 797.6776695296629214, -19.54369356751139364, -357.6776695296636603 ) ) ;
#22656 = CARTESIAN_POINT ( 'NONE',  ( 758.6633372737375112, -140.5328690171417634, -326.9102291470432533 ) ) ;
#22657 = CARTESIAN_POINT ( 'NONE',  ( 802.1676090361156639, -134.6346026584201070, -327.8955696845344505 ) ) ;
#22658 = CARTESIAN_POINT ( 'NONE',  ( 755.5713283507202505, -125.3618753856928834, 334.6858677611754729 ) ) ;
#22659 = EDGE_CURVE ( 'NONE', #33885, #28618, #1247, .T. ) ;
#22660 = CARTESIAN_POINT ( 'NONE',  ( 804.9511171171677688, -437.8055962898679923, -335.8780910478229202 ) ) ;
#22662 = CARTESIAN_POINT ( 'NONE',  ( 794.9819416627830151, -252.9982390220560831, 319.9864689768909898 ) ) ;
#22661 = CARTESIAN_POINT ( 'NONE',  ( 759.9864689768902508, -266.0891481129651197, 354.9819416627836404 ) ) ;
#22663 = DIRECTION ( 'NONE',  ( 0.000000000000000000, 0.6755902076156502511, 0.7372773368101330771 ) ) ;
#22664 = ORIENTED_EDGE ( 'NONE', *, *, #39050, .T. ) ;
#22665 = CARTESIAN_POINT ( 'NONE',  ( 795.9930595647434757, 20.92167643740319605, 320.7433823573372820 ) ) ;
#22666 = CARTESIAN_POINT ( 'NONE',  ( 771.3260364891663130, -259.6454272087890445, -306.0683387631859773 ) ) ;
#22667 = AXIS2_PLACEMENT_3D ( 'NONE', #43296, #32454, #39627 ) ;
#22668 = VERTEX_POINT ( 'NONE', #30097 ) ;
#22669 =( NAMED_UNIT ( * ) SI_UNIT ( $, .STERADIAN. ) SOLID_ANGLE_UNIT ( ) );
#22670 = CARTESIAN_POINT ( 'NONE',  ( 787.5162901302840055, -203.3618753856926276, 305.4481719005793252 ) ) ;
#22671 = CARTESIAN_POINT ( 'NONE',  ( 772.4468031744293057, -297.8272453906070041, 363.8651313633793620 ) ) ;
#22672 = CARTESIAN_POINT ( 'NONE',  ( 805.1016975059191054, -414.8965053807771710, 343.0745993439771837 ) ) ;
#22673 = VERTEX_POINT ( 'NONE', #40949 ) ;
#22674 = CARTESIAN_POINT ( 'NONE',  ( 804.4086373105744769, -73.64542720878957027, -333.3843516231986541 ) ) ;
#22675 = CARTESIAN_POINT ( 'NONE',  ( 755.5713283507202505, -293.3618753856923718, -334.6858677611754729 ) ) ;
#22676 = ORIENTED_EDGE ( 'NONE', *, *, #7494, .F. ) ;
#22677 = CARTESIAN_POINT ( 'NONE',  ( 767.8955696845333705, -384.4527844766011526, -362.1676090361162323 ) ) ;
#22678 = CARTESIAN_POINT ( 'NONE',  ( 755.3201227861273992, -51.72551174932946338, -345.3687786644892981 ) ) ;
#22679 = ADVANCED_FACE ( 'NONE', ( #1462 ), #15349, .F. ) ;
#22680 = CARTESIAN_POINT ( 'NONE',  ( 786.6156483768007774, -265.4419599262323004, 315.5913626894246136 ) ) ;
#22681 = DIRECTION ( 'NONE',  ( 1.000000000000000000, 0.000000000000000000, 0.000000000000000000 ) ) ;
#22682 = DIRECTION ( 'NONE',  ( 1.000000000000000000, -0.000000000000000000, -0.000000000000000000 ) ) ;
#22683 = CARTESIAN_POINT ( 'NONE',  ( 814.4686193811664907, -27.28179084515336328, -346.2056067578752732 ) ) ;
#22684 = CYLINDRICAL_SURFACE ( 'NONE', #25501, 20.00000000000001776 ) ;
#22685 = EDGE_LOOP ( 'NONE', ( #26536, #25700, #3546, #43018 ) ) ;
#22686 = CARTESIAN_POINT ( 'NONE',  ( 745.5313806188320314, -303.2817908451525000, -333.7943932421247268 ) ) ;
#22687 = CARTESIAN_POINT ( 'NONE',  ( 749.5768839229115201, -180.5545181178801499, 358.0661480581553064 ) ) ;
#22689 = CARTESIAN_POINT ( 'NONE',  ( 778.2165204200184689, -286.8164208402378677, -364.9363028652563230 ) ) ;
#22688 = DIRECTION ( 'NONE',  ( 0.000000000000000000, -0.000000000000000000, -1.000000000000000000 ) ) ;
#22690 = LINE ( 'NONE', #36787, #40703 ) ;
#22691 = CARTESIAN_POINT ( 'NONE',  ( 793.9708237608222134, -166.9181544815165523, -319.2295555964448681 ) ) ;
#22692 = CARTESIAN_POINT ( 'NONE',  ( 799.9999999999993179, -512.9681489794448908, -309.9999999999998863 ) ) ;
#22693 = CARTESIAN_POINT ( 'NONE',  ( 755.2512626584698410, -343.5436935675103314, -315.2512626584710915 ) ) ;
#22694 = SURFACE_STYLE_USAGE ( .BOTH. , #15770 ) ;
#22695 = CARTESIAN_POINT ( 'NONE',  ( 800.2193346964447755, -42.99823902205675807, 355.1360043628815788 ) ) ;
#22696 = EDGE_CURVE ( 'NONE', #928, #282, #29894, .T. ) ;
#22697 = CARTESIAN_POINT ( 'NONE',  ( 814.8207195650702488, -290.1908817542434349, 336.2433038121456548 ) ) ;
#22698 = CARTESIAN_POINT ( 'NONE',  ( 782.4968714119720516, -274.8164208402378108, 305.0891759886411023 ) ) ;
#22699 = CARTESIAN_POINT ( 'NONE',  ( 815.2698199232961542, 7.183579159761247723, -342.5225473063383106 ) ) ;
#22700 = FACE_BOUND ( 'NONE', #26050, .T. ) ;
#22701 = EDGE_CURVE ( 'NONE', #14461, #40963, #36804, .T. ) ;
#22702 = EDGE_LOOP ( 'NONE', ( #16572, #27954, #22486, #19305, #3553, #31711, #36135, #25010, #904, #3384, #2374, #25845, #35930, #45125, #37859, #33471, #42569, #38240 ) ) ;
#22703 = CARTESIAN_POINT ( 'NONE',  ( 802.1676090361156639, -350.6346026584192828, 327.8955696845344505 ) ) ;
#22704 = CARTESIAN_POINT ( 'NONE',  ( 755.5913626894240451, -109.6454272087894566, 346.6156483768012890 ) ) ;
#22705 = CARTESIAN_POINT ( 'NONE',  ( 764.0069404352550464, -15.07832356259669560, -359.2566176426627180 ) ) ;
#22706 = FACE_OUTER_BOUND ( 'NONE', #43566, .T. ) ;
#22707 = CARTESIAN_POINT ( 'NONE',  ( 989.9999999999992042, -184.9457194955396631, -62.92409052808250891 ) ) ;
#22708 = CARTESIAN_POINT ( 'NONE',  ( 811.6461892240364477, -124.7146871989599930, 324.1737431748509835 ) ) ;
#22709 = CARTESIAN_POINT ( 'NONE',  ( 755.5713283507202505, -389.3618753856919739, 334.6858677611754729 ) ) ;
#22710 = EDGE_LOOP ( 'NONE', ( #42580, #44261, #1432, #12074 ) ) ;
#22711 = CARTESIAN_POINT ( 'NONE',  ( 803.4237431249931660, -39.18005720387496638, -331.2633955100225194 ) ) ;
#22712 = EDGE_CURVE ( 'NONE', #43744, #1441, #22475, .T. ) ;
#22713 = EDGE_CURVE ( 'NONE', #4120, #16303, #19035, .T. ) ;
#22714 = CARTESIAN_POINT ( 'NONE',  ( 800.7704444035546203, -340.1692326535047641, -326.0291762391768771 ) ) ;
#22715 = CARTESIAN_POINT ( 'NONE',  ( 802.1676090361156639, -158.6346026584199933, 327.8955696845344505 ) ) ;
#22716 = UNCERTAINTY_MEASURE_WITH_UNIT (LENGTH_MEASURE( 1.000000000000000082E-05 ), #35391, 'distance_accuracy_value', 'NONE');
#22717 = CARTESIAN_POINT ( 'NONE',  ( 786.2056067578752163, -323.8055962898684470, -374.4686193811670023 ) ) ;
#22718 = DIRECTION ( 'NONE',  ( -0.000000000000000000, -0.000000000000000000, 1.000000000000000000 ) ) ;
#22719 = VERTEX_POINT ( 'NONE', #19244 ) ;
#22720 = CARTESIAN_POINT ( 'NONE',  ( 771.1735550268778070, -345.1800572038739006, 316.3353852180827630 ) ) ;
#22721 = VERTEX_POINT ( 'NONE', #29429 ) ;
#22722 =( NAMED_UNIT ( * ) PLANE_ANGLE_UNIT ( ) SI_UNIT ( $, .RADIAN. ) );
#22723 = CARTESIAN_POINT ( 'NONE',  ( 812.7932403749906598, -183.1800572038744974, -327.7687537140311633 ) ) ;
#22724 = CARTESIAN_POINT ( 'NONE',  ( 804.7487373415286811, -67.54369356751125508, 364.7487373415288516 ) ) ;
#22725 = ORIENTED_EDGE ( 'NONE', *, *, #11087, .T. ) ;
#22726 = CARTESIAN_POINT ( 'NONE',  ( 781.8018195045267476, -190.2709662947835625, -365.1927285166407273 ) ) ;
#22727 = ORIENTED_EDGE ( 'NONE', *, *, #17646, .T. ) ;
#22728 = EDGE_CURVE ( 'NONE', #28192, #11754, #9074, .T. ) ;
#22729 = AXIS2_PLACEMENT_3D ( 'NONE', #19887, #34429, #3241 ) ;
#22730 = CARTESIAN_POINT ( 'NONE',  ( 754.7162404726377645, -422.7363362996975980, -339.4709603349214717 ) ) ;
#22731 = EDGE_CURVE ( 'NONE', #29779, #3603, #13684, .T. ) ;
#22732 = CARTESIAN_POINT ( 'NONE',  ( 778.1981804954714335, 13.72903370521577138, 314.8072714833589885 ) ) ;
#22733 = CARTESIAN_POINT ( 'NONE',  ( 792.3570229623688874, -261.1800572038741848, 373.1304606946836202 ) ) ;
#22734 = CARTESIAN_POINT ( 'NONE',  ( 755.8398074228967971, -163.4419599262325846, 333.4516893846970333 ) ) ;
#22737 = CARTESIAN_POINT ( 'NONE',  ( 808.7758568127978833, -412.1692326535045936, 320.0363995740631822 ) ) ;
#22736 = DIRECTION ( 'NONE',  ( -0.000000000000000000, 1.000000000000000000, -0.000000000000000000 ) ) ;
#22735 = DIRECTION ( 'NONE',  ( 0.000000000000000000, 0.000000000000000000, -1.000000000000000000 ) ) ;
#22738 = ORIENTED_EDGE ( 'NONE', *, *, #13412, .T. ) ;
#22739 = CARTESIAN_POINT ( 'NONE',  ( 801.5560724626406000, -432.5545181178793541, -326.7756240680316182 ) ) ;
#22740 = DIRECTION ( 'NONE',  ( 0.000000000000000000, 0.000000000000000000, 1.000000000000000000 ) ) ;
#22741 = CARTESIAN_POINT ( 'NONE',  ( 749.5768839229115201, -204.5545181178800931, -358.0661480581553064 ) ) ;
#22742 = CARTESIAN_POINT ( 'NONE',  ( 809.0717654672305343, -52.91815448151692891, 360.1688906516309885 ) ) ;
#22744 = CARTESIAN_POINT ( 'NONE',  ( 755.3201227861273992, -195.7255117493289731, -345.3687786644892981 ) ) ;
#22743 = CARTESIAN_POINT ( 'NONE',  ( 989.9999999999992042, 240.0000000000001990, 201.9999999999999716 ) ) ;
#22745 = CARTESIAN_POINT ( 'NONE',  ( 775.9200461376533440, -335.8055962898683902, -315.3028492785443291 ) ) ;
#22746 = LINE ( 'NONE', #43325, #27656 ) ;
#22747 = CARTESIAN_POINT ( 'NONE',  ( 776.2046728542105711, -236.1908817542436338, -304.8212110874238761 ) ) ;
#22748 = DIRECTION ( 'NONE',  ( -1.880165489482579047E-16, -1.000000000000000000, -0.000000000000000000 ) ) ;
#22749 = FACE_BOUND ( 'NONE', #7312, .T. ) ;
#22750 = CARTESIAN_POINT ( 'NONE',  ( 772.4468031744293057, -33.82724539060788516, -363.8651313633793620 ) ) ;
#22751 = CARTESIAN_POINT ( 'NONE',  ( 783.0745993439762742, -416.1908817542430938, 365.1016975059196739 ) ) ;
#22752 = CARTESIAN_POINT ( 'NONE',  ( 763.2262854647970016, -248.6346026584197659, -309.2812353651462445 ) ) ;
#22753 = CARTESIAN_POINT ( 'NONE',  ( 773.4516893846965786, -235.6454272087890729, 315.8398074228977066 ) ) ;
#22754 = DIRECTION ( 'NONE',  ( 0.7071067811865697772, 0.000000000000000000, -0.7071067811865252573 ) ) ;
#22755 = CARTESIAN_POINT ( 'NONE',  ( 765.0180583372156207, -24.99823902205683268, -360.0135310231089534 ) ) ;
#22756 = EDGE_CURVE ( 'NONE', #23583, #14164, #37016, .T. ) ;
#22757 = CARTESIAN_POINT ( 'NONE',  ( 768.9521613784389729, -177.8272453906074304, 373.2346286133773106 ) ) ;
#22758 = CARTESIAN_POINT ( 'NONE',  ( 813.9316612368132837, -127.4419599262326983, -348.6739635108323228 ) ) ;
#22759 = CARTESIAN_POINT ( 'NONE',  ( 815.2698199232961542, -136.8164208402382371, 342.5225473063383106 ) ) ;
#22760 = CARTESIAN_POINT ( 'NONE',  ( 814.5518280994195948, -375.7255117493283478, -332.4837098697145734 ) ) ;
#22761 = CARTESIAN_POINT ( 'NONE',  ( -26.63011601220122060, 26.27639943461401018, 900.0000000000001137 ) ) ;
#22762 = EDGE_CURVE ( 'NONE', #16836, #42559, #6288, .T. ) ;
#22763 = CARTESIAN_POINT ( 'NONE',  ( 762.3223304703356007, -271.5436935675106156, 322.3223304703362828 ) ) ;
#22764 = CARTESIAN_POINT ( 'NONE',  ( 787.5531968255692163, -21.82724539060792424, 316.1348686366205811 ) ) ;
#22765 = CARTESIAN_POINT ( 'NONE',  ( 788.8264449731200330, -381.1800572038737869, -363.6646147819171233 ) ) ;
#22766 = AXIS2_PLACEMENT_3D ( 'NONE', #16918, #37475, #13230 ) ;
#22767 = FACE_OUTER_BOUND ( 'NONE', #16086, .T. ) ;
#22768 = CARTESIAN_POINT ( 'NONE',  ( 797.8822607201568644, -6.554518117880697048, -370.1134526219340160 ) ) ;
#22769 = CARTESIAN_POINT ( 'NONE',  ( 879.9999999999992042, 249.9999999999998295, -199.9999999999997442 ) ) ;
#22770 = CARTESIAN_POINT ( 'NONE',  ( 805.0264073115434940, -102.3510508353236901, 339.4763451958999099 ) ) ;
#22771 = ORIENTED_EDGE ( 'NONE', *, *, #21942, .F. ) ;
#22772 = ADVANCED_FACE ( 'NONE', ( #8857 ), #34313, .F. ) ;
#22773 = CARTESIAN_POINT ( 'NONE',  ( 803.2186876482843445, -223.9874144716869182, -350.0220218866286928 ) ) ;
#22774 = CARTESIAN_POINT ( 'NONE',  ( 785.3141322388236176, -69.72551174932942786, 364.4286716492789537 ) ) ;
#22775 = CARTESIAN_POINT ( 'NONE',  ( 748.3538107759620743, -232.7146871989596377, -355.8262568251490165 ) ) ;
#22776 = CARTESIAN_POINT ( 'NONE',  ( -28.63011601220122415, -513.1383975375929367, -369.9999999999999432 ) ) ;
#22777 = CARTESIAN_POINT ( 'NONE',  ( 768.8385539511368734, -335.2601417444137724, 306.4236121716840557 ) ) ;
#22778 = ORIENTED_EDGE ( 'NONE', *, *, #9146, .T. ) ;
#22779 = CARTESIAN_POINT ( 'NONE',  ( 811.6461892240364477, -436.7146871989589272, 324.1737431748509835 ) ) ;
#22780 = CARTESIAN_POINT ( 'NONE',  ( 803.8651313633788504, -29.26014174441482751, -332.4468031744301015 ) ) ;
#22781 = CARTESIAN_POINT ( 'NONE',  ( 804.4286716492782716, -329.3618753856922581, 345.3141322388244703 ) ) ;
#22782 = CARTESIAN_POINT ( 'NONE',  ( 811.0346526505616112, -62.63460265842031305, -323.0537975583477532 ) ) ;
#22783 = CARTESIAN_POINT ( 'NONE',  ( 785.3141322388236176, -69.72551174932942786, -364.4286716492789537 ) ) ;
#22784 = EDGE_LOOP ( 'NONE', ( #7350, #23574, #32399, #13809 ) ) ;
#22785 = CARTESIAN_POINT ( 'NONE',  ( 804.1105419155481968, -27.82724539060790292, -347.6308680596136469 ) ) ;
#22786 = VERTEX_POINT ( 'NONE', #37485 ) ;
#22787 = CARTESIAN_POINT ( 'NONE',  ( 790.0220218866281812, -319.0999726633342561, -363.2186876482849129 ) ) ;
#22789 = CARTESIAN_POINT ( 'NONE',  ( 799.2566176426618085, -360.0090635724250774, 324.0069404352559559 ) ) ;
#22788 = CARTESIAN_POINT ( 'NONE',  ( 759.7806653035534055, -102.9982390220565520, 324.8639956371180801 ) ) ;
#22792 = CARTESIAN_POINT ( 'NONE',  ( 795.6651683502461765, -322.7146871989593819, 371.3240766477733814 ) ) ;
#22791 = FACE_OUTER_BOUND ( 'NONE', #32794, .T. ) ;
#22790 = CARTESIAN_POINT ( 'NONE',  ( 787.4397851343537695, -429.7255117493282910, 374.2001403089903988 ) ) ;
#22793 = CARTESIAN_POINT ( 'NONE',  ( 791.1614460488616487, -107.2601417444145824, 373.5763878283158874 ) ) ;
#22794 = CARTESIAN_POINT ( 'NONE',  ( 775.8780910478218402, -321.2817908451525000, -364.9511171171680530 ) ) ;
#22795 = CARTESIAN_POINT ( 'NONE',  ( 804.4286716492782716, -329.3618753856922581, -345.3141322388244703 ) ) ;
#22796 = CARTESIAN_POINT ( 'NONE',  ( 771.1735550268778070, -153.1800572038746395, -316.3353852180827630 ) ) ;
#22797 = CONICAL_SURFACE ( 'NONE', #29441, 8.025000000000003908, 0.7853981633974410625 ) ;
#22798 = CARTESIAN_POINT ( 'NONE',  ( 754.9967657858570647, -433.5436935675099903, 365.0032342141425374 ) ) ;
#22800 = LINE ( 'NONE', #33879, #7158 ) ;
#22799 = CARTESIAN_POINT ( 'NONE',  ( 787.0645410984409409, 17.59807796021646098, 310.5263297651933954 ) ) ;
#22801 = CARTESIAN_POINT ( 'NONE',  ( 812.3518521366052028, -121.0999726633348956, -326.5853460496235243 ) ) ;
#22802 = CARTESIAN_POINT ( 'NONE',  ( -468.8365100919714337, 240.0000000000001421, -199.9999999999908766 ) ) ;
#22803 = DIRECTION ( 'NONE',  ( 1.892425610156518354E-16, 1.000000000000000000, -0.000000000000000000 ) ) ;
#22804 = CARTESIAN_POINT ( 'NONE',  ( 801.5560724626406000, -288.5545181178798657, 326.7756240680316182 ) ) ;
#22805 = CARTESIAN_POINT ( 'NONE',  ( 804.9363028652555840, -184.2709662947835909, 338.2165204200192079 ) ) ;
#22806 = EDGE_LOOP ( 'NONE', ( #36987, #15846, #26373, #28650, #19392, #40525, #30126, #40396, #28488, #26953, #1480, #7353 ) ) ;
#22807 = CARTESIAN_POINT ( 'NONE',  ( 772.4837098697145166, -143.3618753856927697, -374.5518280994205611 ) ) ;
#22808 = FACE_OUTER_BOUND ( 'NONE', #37555, .T. ) ;
#22809 = PRODUCT_DEFINITION ( 'UNKNOWN', '', #31953, #43961 ) ;
#22810 = CARTESIAN_POINT ( 'NONE',  ( 757.7880784355613741, -90.00906357242590161, 312.4576283171834916 ) ) ;
#22811 = CARTESIAN_POINT ( 'NONE',  ( 777.5031285880264704, -286.8164208402378677, -374.9108240113588408 ) ) ;
#22812 = CARTESIAN_POINT ( 'NONE',  ( 795.1271208383658404, -452.8379544210779954, -371.6178728169206238 ) ) ;
#22813 = CARTESIAN_POINT ( 'NONE',  ( 797.6776695296629214, -139.5436935675110135, 357.6776695296636603 ) ) ;
#22814 = CARTESIAN_POINT ( 'NONE',  ( 761.9338519418445230, -350.5328690171411381, -370.4231160770881957 ) ) ;
#22815 = CARTESIAN_POINT ( 'NONE',  ( 800.9747183278959710, -84.99823902205663728, -311.9810565676471583 ) ) ;
#22816 = CARTESIAN_POINT ( 'NONE',  ( 783.0745993439762742, -32.19088175424425913, 365.1016975059196739 ) ) ;
#22817 = CARTESIAN_POINT ( 'NONE',  ( 754.9967657858570647, -337.5436935675102177, -365.0032342141425374 ) ) ;
#22818 = DIRECTION ( 'NONE',  ( 1.000000000000000000, 0.000000000000000000, -0.000000000000000000 ) ) ;
#22819 = CARTESIAN_POINT ( 'NONE',  ( 770.0799878456142551, -397.9874144716864066, 362.9823548866085616 ) ) ;
#22820 = ORIENTED_EDGE ( 'NONE', *, *, #2106, .T. ) ;
#22821 = CARTESIAN_POINT ( 'NONE',  ( 812.6845335610512393, -127.9874144716872308, -353.5525998758768651 ) ) ;
#22822 = LINE ( 'NONE', #6645, #22569 ) ;
#22823 = CARTESIAN_POINT ( 'NONE',  ( 807.5423716828161105, -225.0783235625959833, 362.2119215644372048 ) ) ;
#22824 = CARTESIAN_POINT ( 'NONE',  ( 804.6798772138710092, -87.72551174932935680, 334.6312213355106451 ) ) ;
#22825 = VECTOR ( 'NONE', #10022, 1000.000000000000114 ) ;
#22826 = VERTEX_POINT ( 'NONE', #19703 ) ;
#22827 = CARTESIAN_POINT ( 'NONE',  ( 754.9735926884551418, -234.3510508353232638, -340.5236548041000333 ) ) ;
#22828 = CARTESIAN_POINT ( 'NONE',  ( 771.1735550268778070, -225.1800572038743269, 316.3353852180827630 ) ) ;
#22829 = CARTESIAN_POINT ( 'NONE',  ( 795.6651683502461765, -442.7146871989589840, -371.3240766477733814 ) ) ;
#22830 = CARTESIAN_POINT ( 'NONE',  ( 812.6845335610512393, -55.98741447168748664, -353.5525998758768651 ) ) ;
#22831 = FACE_OUTER_BOUND ( 'NONE', #29095, .T. ) ;
#22832 = ORIENTED_EDGE ( 'NONE', *, *, #24269, .F. ) ;
#22833 = VERTEX_POINT ( 'NONE', #40289 ) ;
#22834 = CARTESIAN_POINT ( 'NONE',  ( 797.8822607201568644, -366.5545181178795815, -370.1134526219340160 ) ) ;
#22835 = CARTESIAN_POINT ( 'NONE',  ( 804.6798772138708955, -231.7255117493288310, -334.6312213355107019 ) ) ;
#22836 = CARTESIAN_POINT ( 'NONE',  ( 745.4481719005789273, -339.7255117493285184, 347.5162901302853697 ) ) ;
#22837 = CARTESIAN_POINT ( 'NONE',  ( 745.1769319972822814, -17.80559628986940979, 346.2694204179732083 ) ) ;
#22838 = APPLICATION_CONTEXT ( 'automotive_design' ) ;
#22839 = CARTESIAN_POINT ( 'NONE',  ( 766.0291762391763086, -226.9181544815163534, -360.7704444035551319 ) ) ;
#22840 = CARTESIAN_POINT ( 'NONE',  ( 804.9363028652555840, -208.2709662947835341, -338.2165204200192079 ) ) ;
#22841 = CARTESIAN_POINT ( 'NONE',  ( 774.6312213355098493, -383.3618753856920875, -364.6798772138717482 ) ) ;
#22842 = VERTEX_POINT ( 'NONE', #4940 ) ;
#22843 = CARTESIAN_POINT ( 'NONE',  ( 771.2633955100217236, -215.9073299311471317, 363.4237431249939618 ) ) ;
#22844 = CARTESIAN_POINT ( 'NONE',  ( 800.2193346964447755, -114.9982390220565236, -355.1360043628815788 ) ) ;
#22845 = ORIENTED_EDGE ( 'NONE', *, *, #17041, .T. ) ;
#22846 = CARTESIAN_POINT ( 'NONE',  ( 755.2512626584698410, -319.5436935675104451, 315.2512626584710915 ) ) ;
#22847 = LINE ( 'NONE', #5293, #39591 ) ;
#22848 = FACE_BOUND ( 'NONE', #18600, .T. ) ;
#22849 = PLANE ( 'NONE',  #26075 ) ;
#22850 = CARTESIAN_POINT ( 'NONE',  ( 755.8894580844503253, -183.8272453906074020, 332.3691319403863531 ) ) ;
#22851 = CARTESIAN_POINT ( 'NONE',  ( 797.8594530101008786, -85.54369356751118403, 322.1405469898980982 ) ) ;
#22852 = VERTEX_POINT ( 'NONE', #40049 ) ;
#22853 = CARTESIAN_POINT ( 'NONE',  ( 814.4686193811664907, -459.2817908451519884, -346.2056067578752732 ) ) ;
#22854 = CARTESIAN_POINT ( 'NONE',  ( 796.7737145352015204, -20.63460265842048003, -370.7187646348536987 ) ) ;
#22855 = CARTESIAN_POINT ( 'NONE',  ( 754.9735926884551418, -258.3510508353231785, 340.5236548041000333 ) ) ;
#22856 = CARTESIAN_POINT ( 'NONE',  ( 774.6858677611749044, -393.7255117493283478, -315.5713283507209894 ) ) ;
#22857 = CARTESIAN_POINT ( 'NONE',  ( 800.0135310231082713, -14.08914811296595460, -325.0180583372163028 ) ) ;
#22858 = CARTESIAN_POINT ( 'NONE',  ( 746.8695393053150156, -437.9073299311463074, 327.6429770376306010 ) ) ;
#22859 = CARTESIAN_POINT ( 'NONE',  ( 773.4999999999993179, -494.6608068873671300, -357.6536686473015720 ) ) ;
#22860 = CARTESIAN_POINT ( 'NONE',  ( 755.1538015810308480, -278.1908817542434917, -343.0433043558613804 ) ) ;
#22861 = CARTESIAN_POINT ( 'NONE',  ( 808.0189434323515343, -182.0891481129654323, -319.0252816721025511 ) ) ;
#22862 = CARTESIAN_POINT ( 'NONE',  ( 767.6429770376289525, -57.18005720387489532, 306.8695393053162093 ) ) ;
#22863 = CARTESIAN_POINT ( 'NONE',  ( 787.5162901302840055, -131.3618753856928834, 305.4481719005792684 ) ) ;
#22864 = CARTESIAN_POINT ( 'NONE',  ( 939.9999999999993179, 62.79977829742944095, 207.3621835540873235 ) ) ;
#22865 = EDGE_CURVE ( 'NONE', #811, #8509, #19464, .T. ) ;
#22866 = CARTESIAN_POINT ( 'NONE',  ( 799.9999999999993179, 205.0000000000000568, -265.0000000000000000 ) ) ;
#22867 = LINE ( 'NONE', #1844, #32416 ) ;
#22868 = CARTESIAN_POINT ( 'NONE',  ( 748.9653473494363425, -362.6346026584194533, 356.9462024416521331 ) ) ;
#22869 = CARTESIAN_POINT ( 'NONE',  ( 801.9419747391806368, -330.4527844766013231, -351.9812246680014027 ) ) ;
#22870 = CARTESIAN_POINT ( 'NONE',  ( 797.6776695296629214, -451.5436935675099903, 357.6776695296636603 ) ) ;
#22871 = CARTESIAN_POINT ( 'NONE',  ( 802.2119215644370342, -102.0090635724258448, -367.5423716828165084 ) ) ;
#22872 = CARTESIAN_POINT ( 'NONE',  ( 773.3843516231979720, -133.4419599262326699, -364.4086373105754433 ) ) ;
#22873 = B_SPLINE_CURVE_WITH_KNOTS ( 'NONE', 3,
 ( #1402, #39992, #26777, #5778, #1619, #36739, #15718, #2076, #43442, #40444, #15506, #8796, #29586, #9009, #19634, #23317, #12479, #29804, #36957, #40656, #26102, #37421, #43883, #8340, #40883, #15949, #23079, #33729, #19864, #9247, #30031, #4870, #37178, #33273, #43662, #12260 ),
 .UNSPECIFIED., .F., .F.,
 ( 4, 2, 2, 2, 2, 2, 2, 2, 2, 2, 2, 2, 2, 2, 2, 2, 2, 4 ),
 ( 0.000000000000000000, 0.004405609005296106002, 0.008811218010592212005, 0.01101402251324022814, 0.01321682701588824428, 0.01762243602118459054, 0.01982524052383277668, 0.02202804502648095936, 0.02643365403177701245, 0.02863645853442487593, 0.03083926303707274288, 0.03194066528839652197, 0.03304206753972029759, 0.03359276866538235540, 0.03414346979104441321, 0.03469417091670646408, 0.03496952147953734380, 0.03524487204236821658 ),
 .UNSPECIFIED. ) ;
#22874 = CARTESIAN_POINT ( 'NONE',  ( 764.3348316497523456, -142.7146871989599219, 308.6759233522265617 ) ) ;
#22875 = FACE_OUTER_BOUND ( 'NONE', #14171, .T. ) ;
#22876 = CARTESIAN_POINT ( 'NONE',  ( 771.2633955100217236, -23.90732993114773919, -363.4237431249939618 ) ) ;
#22877 = CARTESIAN_POINT ( 'NONE',  ( 803.2186876482843445, -127.9874144716872308, -350.0220218866286928 ) ) ;
#22878 = CARTESIAN_POINT ( 'NONE',  ( 764.8639956371174549, -128.0891481129655176, -319.7806653035542013 ) ) ;
#22879 = CARTESIAN_POINT ( 'NONE',  ( 803.6646147819161570, -137.9073299311473875, 348.8264449731210561 ) ) ;
#22880 = CARTESIAN_POINT ( 'NONE',  ( 764.3348316497523456, 25.28531280103955226, -308.6759233522265617 ) ) ;
#22881 = EDGE_CURVE ( 'NONE', #5961, #39395, #1908, .T. ) ;
#22883 = CARTESIAN_POINT ( 'NONE',  ( 804.4286716492782716, -257.3618753856924286, 345.3141322388244703 ) ) ;
#22882 = CARTESIAN_POINT ( 'NONE',  ( 754.8072714833581358, -268.8164208402378108, 338.1981804954720587 ) ) ;
#22884 = CARTESIAN_POINT ( 'NONE',  ( -468.8365100919714337, 260.0000000000001705, -197.2499999999910187 ) ) ;
#22885 = VERTEX_POINT ( 'NONE', #26618 ) ;
#22886 = CARTESIAN_POINT ( 'NONE',  ( 804.4286716492782716, -449.3618753856918602, 345.3141322388244703 ) ) ;
#22887 = CARTESIAN_POINT ( 'NONE',  ( 814.8207195650702488, -290.1908817542434349, -336.2433038121456548 ) ) ;
#22888 = ORIENTED_EDGE ( 'NONE', *, *, #7510, .T. ) ;
#22889 = CARTESIAN_POINT ( 'NONE',  ( 782.5225473063383106, -214.2709662947834772, 375.2698199232970637 ) ) ;
#22890 = CARTESIAN_POINT ( 'NONE',  ( 775.8780910478218402, -297.2817908451526137, 364.9511171171680530 ) ) ;
#22891 = CARTESIAN_POINT ( 'NONE',  ( 754.9735926884551418, -402.3510508353228374, 340.5236548041000333 ) ) ;
#22892 = ORIENTED_EDGE ( 'NONE', *, *, #38314, .F. ) ;
#22893 = CARTESIAN_POINT ( 'NONE',  ( 769.9779781133707957, -115.0999726633348956, -316.7813123517150871 ) ) ;
#22894 = CARTESIAN_POINT ( 'NONE',  ( 756.5762568750052424, -267.1800572038742985, -348.7366044899774238 ) ) ;
#22895 = EDGE_LOOP ( 'NONE', ( #43498, #4672, #16029, #34018 ) ) ;
#22896 = CARTESIAN_POINT ( 'NONE',  ( 791.9812246680005501, -428.6346026584192259, -361.9419747391813189 ) ) ;
#22897 = CARTESIAN_POINT ( 'NONE',  ( 754.8072714833581358, -76.81642084023845030, -338.1981804954720587 ) ) ;
#22898 = CARTESIAN_POINT ( 'NONE',  ( 757.2208543904082489, -280.7146871989594956, 350.9844846989624330 ) ) ;
#22899 = CARTESIAN_POINT ( 'NONE',  ( 919.9999999999993179, 154.9999999999998863, -359.9749999999999659 ) ) ;
#22900 = CARTESIAN_POINT ( 'NONE',  ( 311.1634899080286232, 260.0000000000000000, -197.2499999999964473 ) ) ;
#22901 = CARTESIAN_POINT ( 'NONE',  ( 771.3260364891663130, -19.64542720878974791, -306.0683387631859773 ) ) ;
#22902 = CARTESIAN_POINT ( 'NONE',  ( 802.1676090361156639, 9.365397341579420498, 327.8955696845344505 ) ) ;
#22903 = EDGE_LOOP ( 'NONE', ( #11668, #25637, #40066, #36053, #644, #29653, #14396, #41080 ) ) ;
#22904 = CARTESIAN_POINT ( 'NONE',  ( 783.7953271457878373, -344.1908817542433212, -375.1787889125761239 ) ) ;
#22905 = CARTESIAN_POINT ( 'NONE',  ( 755.8990559732751535, -203.4636090269709996, 365.9055244015606831 ) ) ;
#22907 = CARTESIAN_POINT ( 'NONE',  ( 755.3201227861273992, -291.7255117493285752, -345.3687786644892981 ) ) ;
#22906 = DIRECTION ( 'NONE',  ( 0.000000000000000000, -1.000000000000000000, 0.000000000000000000 ) ) ;
#22908 = DIRECTION ( 'NONE',  ( -1.000000000000000000, -0.000000000000000000, 0.000000000000000000 ) ) ;
#22909 = CARTESIAN_POINT ( 'NONE',  ( 754.7162404726377645, -158.7363362996984222, -339.4709603349214717 ) ) ;
#22910 = ADVANCED_FACE ( 'NONE', ( #22706, #9312, #5846 ), #32901, .F. ) ;
#22911 = CARTESIAN_POINT ( 'NONE',  ( 758.8095938919642549, -56.08914811296580893, 311.6929314249763365 ) ) ;
#22912 = CARTESIAN_POINT ( 'NONE',  ( 959.5497976682736407, 239.9999999999998863, 350.0000000000000000 ) ) ;
#22913 = CARTESIAN_POINT ( 'NONE',  ( 759.0252816721024374, -336.9982390220558273, -368.0189434323527280 ) ) ;
#22914 = CARTESIAN_POINT ( 'NONE',  ( -773.4999999999993179, 26.27639943461401018, 900.0000000000001137 ) ) ;
#22915 = CARTESIAN_POINT ( 'NONE',  ( 762.1405469898971887, -49.54369356751129061, 357.8594530101015607 ) ) ;
#22916 = CARTESIAN_POINT ( 'NONE',  ( 778.7629533639073998, -272.7363362996981095, 375.0009284576466371 ) ) ;
#22917 = CARTESIAN_POINT ( 'NONE',  ( 745.7998596910086917, -269.3618753856924286, 332.5602148656461168 ) ) ;
#22918 = CARTESIAN_POINT ( 'NONE',  ( 772.4837098697144029, 0.6381246143067236254, -374.5518280994205611 ) ) ;
#22919 = FACE_OUTER_BOUND ( 'NONE', #8978, .T. ) ;
#22920 = LINE ( 'NONE', #5603, #13629 ) ;
#22921 = CARTESIAN_POINT ( 'NONE',  ( 756.5762568750052424, -363.1800572038739006, 348.7366044899774238 ) ) ;
#22922 = CARTESIAN_POINT ( 'NONE',  ( 787.5531968255692163, -117.8272453906076151, 316.1348686366205811 ) ) ;
#22923 = CARTESIAN_POINT ( 'NONE',  ( 805.1016975059191054, -6.896505380778533478, -343.0745993439771837 ) ) ;
#22924 = DIRECTION ( 'NONE',  ( 0.000000000000000000, -1.000000000000000000, 0.000000000000000000 ) ) ;
#22925 = LINE ( 'NONE', #37017, #26236 ) ;
#22926 = CARTESIAN_POINT ( 'NONE',  ( 788.8264449731200330, -405.1800572038737300, 363.6646147819171233 ) ) ;
#22927 = ORIENTED_EDGE ( 'NONE', *, *, #22626, .T. ) ;
#22928 = CARTESIAN_POINT ( 'NONE',  ( 798.7617431975189675, -339.6237781080502600, -323.0428371773161871 ) ) ;
#22930 = CARTESIAN_POINT ( 'NONE',  ( 759.7806653035535192, -150.9982390220564241, 324.8639956371181370 ) ) ;
#22929 = CARTESIAN_POINT ( 'NONE',  ( 778.2165204200184689, -142.8164208402382656, 364.9363028652563230 ) ) ;
#22931 = CARTESIAN_POINT ( 'NONE',  ( 798.0661480581538854, -314.5328690171411949, -309.5768839229118043 ) ) ;
#22932 = DIRECTION ( 'NONE',  ( 0.000000000000000000, 0.000000000000000000, 1.000000000000000000 ) ) ;
#22933 = ORIENTED_EDGE ( 'NONE', *, *, #27840, .F. ) ;
#22934 = CARTESIAN_POINT ( 'NONE',  ( 758.0580252608178853, -342.4527844766013231, 328.0187753319985404 ) ) ;
#22935 = VERTEX_POINT ( 'NONE', #19932 ) ;
#22936 = CARTESIAN_POINT ( 'NONE',  ( 758.8095938919642549, -176.0891481129653755, -311.6929314249763365 ) ) ;
#22937 = CARTESIAN_POINT ( 'NONE',  ( 815.2698199232962679, -112.8164208402383650, 342.5225473063383674 ) ) ;
#22938 = VERTEX_POINT ( 'NONE', #10217 ) ;
#22939 = CARTESIAN_POINT ( 'NONE',  ( 771.2633955100217236, -191.9073299311471885, -363.4237431249939618 ) ) ;
#22940 = ORIENTED_EDGE ( 'NONE', *, *, #22696, .T. ) ;
#22941 = CARTESIAN_POINT ( 'NONE',  ( 802.1676090361156639, 9.365397341579420498, -327.8955696845344505 ) ) ;
#22942 = CARTESIAN_POINT ( 'NONE',  ( 813.1304606946830518, -257.9073299311469896, 352.3570229623690580 ) ) ;
#22943 = CARTESIAN_POINT ( 'NONE',  ( 787.6308680596127942, -155.2601417444144261, 364.1105419155492768 ) ) ;
#22945 = FACE_OUTER_BOUND ( 'NONE', #205, .T. ) ;
#22944 = FACE_OUTER_BOUND ( 'NONE', #15272, .T. ) ;
#22946 = EDGE_CURVE ( 'NONE', #32451, #40161, #45572, .T. ) ;
#22947 = EDGE_LOOP ( 'NONE', ( #37721, #18805 ) ) ;
#22948 = CARTESIAN_POINT ( 'NONE',  ( 754.7162404726377645, -422.7363362996975980, -339.4709603349214717 ) ) ;
#22949 = CARTESIAN_POINT ( 'NONE',  ( -879.9999999999992042, 260.0000000000002274, -179.9999999999999716 ) ) ;
#22950 = ORIENTED_EDGE ( 'NONE', *, *, #25197, .F. ) ;
#22951 = CARTESIAN_POINT ( 'NONE',  ( 799.9636004259356241, -190.9181544815164955, -311.2241431872006956 ) ) ;
#22952 = CARTESIAN_POINT ( 'NONE',  ( 781.2370466360911223, -116.7363362996985217, 304.9990715423533629 ) ) ;
#22954 = CARTESIAN_POINT ( 'NONE',  ( 785.3687786644884454, -179.3618753856927128, -315.3201227861279676 ) ) ;
#22953 = DIRECTION ( 'NONE',  ( 0.000000000000000000, -1.000000000000000000, -1.672022627447524993E-16 ) ) ;
#22955 = CARTESIAN_POINT ( 'NONE',  ( 779.4709603349208464, -360.3510508353228374, -314.7162404726379918 ) ) ;
#22956 = DIRECTION ( 'NONE',  ( -1.000000000000000000, -0.000000000000000000, -0.000000000000000000 ) ) ;
#22957 = CARTESIAN_POINT ( 'NONE',  ( 811.3240766477731540, -220.3726999360618208, -355.6651683502462902 ) ) ;
#22958 = CARTESIAN_POINT ( 'NONE',  ( 787.4999999999992042, -462.9681489794447771, 310.9526249034443026 ) ) ;
#22960 = EDGE_CURVE ( 'NONE', #31811, #12219, #16929, .T. ) ;
#22959 = CARTESIAN_POINT ( 'NONE',  ( 939.9999999999993179, -600.0000000000001137, 350.0000000000000000 ) ) ;
#22961 = CARTESIAN_POINT ( 'NONE',  ( 757.0176451133909268, -61.09997266333506616, -349.9200121543848354 ) ) ;
#22962 = EDGE_CURVE ( 'NONE', #26734, #32683, #34926, .T. ) ;
#22963 = CARTESIAN_POINT ( 'NONE',  ( 801.5560724626406000, -432.5545181178793541, 326.7756240680316182 ) ) ;
#22964 = CARTESIAN_POINT ( 'NONE',  ( 808.0189434323515343, -230.0891481129652618, -319.0252816721025511 ) ) ;
#22965 = CARTESIAN_POINT ( 'NONE',  ( 804.1105419155481968, -243.8272453906072030, 347.6308680596136469 ) ) ;
#22966 = CARTESIAN_POINT ( 'NONE',  ( 1238.921997096861332, 430.0000000000002842, -244.9999999999999716 ) ) ;
#22967 = PLANE ( 'NONE',  #19450 ) ;
#22968 = CARTESIAN_POINT ( 'NONE',  ( 771.1735550268778070, -33.18005720387498769, -316.3353852180827630 ) ) ;
#22969 = CARTESIAN_POINT ( 'NONE',  ( 805.6418435158337843, -197.4636090269709996, 363.8556311672236916 ) ) ;
#22970 = CARTESIAN_POINT ( 'NONE',  ( 761.9338519418445230, -134.5328690171417350, -370.4231160770881957 ) ) ;
#22971 = CARTESIAN_POINT ( 'NONE',  ( 745.4481719005789273, -147.7255117493291152, 347.5162901302853129 ) ) ;
#22972 = CARTESIAN_POINT ( 'NONE',  ( 813.1304606946830518, -377.9073299311466485, -352.3570229623690580 ) ) ;
#22973 = DIRECTION ( 'NONE',  ( 0.000000000000000000, 0.000000000000000000, 1.000000000000000000 ) ) ;
#22974 = CARTESIAN_POINT ( 'NONE',  ( 774.6312213355099630, -239.3618753856924570, 364.6798772138717482 ) ) ;
#22975 = CARTESIAN_POINT ( 'NONE',  ( 769.0155153010367712, -34.37269993606243901, 362.7791456095907279 ) ) ;
#22976 = EDGE_CURVE ( 'NONE', #12562, #15121, #21062, .T. ) ;
#22977 = CARTESIAN_POINT ( 'NONE',  ( 791.9812246680005501, -404.6346026584193396, -361.9419747391813189 ) ) ;
#22978 = CARTESIAN_POINT ( 'NONE',  ( -786.4999999999993179, -494.6608068873671300, -357.6536686473015720 ) ) ;
#22979 = CARTESIAN_POINT ( 'NONE',  ( 814.4686193811664907, -3.281790845153435221, -346.2056067578752732 ) ) ;
#22981 = EDGE_CURVE ( 'NONE', #34173, #22008, #30543, .T. ) ;
#22980 = CARTESIAN_POINT ( 'NONE',  ( 759.2380499001254748, 21.41625977839825978, -318.3449445151863415 ) ) ;
#22982 = CARTESIAN_POINT ( 'NONE',  ( 755.8398074228967971, -91.44195992623282621, 333.4516893846970333 ) ) ;
#22983 = ORIENTED_EDGE ( 'NONE', *, *, #22960, .T. ) ;
#22984 = CARTESIAN_POINT ( 'NONE',  ( 755.0488828828309806, -209.8055962898687881, -344.1219089521771934 ) ) ;
#22985 = EDGE_CURVE ( 'NONE', #16350, #31813, #6295, .T. ) ;
#22986 = CARTESIAN_POINT ( 'NONE',  ( 757.8323909638827445, -50.63460265842036989, 352.1044303154654358 ) ) ;
#22987 = CARTESIAN_POINT ( 'NONE',  ( 751.2241431872005251, -208.1692326535051905, -359.9636004259367610 ) ) ;
#22988 = SURFACE_STYLE_FILL_AREA ( #34073 ) ;
#22989 = CARTESIAN_POINT ( 'NONE',  ( 813.9316612368132837, -367.4419599262319025, 348.6739635108323228 ) ) ;
#22990 = ORIENTED_EDGE ( 'NONE', *, *, #43102, .T. ) ;
#22991 = CARTESIAN_POINT ( 'NONE',  ( 815.1787889125755555, -438.8965053807771710, 343.7953271457877804 ) ) ;
#22992 = CARTESIAN_POINT ( 'NONE',  ( 792.1044303154645831, -180.4527844766017211, -317.8323909638837677 ) ) ;
#22993 = CARTESIAN_POINT ( 'NONE',  ( 765.0180583372156207, -360.9982390220557704, 360.0135310231089534 ) ) ;
#22994 = CARTESIAN_POINT ( 'NONE',  ( 745.4481719005789273, -75.72551174932937101, -347.5162901302853129 ) ) ;
#22995 = CARTESIAN_POINT ( 'NONE',  ( 804.9363028652555840, -88.27096629478390355, -338.2165204200192079 ) ) ;
#22996 = ORIENTED_EDGE ( 'NONE', *, *, #37891, .F. ) ;
#22997 = CARTESIAN_POINT ( 'NONE',  ( 804.8461984189677878, -26.19088175424427334, -336.9566956441385628 ) ) ;
#22998 = ORIENTED_EDGE ( 'NONE', *, *, #2759, .T. ) ;
#22999 = CARTESIAN_POINT ( 'NONE',  ( 796.9571628226829034, -335.4636090269705733, -321.2382568024804641 ) ) ;
#23000 = EDGE_CURVE ( 'NONE', #24825, #40516, #44645, .T. ) ;
#23002 = CARTESIAN_POINT ( 'NONE',  ( 763.0428371773158460, -395.4636090269705164, 358.7617431975195359 ) ) ;
#23001 = CARTESIAN_POINT ( 'NONE',  ( 804.6798772138708955, -87.72551174932937101, 334.6312213355107019 ) ) ;
#23005 = CARTESIAN_POINT ( 'NONE',  ( 764.3348316497523456, -334.7146871989593251, 308.6759233522265617 ) ) ;
#23004 = DIRECTION ( 'NONE',  ( -0.000000000000000000, 1.000000000000000000, -0.000000000000000000 ) ) ;
#23003 = CARTESIAN_POINT ( 'NONE',  ( 777.4774526936600978, -442.2709662947827383, 304.7301800767028226 ) ) ;
#23006 = ADVANCED_FACE ( 'NONE', ( #13692 ), #27771, .T. ) ;
#23007 = CARTESIAN_POINT ( 'NONE',  ( 783.0745993439762742, -320.1908817542434349, -365.1016975059196739 ) ) ;
#23008 = CARTESIAN_POINT ( 'NONE',  ( 774.6858677611749044, -321.7255117493286320, -315.5713283507209894 ) ) ;
#23009 = CARTESIAN_POINT ( 'NONE',  ( 778.1981804954714335, -154.2709662947836478, -314.8072714833589885 ) ) ;
#23010 = CARTESIAN_POINT ( 'NONE',  ( 788.6739635108323228, -7.645427208789786100, 373.9316612368139090 ) ) ;
#23012 = LINE ( 'NONE', #37106, #41806 ) ;
#23011 = CARTESIAN_POINT ( 'NONE',  ( 769.9999999999992042, 205.0000000000000568, -360.0000000000000000 ) ) ;
#23013 = CARTESIAN_POINT ( 'NONE',  ( 745.7194118038753459, -133.6454272087893571, -348.7631598425976449 ) ) ;
#23014 = LINE ( 'NONE', #9169, #29319 ) ;
#23016 = EDGE_CURVE ( 'NONE', #33397, #9428, #10441, .T. ) ;
#23015 = CARTESIAN_POINT ( 'NONE',  ( 794.9999999999993179, 205.0000000000000568, 255.0000000000000000 ) ) ;
#23017 = ADVANCED_FACE ( 'NONE', ( #2601 ), #20380, .T. ) ;
#23018 = CARTESIAN_POINT ( 'NONE',  ( 755.5913626894240451, -301.6454272087889308, 346.6156483768012890 ) ) ;
#23019 = ORIENTED_EDGE ( 'NONE', *, *, #41912, .T. ) ;
#23020 = CARTESIAN_POINT ( 'NONE',  ( 768.9521613784389729, -273.8272453906071746, 373.2346286133773106 ) ) ;
#23021 = CIRCLE ( 'NONE', #34071, 9.999999999999982236 ) ;
#23022 = CARTESIAN_POINT ( 'NONE',  ( 763.2262854647970016, -152.6346026584200786, -309.2812353651462445 ) ) ;
#23023 = LINE ( 'NONE', #15883, #44520 ) ;
#23024 = CARTESIAN_POINT ( 'NONE',  ( 781.2370466360911223, -92.73633629969860692, 304.9990715423533629 ) ) ;
#23025 = CARTESIAN_POINT ( 'NONE',  ( 792.2312462859673587, -275.9073299311469896, -307.2067596250082602 ) ) ;
#23026 = FACE_OUTER_BOUND ( 'NONE', #6311, .T. ) ;
#23027 = CARTESIAN_POINT ( 'NONE',  ( 764.8639956371174549, -152.0891481129655460, 319.7806653035542013 ) ) ;
#23028 = VERTEX_POINT ( 'NONE', #24516 ) ;
#23029 = CARTESIAN_POINT ( 'NONE',  ( 764.3348316497523456, -334.7146871989593251, -308.6759233522265617 ) ) ;
#23030 = CARTESIAN_POINT ( 'NONE',  ( 808.0189434323515343, -86.08914811296573077, -319.0252816721025511 ) ) ;
#23031 = CARTESIAN_POINT ( 'NONE',  ( 779.4763451958990572, -32.73633629969879877, 365.0264073115438919 ) ) ;
#23032 = CARTESIAN_POINT ( 'NONE',  ( 746.8695393053150156, -365.9073299311465917, -327.6429770376306010 ) ) ;
#23033 = FACE_OUTER_BOUND ( 'NONE', #36718, .T. ) ;
#23034 = CARTESIAN_POINT ( 'NONE',  ( 783.0433043558608688, -432.8965053807771142, 315.1538015810313027 ) ) ;
#23035 = ORIENTED_EDGE ( 'NONE', *, *, #42173, .F. ) ;
#23036 = CIRCLE ( 'NONE', #3143, 9.999999999999982236 ) ;
#23037 = CARTESIAN_POINT ( 'NONE',  ( 776.2433038121456548, -132.8965053807781374, -374.8207195650711014 ) ) ;
#23038 = CARTESIAN_POINT ( 'NONE',  ( 571.1634899080285095, 259.9999999999999432, -199.9999999999981526 ) ) ;
#23039 = CARTESIAN_POINT ( 'NONE',  ( 745.1769319972822814, -233.8055962898687028, 346.2694204179732083 ) ) ;
#23040 = ORIENTED_EDGE ( 'NONE', *, *, #25157, .F. ) ;
#23041 = CARTESIAN_POINT ( 'NONE',  ( 766.7756240680305382, -14.53286901714214707, -361.5560724626415663 ) ) ;
#23042 = CARTESIAN_POINT ( 'NONE',  ( 797.6776695296629214, -283.5436935675105019, 357.6776695296636603 ) ) ;
#23043 = CARTESIAN_POINT ( 'NONE',  ( 786.2056067578752163, -419.8055962898681059, -374.4686193811670023 ) ) ;
#23044 = DIRECTION ( 'NONE',  ( 8.659560562354807133E-17, 0.7071067811865578978, -0.7071067811865372477 ) ) ;
#23045 = ORIENTED_EDGE ( 'NONE', *, *, #25473, .F. ) ;
#23046 = ORIENTED_EDGE ( 'NONE', *, *, #39154, .F. ) ;
#23047 = CARTESIAN_POINT ( 'NONE',  ( 768.9521613784389729, -369.8272453906068904, -373.2346286133773106 ) ) ;
#23048 = EDGE_CURVE ( 'NONE', #44849, #39281, #6059, .T. ) ;
#23049 = CARTESIAN_POINT ( 'NONE',  ( 757.8323909638827445, -242.6346026584197659, -352.1044303154654358 ) ) ;
#23050 = CARTESIAN_POINT ( 'NONE',  ( 796.7737145352015204, -332.6346026584195101, 370.7187646348536987 ) ) ;
#23051 = CARTESIAN_POINT ( 'NONE',  ( 781.2497674668890113, -36.35105083532390324, 375.3608509340180603 ) ) ;
#23052 = CARTESIAN_POINT ( 'NONE',  ( 773.4516893846965786, -211.6454272087891582, -315.8398074228977066 ) ) ;
#23053 = CARTESIAN_POINT ( 'NONE',  ( 803.6646147819161570, -209.9073299311470748, -348.8264449731210561 ) ) ;
#23054 = CARTESIAN_POINT ( 'NONE',  ( 758.0580252608178853, -414.4527844766010389, -328.0187753319985404 ) ) ;
#23055 = ORIENTED_EDGE ( 'NONE', *, *, #14023, .T. ) ;
#23056 = CARTESIAN_POINT ( 'NONE',  ( 800.0135310231082713, -206.0891481129653471, 325.0180583372163028 ) ) ;
#23057 = CARTESIAN_POINT ( 'NONE',  ( 791.9812246680005501, -92.63460265842026331, -361.9419747391813189 ) ) ;
#23058 = VERTEX_POINT ( 'NONE', #41874 ) ;
#23059 = CARTESIAN_POINT ( 'NONE',  ( 744.7301800767019131, -340.8164208402376971, 337.4774526936615757 ) ) ;
#23060 = CARTESIAN_POINT ( 'NONE',  ( 767.9999999999992042, 178.9475563372491251, -360.0000000000000000 ) ) ;
#23061 = CARTESIAN_POINT ( 'NONE',  ( 939.9999999999992042, 74.99999999999984368, -350.0000000000000000 ) ) ;
#23062 = DIRECTION ( 'NONE',  ( 0.000000000000000000, -0.6438296778008192334, 0.7651688349527138167 ) ) ;
#23063 = CARTESIAN_POINT ( 'NONE',  ( 761.4292242960306112, -209.4636090269709996, 323.2154366446414429 ) ) ;
#23064 = CARTESIAN_POINT ( 'NONE',  ( 788.8264449731200330, -93.18005720387481006, 363.6646147819171233 ) ) ;
#23065 = ORIENTED_EDGE ( 'NONE', *, *, #5182, .F. ) ;
#23066 = CARTESIAN_POINT ( 'NONE',  ( 797.8822607201568644, -462.5545181178792973, -370.1134526219340160 ) ) ;
#23067 = CIRCLE ( 'NONE', #14231, 4.999999999999982236 ) ;
#23068 = CARTESIAN_POINT ( 'NONE',  ( 777.5031285880264704, -22.81642084023865280, -374.9108240113588408 ) ) ;
#23069 = PRODUCT_DEFINITION_FORMATION_WITH_SPECIFIED_SOURCE ( 'ANY', '', #2245, .NOT_KNOWN. ) ;
#23070 = CARTESIAN_POINT ( 'NONE',  ( 803.8651313633788504, -269.2601417444139997, 332.4468031744301015 ) ) ;
#23071 = CARTESIAN_POINT ( 'NONE',  ( 802.1676090361156639, -398.6346026584193396, -327.8955696845344505 ) ) ;
#23072 = CARTESIAN_POINT ( 'NONE',  ( 803.6646147819162707, 6.092670068852160448, -348.8264449731211130 ) ) ;
#23073 = CARTESIAN_POINT ( 'NONE',  ( 747.2067596250078623, -435.1800572038737869, 352.2312462859687230 ) ) ;
#23074 = LINE ( 'NONE', #4865, #29856 ) ;
#23075 = CARTESIAN_POINT ( 'NONE',  ( 754.7162404726377645, -302.7363362996979959, -339.4709603349214717 ) ) ;
#23076 = CARTESIAN_POINT ( 'NONE',  ( 755.2512626584698410, -175.5436935675108998, -315.2512626584710915 ) ) ;
#23077 = CARTESIAN_POINT ( 'NONE',  ( 813.1304606946830518, -89.90732993114750116, 352.3570229623690580 ) ) ;
#23078 = CARTESIAN_POINT ( 'NONE',  ( 808.3070685750230950, -138.9982390220563957, 361.1904061080339261 ) ) ;
#23079 = CARTESIAN_POINT ( 'NONE',  ( 793.5727445751998630, 16.45630643248830793, -314.6726781324130684 ) ) ;
#23080 = DIRECTION ( 'NONE',  ( -0.000000000000000000, 1.000000000000000000, -0.000000000000000000 ) ) ;
#23081 = VECTOR ( 'NONE', #36870, 1000.000000000000000 ) ;
#23082 = CARTESIAN_POINT ( 'NONE',  ( 769.9999999999992042, 178.9475563372491251, -320.0000000000000000 ) ) ;
#23083 = CARTESIAN_POINT ( 'NONE',  ( 804.7487373415286811, -355.5436935675103882, 364.7487373415288516 ) ) ;
#23084 = CARTESIAN_POINT ( 'NONE',  ( 762.3223304703356007, -343.5436935675103314, -322.3223304703362828 ) ) ;
#23085 = CARTESIAN_POINT ( 'NONE',  ( 804.9363028652555840, -448.2709662947827951, 338.2165204200192079 ) ) ;
#23086 = CARTESIAN_POINT ( 'NONE',  ( 778.7629533639073998, -104.7363362996985785, -375.0009284576466371 ) ) ;
#23087 = CARTESIAN_POINT ( 'NONE',  ( 754.9735926884551418, -162.3510508353235196, -340.5236548041000333 ) ) ;
#23088 = CARTESIAN_POINT ( 'NONE',  ( 815.0009284576459549, -150.3510508353235480, 338.7629533639073429 ) ) ;
#23089 = CARTESIAN_POINT ( 'NONE',  ( 800.0135310231082713, 9.910851887033969021, 325.0180583372163028 ) ) ;
#23090 = CARTESIAN_POINT ( 'NONE',  ( 804.4286716492782716, -41.36187538569314626, -345.3141322388244703 ) ) ;
#23091 = CARTESIAN_POINT ( 'NONE',  ( 766.7756240680305382, -158.5328690171417065, -361.5560724626415663 ) ) ;
#23092 = CARTESIAN_POINT ( 'NONE',  ( 767.8955696845333705, -120.4527844766019484, -362.1676090361162323 ) ) ;
#23093 = CARTESIAN_POINT ( 'NONE',  ( 805.1927285166397041, -112.8164208402383508, 341.8018195045277707 ) ) ;
#23094 = CARTESIAN_POINT ( 'NONE',  ( 794.1144889064781864, -418.1692326535044799, -360.9840315886528401 ) ) ;
#23095 = CARTESIAN_POINT ( 'NONE',  ( 788.7366044899766848, -275.9073299311469896, 316.5762568750059813 ) ) ;
#23096 = AXIS2_PLACEMENT_3D ( 'NONE', #38282, #31785, #7095 ) ;
#23097 = DIRECTION ( 'NONE',  ( 0.000000000000000000, 0.6755902076156502511, 0.7372773368101330771 ) ) ;
#23098 = VERTEX_POINT ( 'NONE', #45107 ) ;
#23099 = CARTESIAN_POINT ( 'NONE',  ( 803.4237431249931660, -447.1800572038736732, 331.2633955100225194 ) ) ;
#23100 = AXIS2_PLACEMENT_3D ( 'NONE', #15929, #5295, #43863 ) ;
#23101 = CARTESIAN_POINT ( 'NONE',  ( 814.4686193811664907, -267.2817908451526137, -346.2056067578752732 ) ) ;
#23102 = ORIENTED_EDGE ( 'NONE', *, *, #13502, .F. ) ;
#23103 = CARTESIAN_POINT ( 'NONE',  ( 801.1904061080338124, -212.0891481129653187, 368.3070685750236066 ) ) ;
#23104 = CARTESIAN_POINT ( 'NONE',  ( 804.1105419155481968, -315.8272453906070609, 347.6308680596136469 ) ) ;
#23105 = CARTESIAN_POINT ( 'NONE',  ( 769.1273215169530886, -382.7146871989591546, 317.4527132478988847 ) ) ;
#23106 = ORIENTED_EDGE ( 'NONE', *, *, #42760, .F. ) ;
#23107 = CARTESIAN_POINT ( 'NONE',  ( 804.1105419155481968, -123.8272453906076009, -347.6308680596136469 ) ) ;
#23108 = CARTESIAN_POINT ( 'NONE',  ( 771.1735550268778070, -129.1800572038746111, -316.3353852180827630 ) ) ;
#23109 = CARTESIAN_POINT ( 'NONE',  ( 785.3687786644885591, -275.3618753856924286, -315.3201227861280813 ) ) ;
#23110 = ORIENTED_EDGE ( 'NONE', *, *, #25847, .T. ) ;
#23111 = CARTESIAN_POINT ( 'NONE',  ( 774.6312213355099630, -431.3618753856918033, -364.6798772138717482 ) ) ;
#23112 = CARTESIAN_POINT ( 'NONE',  ( 797.6776695296629214, -91.54369356751116982, -357.6776695296636603 ) ) ;
#23113 = CARTESIAN_POINT ( 'NONE',  ( 779.4709603349208464, -288.3510508353231216, 314.7162404726379918 ) ) ;
#23114 = CARTESIAN_POINT ( 'NONE',  ( 51.16348990802859475, 240.0000000000000568, -199.9999999999945146 ) ) ;
#23115 = DIRECTION ( 'NONE',  ( -0.000000000000000000, 1.000000000000000000, -0.000000000000000000 ) ) ;
#23116 = CARTESIAN_POINT ( 'NONE',  ( 797.8594530101008786, 10.45630643248850866, 322.1405469898980982 ) ) ;
#23117 = ORIENTED_EDGE ( 'NONE', *, *, #30060, .T. ) ;
#23118 = CARTESIAN_POINT ( 'NONE',  ( 786.2694204179717872, -357.2817908451523294, -305.1769319972829067 ) ) ;
#23120 = CARTESIAN_POINT ( 'NONE',  ( 794.9819416627830151, -276.9982390220559978, -319.9864689768909898 ) ) ;
#23119 = FACE_BOUND ( 'NONE', #5176, .T. ) ;
#23121 = PLANE ( 'NONE',  #25898 ) ;
#23122 = CARTESIAN_POINT ( 'NONE',  ( 787.5531968255692163, -189.8272453906073736, -316.1348686366205811 ) ) ;
#23123 = CARTESIAN_POINT ( 'NONE',  ( 796.9462024416508257, -36.45278447660223975, 308.9653473494370246 ) ) ;
#23124 = AXIS2_PLACEMENT_3D ( 'NONE', #4754, #29471, #25772 ) ;
#23125 = DIRECTION ( 'NONE',  ( 0.000000000000000000, 0.000000000000000000, 1.000000000000000000 ) ) ;
#23126 = CARTESIAN_POINT ( 'NONE',  ( 814.2001403089898304, -377.3618753856920875, -347.4397851343538264 ) ) ;
#23127 =( GEOMETRIC_REPRESENTATION_CONTEXT ( 3 ) GLOBAL_UNCERTAINTY_ASSIGNED_CONTEXT ( ( #6241 ) ) GLOBAL_UNIT_ASSIGNED_CONTEXT ( ( #45148, #3342, #38442 ) ) REPRESENTATION_CONTEXT ( 'NONE', 'WORKASPACE' ) );
#23128 = FILL_AREA_STYLE ('',( #37697 ) ) ;
#23129 = CARTESIAN_POINT ( 'NONE',  ( 785.3687786644884454, -59.36187538569306810, 315.3201227861279676 ) ) ;
#23130 = CARTESIAN_POINT ( 'NONE',  ( 773.7305795820266212, -321.2817908451525000, 374.8230680027170365 ) ) ;
#23131 = CARTESIAN_POINT ( 'NONE',  ( 787.4397851343537695, -261.7255117493288026, 374.2001403089903988 ) ) ;
#23132 = CARTESIAN_POINT ( 'NONE',  ( 755.2512626584698410, -31.54369356751135456, -315.2512626584710915 ) ) ;
#23133 = CARTESIAN_POINT ( 'NONE',  ( 804.9363028652555840, -232.2709662947834488, -338.2165204200192079 ) ) ;
#23134 = DIRECTION ( 'NONE',  ( 1.000000000000000000, -0.000000000000000000, -0.000000000000000000 ) ) ;
#23135 = CARTESIAN_POINT ( 'NONE',  ( 767.8955696845333705, -360.4527844766010958, 362.1676090361162323 ) ) ;
#23136 = CARTESIAN_POINT ( 'NONE',  ( 755.3028492785439312, -135.2817908451530116, 335.9200461376539693 ) ) ;
#23137 = CARTESIAN_POINT ( 'NONE',  ( 756.7813123517142913, -19.98741447168758256, -329.9779781133712504 ) ) ;
#23138 = CARTESIAN_POINT ( 'NONE',  ( 767.8955696845334842, -384.4527844766011526, 362.1676090361161755 ) ) ;
#23139 = DIRECTION ( 'NONE',  ( 0.000000000000000000, 0.000000000000000000, 1.000000000000000000 ) ) ;
#23140 = VECTOR ( 'NONE', #34958, 1000.000000000000114 ) ;
#23141 = CARTESIAN_POINT ( 'NONE',  ( 799.9999999999993179, -512.9681489794448908, 309.9999999999998863 ) ) ;
#23142 = CARTESIAN_POINT ( 'NONE',  ( 755.0636971347428243, -412.2709662947829088, 341.7834795799807353 ) ) ;
#23143 = ORIENTED_EDGE ( 'NONE', *, *, #12533, .F. ) ;
#23144 = CARTESIAN_POINT ( 'NONE',  ( 804.1601925771018387, -319.4419599262320730, -346.5483106153029098 ) ) ;
#23146 = CARTESIAN_POINT ( 'NONE',  ( 756.5762568750052424, -147.1800572038746395, 348.7366044899774238 ) ) ;
#23145 = CARTESIAN_POINT ( 'NONE',  ( 764.8639956371174549, -200.0891481129653187, 319.7806653035542013 ) ) ;
#23147 = CARTESIAN_POINT ( 'NONE',  ( 781.2497674668890113, -372.3510508353228374, -375.3608509340180603 ) ) ;
#23148 = CARTESIAN_POINT ( 'NONE',  ( 914.9999999999992042, 74.99999999999984368, 350.0000000000000000 ) ) ;
#23149 = EDGE_CURVE ( 'NONE', #24787, #19824, #27095, .T. ) ;
#23150 = ORIENTED_EDGE ( 'NONE', *, *, #19367, .F. ) ;
#23151 = CARTESIAN_POINT ( 'NONE',  ( 755.5713283507202505, -365.3618753856920875, 334.6858677611754729 ) ) ;
#23152 = ORIENTED_EDGE ( 'NONE', *, *, #16294, .F. ) ;
#23153 = CARTESIAN_POINT ( 'NONE',  ( 0.000000000000000000, 0.000000000000000000, 0.000000000000000000 ) ) ;
#23154 = CARTESIAN_POINT ( 'NONE',  ( 744.7301800767019131, -196.8164208402380950, -337.4774526936615757 ) ) ;
#23155 = CARTESIAN_POINT ( 'NONE',  ( 814.5518280994195948, -111.7255117493292857, 332.4837098697145166 ) ) ;
#23156 = AXIS2_PLACEMENT_3D ( 'NONE', #547, #42338, #3323 ) ;
#23157 = ORIENTED_EDGE ( 'NONE', *, *, #39633, .F. ) ;
#23158 = CARTESIAN_POINT ( 'NONE',  ( 759.9864689768902508, -194.0891481129654039, -354.9819416627836404 ) ) ;
#23159 = AXIS2_PLACEMENT_3D ( 'NONE', #16004, #26606, #30774 ) ;
#23160 = ORIENTED_EDGE ( 'NONE', *, *, #14545, .T. ) ;
#23161 = CARTESIAN_POINT ( 'NONE',  ( 804.4286716492782716, -329.3618753856922581, -345.3141322388244703 ) ) ;
#23162 = CARTESIAN_POINT ( 'NONE',  ( 796.9571628226829034, -455.4636090269701754, -321.2382568024804641 ) ) ;
#23163 = CARTESIAN_POINT ( 'NONE',  ( 767.6429770376289525, -249.1800572038742416, 306.8695393053162093 ) ) ;
#23164 = CARTESIAN_POINT ( 'NONE',  ( 786.6156483768007774, -193.4419599262325278, 315.5913626894246136 ) ) ;
#23166 = DIRECTION ( 'NONE',  ( 0.000000000000000000, 0.000000000000000000, 1.000000000000000000 ) ) ;
#23165 = LINE ( 'NONE', #33815, #1184 ) ;
#23167 = DIRECTION ( 'NONE',  ( -0.000000000000000000, 1.000000000000000000, -0.000000000000000000 ) ) ;
#23168 = VERTEX_POINT ( 'NONE', #23826 ) ;
#23169 = CARTESIAN_POINT ( 'NONE',  ( 798.5707757039680246, -437.4636090269703459, -356.7845633553585003 ) ) ;
#23170 = CARTESIAN_POINT ( 'NONE',  ( -26.63011601220122060, -513.1383975375929367, -369.9999999999999432 ) ) ;
#23171 = DIRECTION ( 'NONE',  ( 1.000000000000000000, 0.000000000000000000, 0.000000000000000000 ) ) ;
#23172 = ORIENTED_EDGE ( 'NONE', *, *, #34811, .T. ) ;
#23173 = CARTESIAN_POINT ( 'NONE',  ( 760.0363995740630116, -250.9181544815163534, -368.7758568127991907 ) ) ;
#23174 = CARTESIAN_POINT ( 'NONE',  ( 807.2620300519052989, -120.0090635724258021, 318.0141637701419768 ) ) ;
#23175 = VECTOR ( 'NONE', #23505, 1000.000000000000000 ) ;
#23177 = CARTESIAN_POINT ( 'NONE',  ( 755.5713283507202505, -173.3618753856927128, -334.6858677611754729 ) ) ;
#23176 = DIRECTION ( 'NONE',  ( 0.000000000000000000, 0.000000000000000000, -1.000000000000000000 ) ) ;
#23178 = CARTESIAN_POINT ( 'NONE',  ( 760.5453621957607311, -357.0783235625956422, -323.8424801807151425 ) ) ;
#23179 = CARTESIAN_POINT ( 'NONE',  ( 187.1337867209877857, 62.85347435602256638, -357.4246812887967053 ) ) ;
#23180 = CARTESIAN_POINT ( 'NONE',  ( 783.7953271457878373, -224.1908817542436623, -375.1787889125761239 ) ) ;
#23181 = DIRECTION ( 'NONE',  ( 0.000000000000000000, 1.000000000000000000, -0.000000000000000000 ) ) ;
#23182 = DIRECTION ( 'NONE',  ( -0.000000000000000000, -0.000000000000000000, 1.000000000000000000 ) ) ;
#23183 = CARTESIAN_POINT ( 'NONE',  ( 769.0155153010367712, -82.37269993606227558, -362.7791456095907279 ) ) ;
#23184 = CARTESIAN_POINT ( 'NONE',  ( 766.9102291470427417, -426.5545181178794678, 318.6633372737382501 ) ) ;
#23185 = VECTOR ( 'NONE', #21572, 999.9999999999998863 ) ;
#23186 = CARTESIAN_POINT ( 'NONE',  ( -598.8365100919716042, 256.5000000000001705, -199.9999999999899671 ) ) ;
#23187 = CARTESIAN_POINT ( 'NONE',  ( 814.5518280994195948, -279.7255117493288026, -332.4837098697145166 ) ) ;
#23188 = DIRECTION ( 'NONE',  ( -1.000000000000000000, -0.000000000000000000, 0.000000000000000000 ) ) ;
#23189 = CARTESIAN_POINT ( 'NONE',  ( -598.8365100919716042, 256.5000000000001705, -197.2499999999900524 ) ) ;
#23190 = CARTESIAN_POINT ( 'NONE',  ( 803.6646147819161570, -41.90732993114767169, -348.8264449731210561 ) ) ;
#23191 = CARTESIAN_POINT ( 'NONE',  ( 805.6418435158337843, -221.4636090269709428, 363.8556311672236916 ) ) ;
#23192 = CARTESIAN_POINT ( 'NONE',  ( 744.8212110874229666, -138.8965053807781374, -336.2046728542121627 ) ) ;
#23193 = CARTESIAN_POINT ( 'NONE',  ( 751.9810565676468741, -146.0891481129655176, 360.9747183278973921 ) ) ;
#23194 = CARTESIAN_POINT ( 'NONE',  ( 763.0537975583475827, -408.4527844766009252, -371.0346526505627480 ) ) ;
#23195 = LINE ( 'NONE', #18864, #1790 ) ;
#23196 = CARTESIAN_POINT ( 'NONE',  ( 774.6312213355099630, -263.3618753856924855, 364.6798772138717482 ) ) ;
#23197 = CARTESIAN_POINT ( 'NONE',  ( 804.8461984189677878, -26.19088175424427334, 336.9566956441385628 ) ) ;
#23198 = CARTESIAN_POINT ( 'NONE',  ( 802.1676090361156639, -374.6346026584192828, -327.8955696845344505 ) ) ;
#23199 = CARTESIAN_POINT ( 'NONE',  ( 998.9999999999992042, -600.0000000000001137, -360.0000000000000000 ) ) ;
#23200 = CARTESIAN_POINT ( 'NONE',  ( 776.2046728542105711, -44.19088175424421649, -304.8212110874238761 ) ) ;
#23201 = CYLINDRICAL_SURFACE ( 'NONE', #1854, 7.999999999999896083 ) ;
#23203 = CARTESIAN_POINT ( 'NONE',  ( 805.1927285166397041, -304.8164208402376403, 341.8018195045277707 ) ) ;
#23202 = CARTESIAN_POINT ( 'NONE',  ( 799.4546378042377910, -105.0783235625964096, 356.1575198192848006 ) ) ;
#23204 = ORIENTED_EDGE ( 'NONE', *, *, #13049, .T. ) ;
#23205 = EDGE_CURVE ( 'NONE', #3123, #30414, #45070, .T. ) ;
#23206 = CARTESIAN_POINT ( 'NONE',  ( 757.2208543904082489, -208.7146871989596946, -350.9844846989624330 ) ) ;
#23207 = CARTESIAN_POINT ( 'NONE',  ( 795.1360043628807261, -44.08914811296584446, 360.2193346964456282 ) ) ;
#23208 = AXIS2_PLACEMENT_3D ( 'NONE', #25874, #8570, #37173 ) ;
#23209 = CARTESIAN_POINT ( 'NONE',  ( 751.2241431872005251, -232.1692326535051620, -359.9636004259367610 ) ) ;
#23210 = CARTESIAN_POINT ( 'NONE',  ( 999.9999999999992042, 249.9999999999998863, 360.0000000000000000 ) ) ;
#23211 = CARTESIAN_POINT ( 'NONE',  ( 803.8556311672234642, -393.6237781080500326, 365.6418435158340117 ) ) ;
#23212 = VERTEX_POINT ( 'NONE', #2451 ) ;
#23213 = VECTOR ( 'NONE', #18925, 1000.000000000000000 ) ;
#23214 = CARTESIAN_POINT ( 'NONE',  ( 749.2812353651451076, -6.452784476602343666, 323.2262854647983090 ) ) ;
#23215 = CARTESIAN_POINT ( 'NONE',  ( 763.2154366446407039, -21.62377810805121570, -321.4292242960311228 ) ) ;
#23216 = CARTESIAN_POINT ( 'NONE',  ( 797.6776695296629214, -187.5436935675108430, -357.6776695296636603 ) ) ;
#23217 = CARTESIAN_POINT ( 'NONE',  ( 762.3223304703356007, -367.5436935675102745, 322.3223304703362828 ) ) ;
#23218 = EDGE_CURVE ( 'NONE', #25919, #18880, #39521, .T. ) ;
#23219 = AXIS2_PLACEMENT_3D ( 'NONE', #28046, #6800, #34975 ) ;
#23220 = CARTESIAN_POINT ( 'NONE',  ( 813.1304606946830518, -89.90732993114750116, -352.3570229623690580 ) ) ;
#23221 = AXIS2_PLACEMENT_3D ( 'NONE', #1948, #6725, #19500 ) ;
#23222 = EDGE_CURVE ( 'NONE', #2103, #32355, #38033, .T. ) ;
#23223 = CARTESIAN_POINT ( 'NONE',  ( 785.3687786644885591, -59.36187538569307520, -315.3201227861280813 ) ) ;
#23224 = EDGE_LOOP ( 'NONE', ( #37840, #28698 ) ) ;
#23225 = CARTESIAN_POINT ( 'NONE',  ( 757.4527132478984868, -16.37269993606248519, -329.1273215169538844 ) ) ;
#23226 = VERTEX_POINT ( 'NONE', #3137 ) ;
#23227 = CARTESIAN_POINT ( 'NONE',  ( 804.4086373105744769, -361.6454272087887603, -333.3843516231986541 ) ) ;
#23229 = CARTESIAN_POINT ( 'NONE',  ( 759.0159684113467620, -400.9181544815159555, 325.8855110935213020 ) ) ;
#23228 = CARTESIAN_POINT ( 'NONE',  ( 781.8018195045266339, -94.27096629478386092, 365.1927285166406705 ) ) ;
#23230 = CARTESIAN_POINT ( 'NONE',  ( 784.0799538623451781, -107.8055962898691433, 364.6971507214555572 ) ) ;
#23233 = CARTESIAN_POINT ( 'NONE',  ( 764.3348316497523456, -310.7146871989593251, 308.6759233522265617 ) ) ;
#23232 = DIRECTION ( 'NONE',  ( 1.000000000000000000, 0.000000000000000000, 0.000000000000000000 ) ) ;
#23231 = CARTESIAN_POINT ( 'NONE',  ( 811.0346526505617248, -422.6346026584191691, 323.0537975583478101 ) ) ;
#23234 = AXIS2_PLACEMENT_3D ( 'NONE', #7441, #32388, #14617 ) ;
#23235 = CARTESIAN_POINT ( 'NONE',  ( 799.2566176426618085, -312.0090635724251911, -324.0069404352559559 ) ) ;
#23236 = CARTESIAN_POINT ( 'NONE',  ( 781.8018195045266339, -310.2709662947832499, -365.1927285166406705 ) ) ;
#23237 = CARTESIAN_POINT ( 'NONE',  ( 745.5313806188320314, -135.2817908451530116, -333.7943932421247268 ) ) ;
#23238 = VECTOR ( 'NONE', #7849, 1000.000000000000000 ) ;
#23239 = EDGE_CURVE ( 'NONE', #13477, #25691, #24372, .T. ) ;
#23240 = CARTESIAN_POINT ( 'NONE',  ( 810.7187646348534145, -450.4527844766009821, 356.7737145352016341 ) ) ;
#23241 = VECTOR ( 'NONE', #40214, 1000.000000000000000 ) ;
#23243 = DIRECTION ( 'NONE',  ( 0.000000000000000000, 1.000000000000000000, 0.000000000000000000 ) ) ;
#23242 = DIRECTION ( 'NONE',  ( -0.000000000000000000, 1.000000000000000000, -0.000000000000000000 ) ) ;
#23244 = EDGE_CURVE ( 'NONE', #35615, #27491, #13319, .T. ) ;
#23245 = CARTESIAN_POINT ( 'NONE',  ( 771.3260364891663130, -115.6454272087894424, -306.0683387631859773 ) ) ;
#23246 = CARTESIAN_POINT ( 'NONE',  ( 927.9999999999993179, 219.9999999999998863, -359.9749999999999659 ) ) ;
#23247 = DIRECTION ( 'NONE',  ( 0.000000000000000000, 0.000000000000000000, -1.000000000000000000 ) ) ;
#23248 = CARTESIAN_POINT ( 'NONE',  ( 769.0155153010367712, -322.3726999360615082, 362.7791456095907279 ) ) ;
#23249 = CARTESIAN_POINT ( 'NONE',  ( 801.9419747391806368, -186.4527844766017779, 351.9812246680014027 ) ) ;
#23250 = EDGE_CURVE ( 'NONE', #8526, #27321, #34322, .T. ) ;
#23251 = VERTEX_POINT ( 'NONE', #23912 ) ;
#23252 = CARTESIAN_POINT ( 'NONE',  ( 793.5525998758768083, -319.0999726633342561, 372.6845335610516941 ) ) ;
#23253 = CARTESIAN_POINT ( 'NONE',  ( 814.5518280994195948, -159.7255117493291436, -332.4837098697145166 ) ) ;
#23254 = CARTESIAN_POINT ( 'NONE',  ( 939.9999999999993179, -431.4567479753240491, -350.0000000000000000 ) ) ;
#23255 = AXIS2_PLACEMENT_3D ( 'NONE', #25732, #21808, #11419 ) ;
#23256 = CARTESIAN_POINT ( 'NONE',  ( 814.4686193811664907, -75.28179084515321051, 346.2056067578752732 ) ) ;
#23257 = CARTESIAN_POINT ( 'NONE',  ( 814.2001403089898304, -257.3618753856924286, -347.4397851343538264 ) ) ;
#23258 = AXIS2_PLACEMENT_3D ( 'NONE', #10736, #4275, #18367 ) ;
#23259 = CARTESIAN_POINT ( 'NONE',  ( 748.9653473494365699, -434.6346026584190554, -356.9462024416520762 ) ) ;
#23260 = CARTESIAN_POINT ( 'NONE',  ( 788.7366044899766848, -155.9073299311473306, 316.5762568750059813 ) ) ;
#23261 = VERTEX_POINT ( 'NONE', #42170 ) ;
#23262 = CARTESIAN_POINT ( 'NONE',  ( 762.1177392798416577, -402.5545181178795247, 309.8865473780659272 ) ) ;
#23263 = CARTESIAN_POINT ( 'NONE',  ( 759.8311093483677041, -334.1692326535047073, -310.9282345327691814 ) ) ;
#23264 = CARTESIAN_POINT ( 'NONE',  ( 805.0032342141412300, -85.54369356751118403, -314.9967657858571783 ) ) ;
#23265 = EDGE_CURVE ( 'NONE', #24190, #36920, #45421, .T. ) ;
#23266 = CARTESIAN_POINT ( 'NONE',  ( 776.9254006560222479, -68.19088175424413123, 314.8983024940802125 ) ) ;
#23267 = CARTESIAN_POINT ( 'NONE',  ( 745.7998596910086917, -389.3618753856919739, -332.5602148656461168 ) ) ;
#23268 = LINE ( 'NONE', #5485, #45369 ) ;
#23269 = CARTESIAN_POINT ( 'NONE',  ( 798.7617431975189675, -435.6237781080499190, 323.0428371773161871 ) ) ;
#23270 = ORIENTED_EDGE ( 'NONE', *, *, #1487, .F. ) ;
#23271 = EDGE_CURVE ( 'NONE', #41554, #44486, #44962, .T. ) ;
#23272 = CARTESIAN_POINT ( 'NONE',  ( 771.2368401574024119, -133.4419599262326699, -374.2805881961240857 ) ) ;
#23273 = DIRECTION ( 'NONE',  ( 0.000000000000000000, 0.000000000000000000, 1.000000000000000000 ) ) ;
#23274 = CARTESIAN_POINT ( 'NONE',  ( 778.7502325331095108, -264.3510508353232353, 304.6391490659818828 ) ) ;
#23275 = CARTESIAN_POINT ( 'NONE',  ( 758.0580252608178853, -78.45278447660211896, 328.0187753319985404 ) ) ;
#23276 = ORIENTED_EDGE ( 'NONE', *, *, #35704, .T. ) ;
#23277 = AXIS2_PLACEMENT_3D ( 'NONE', #12179, #16318, #8726 ) ;
#23278 = CARTESIAN_POINT ( 'NONE',  ( 780.5290396650775619, -12.35105083532396897, -365.2837595273619513 ) ) ;
#23279 = EDGE_CURVE ( 'NONE', #19176, #22430, #3381, .T. ) ;
#23280 = CARTESIAN_POINT ( 'NONE',  ( 781.8018195045266339, -286.2709662947833635, 365.1927285166406705 ) ) ;
#23281 = EDGE_CURVE ( 'NONE', #861, #14052, #27394, .T. ) ;
#23282 = CARTESIAN_POINT ( 'NONE',  ( 756.1443688327750579, -429.6237781080499190, -314.3581564841659315 ) ) ;
#23283 = LINE ( 'NONE', #12664, #14342 ) ;
#23284 = ORIENTED_EDGE ( 'NONE', *, *, #7500, .T. ) ;
#23285 = ORIENTED_EDGE ( 'NONE', *, *, #29254, .F. ) ;
#23286 = CARTESIAN_POINT ( 'NONE',  ( 750.9282345327678740, -376.9181544815159555, -319.8311093483690115 ) ) ;
#23287 = AXIS2_PLACEMENT_3D ( 'NONE', #23141, #26619, #40717 ) ;
#23288 = CARTESIAN_POINT ( 'NONE',  ( 785.3141322388236176, -237.7255117493289163, -364.4286716492789537 ) ) ;
#23289 = AXIS2_PLACEMENT_3D ( 'NONE', #28074, #30638, #38713 ) ;
#23291 = CARTESIAN_POINT ( 'NONE',  ( 811.6461892240364477, -220.7146871989596661, 324.1737431748509835 ) ) ;
#23290 = CARTESIAN_POINT ( 'NONE',  ( 751.6929314249750860, -342.9982390220557704, 318.8095938919659034 ) ) ;
#23292 = CARTESIAN_POINT ( 'NONE',  ( 759.8311093483677041, -22.16923265350575889, 310.9282345327691814 ) ) ;
#23293 = CARTESIAN_POINT ( 'NONE',  ( 804.1105419155481968, -219.8272453906073167, -347.6308680596136469 ) ) ;
#23294 = CARTESIAN_POINT ( 'NONE',  ( 803.6646147819161570, -233.9073299311470180, -348.8264449731210561 ) ) ;
#23295 = CARTESIAN_POINT ( 'NONE',  ( 791.9812246680005501, -428.6346026584192259, -361.9419747391813189 ) ) ;
#23296 = ORIENTED_EDGE ( 'NONE', *, *, #11651, .F. ) ;
#23297 = CARTESIAN_POINT ( 'NONE',  ( 755.3201227861273992, -99.72551174932928575, -345.3687786644892981 ) ) ;
#23298 = CARTESIAN_POINT ( 'NONE',  ( 808.0189434323515343, -374.0891481129647786, 319.0252816721025511 ) ) ;
#23299 = LINE ( 'NONE', #37620, #13762 ) ;
#23300 = EDGE_CURVE ( 'NONE', #22833, #30278, #41749, .T. ) ;
#23301 = CARTESIAN_POINT ( 'NONE',  ( 793.3891180349545493, 16.45630643248849978, 314.6660875939051607 ) ) ;
#23302 = DIRECTION ( 'NONE',  ( -1.000000000000000000, -0.000000000000000000, -0.000000000000000000 ) ) ;
#23303 = CARTESIAN_POINT ( 'NONE',  ( 798.5707757039680246, -221.4636090269709428, 356.7845633553585003 ) ) ;
#23304 = CARTESIAN_POINT ( 'NONE',  ( 781.7834795799800531, -82.81642084023846451, 315.0636971347436202 ) ) ;
#23305 = ORIENTED_EDGE ( 'NONE', *, *, #14520, .T. ) ;
#23306 = CARTESIAN_POINT ( 'NONE',  ( 747.6481478633932056, -445.0999726633338582, -353.4146539503763620 ) ) ;
#23307 = CARTESIAN_POINT ( 'NONE',  ( 811.0346526505617248, -38.63460265842041963, -323.0537975583478101 ) ) ;
#23308 = CARTESIAN_POINT ( 'NONE',  ( 803.2186876482843445, -247.9874144716867761, 350.0220218866286928 ) ) ;
#23309 = CARTESIAN_POINT ( 'NONE',  ( 797.6776695296629214, -427.5436935675101040, -357.6776695296636603 ) ) ;
#23310 = CARTESIAN_POINT ( 'NONE',  ( 759.7806653035535192, -6.998239022056886860, -324.8639956371181370 ) ) ;
#23311 = CARTESIAN_POINT ( 'NONE',  ( 759.0252816721024374, -432.9982390220555999, 368.0189434323527280 ) ) ;
#23312 = CARTESIAN_POINT ( 'NONE',  ( -78.83651009197140525, 256.5000000000000568, -199.9999999999936051 ) ) ;
#23313 = CARTESIAN_POINT ( 'NONE',  ( 790.9844846989617508, -286.3726999360617356, -317.2208543904092721 ) ) ;
#23314 = CARTESIAN_POINT ( 'NONE',  ( 804.7487373415286811, -163.5436935675109567, -364.7487373415288516 ) ) ;
#23315 = CARTESIAN_POINT ( 'NONE',  ( 748.9653473494363425, -74.63460265842032015, 356.9462024416521331 ) ) ;
#23316 = CARTESIAN_POINT ( 'NONE',  ( 758.8095938919642549, -152.0891481129655460, 311.6929314249763365 ) ) ;
#23317 = CARTESIAN_POINT ( 'NONE',  ( 783.6926022324497580, 16.45630643248849267, -313.7971720364932935 ) ) ;
#23318 = CARTESIAN_POINT ( 'NONE',  ( 989.9999999999992042, -434.4637272565419153, 347.3621835540870393 ) ) ;
#23319 = CARTESIAN_POINT ( 'NONE',  ( 745.1769319972822814, -233.8055962898687028, -346.2694204179732083 ) ) ;
#23320 = EDGE_CURVE ( 'NONE', #12731, #37281, #13545, .T. ) ;
#23321 = DIRECTION ( 'NONE',  ( 0.000000000000000000, 0.000000000000000000, -1.000000000000000000 ) ) ;
#23322 = CARTESIAN_POINT ( 'NONE',  ( 804.7487373415286811, -403.5436935675101608, 364.7487373415288516 ) ) ;
#23323 = CARTESIAN_POINT ( 'NONE',  ( 747.2067596250078623, -3.180057203875080063, 352.2312462859687230 ) ) ;
#23324 = CARTESIAN_POINT ( 'NONE',  ( 768.0187753319979720, -344.6346026584195101, -318.0580252608186242 ) ) ;
#23325 = VECTOR ( 'NONE', #33255, 1000.000000000000000 ) ;
#23326 = ADVANCED_FACE ( 'NONE', ( #41727 ), #10081, .F. ) ;
#23327 = CARTESIAN_POINT ( 'NONE',  ( 763.2154366446407039, 2.376221891948710585, 321.4292242960311228 ) ) ;
#23328 = CARTESIAN_POINT ( 'NONE',  ( 815.3608509340175488, -98.73633629969859271, -341.2497674668889545 ) ) ;
#23329 = CARTESIAN_POINT ( 'NONE',  ( 756.7813123517142913, -139.9874144716872024, -329.9779781133712504 ) ) ;
#23330 = CARTESIAN_POINT ( 'NONE',  ( 815.1787889125755555, -174.8965053807779952, 343.7953271457877804 ) ) ;
#23331 = CARTESIAN_POINT ( 'NONE',  ( 787.4999999999992042, -462.9681489794448339, -370.0000000000000568 ) ) ;
#23332 = CARTESIAN_POINT ( 'NONE',  ( 790.8726784830453198, -154.7146871989598935, -362.5472867521010585 ) ) ;
#23333 = CARTESIAN_POINT ( 'NONE',  ( 755.5713283507202505, -173.3618753856927128, 334.6858677611754729 ) ) ;
#23334 = CARTESIAN_POINT ( 'NONE',  ( 800.1688906516307043, -10.16923265350579442, -369.0717654672308186 ) ) ;
#23335 = PRODUCT_DEFINITION ( 'UNKNOWN', '', #45220, #41365 ) ;
#23337 = CARTESIAN_POINT ( 'NONE',  ( 767.8955696845334842, -288.4527844766014937, 362.1676090361161755 ) ) ;
#23336 = CARTESIAN_POINT ( 'NONE',  ( 781.8018195045266339, -286.2709662947833635, 365.1927285166406705 ) ) ;
#23338 = FACE_BOUND ( 'NONE', #26528, .T. ) ;
#23339 = ORIENTED_EDGE ( 'NONE', *, *, #20986, .F. ) ;
#23340 = CARTESIAN_POINT ( 'NONE',  ( 800.7704444035546203, -4.169232653505813069, 326.0291762391768771 ) ) ;
#23341 = CARTESIAN_POINT ( 'NONE',  ( 799.9636004259356241, -262.9181544815162965, -311.2241431872006956 ) ) ;
#23342 = ORIENTED_EDGE ( 'NONE', *, *, #14859, .T. ) ;
#23343 = DIRECTION ( 'NONE',  ( -1.000000000000000000, 0.000000000000000000, 0.000000000000000000 ) ) ;
#23344 = VECTOR ( 'NONE', #14174, 1000.000000000000000 ) ;
#23345 = CARTESIAN_POINT ( 'NONE',  ( 787.5162901302840055, -227.3618753856925423, 305.4481719005793252 ) ) ;
#23346 = CARTESIAN_POINT ( 'NONE',  ( 805.2837595273609850, -314.7363362996979959, 340.5290396650784714 ) ) ;
#23347 = CARTESIAN_POINT ( 'NONE',  ( 766.7756240680305382, -398.5328690171409107, 361.5560724626415663 ) ) ;
#23348 = EDGE_LOOP ( 'NONE', ( #22266, #31924 ) ) ;
#23350 = VECTOR ( 'NONE', #37910, 1000.000000000000000 ) ;
#23349 = CARTESIAN_POINT ( 'NONE',  ( 804.4086373105744769, -121.6454272087894282, -333.3843516231986541 ) ) ;
#23351 = CARTESIAN_POINT ( 'NONE',  ( 788.7366044899766848, -107.9073299311474727, -316.5762568750059813 ) ) ;
#23352 = CARTESIAN_POINT ( 'NONE',  ( 800.0135310231082713, -302.0891481129650629, -325.0180583372163028 ) ) ;
#23353 = VERTEX_POINT ( 'NONE', #34774 ) ;
#23354 = CARTESIAN_POINT ( 'NONE',  ( 762.1405469898971887, -433.5436935675099903, -357.8594530101015607 ) ) ;
#23355 = CARTESIAN_POINT ( 'NONE',  ( 773.3843516231979720, -301.4419599262320730, 364.4086373105754433 ) ) ;
#23356 = LINE ( 'NONE', #21218, #23350 ) ;
#23357 = FACE_OUTER_BOUND ( 'NONE', #39158, .T. ) ;
#23358 = AXIS2_PLACEMENT_3D ( 'NONE', #41043, #37105, #37346 ) ;
#23359 = LINE ( 'NONE', #44619, #26320 ) ;
#23360 = ORIENTED_EDGE ( 'NONE', *, *, #4428, .T. ) ;
#23361 = CARTESIAN_POINT ( 'NONE',  ( 807.2620300519052989, -360.0090635724250774, -318.0141637701419768 ) ) ;
#23362 = CARTESIAN_POINT ( 'NONE',  ( 799.9636004259356241, -190.9181544815164955, 311.2241431872006956 ) ) ;
#23363 = CARTESIAN_POINT ( 'NONE',  ( 801.9419747391806368, -306.4527844766013800, -351.9812246680014027 ) ) ;
#23364 = CARTESIAN_POINT ( 'NONE',  ( -786.4999999999993179, -563.3203001761230553, -342.3463313526983143 ) ) ;
#23365 = CARTESIAN_POINT ( 'NONE',  ( 776.9254006560222479, -188.1908817542437760, -314.8983024940802125 ) ) ;
#23366 = CARTESIAN_POINT ( 'NONE',  ( 751.6929314249748586, -54.99823902205672255, 318.8095938919659034 ) ) ;
#23367 = DIRECTION ( 'NONE',  ( 0.000000000000000000, -1.000000000000000000, 0.000000000000000000 ) ) ;
#23368 = CARTESIAN_POINT ( 'NONE',  ( 745.7998596910086917, -365.3618753856920875, -332.5602148656461168 ) ) ;
#23369 = CARTESIAN_POINT ( 'NONE',  ( 800.0135310231082713, -62.08914811296580183, 325.0180583372163028 ) ) ;
#23370 = CARTESIAN_POINT ( 'NONE',  ( 795.8262568251477660, -334.3726999360615082, 308.3538107759623585 ) ) ;
#23371 = CARTESIAN_POINT ( 'NONE',  ( 759.9999999999992042, -512.9681489794448908, 339.9999999999999432 ) ) ;
#23372 = CARTESIAN_POINT ( 'NONE',  ( 796.7737145352015204, -284.6346026584196807, 370.7187646348536987 ) ) ;
#23373 = CARTESIAN_POINT ( 'NONE',  ( 746.8695393053150156, -29.90732993114771787, -327.6429770376306010 ) ) ;
#23374 = CIRCLE ( 'NONE', #22622, 30.00000000000008171 ) ;
#23375 = CARTESIAN_POINT ( 'NONE',  ( 800.2193346964447755, -258.9982390220561115, -355.1360043628815788 ) ) ;
#23376 = LINE ( 'NONE', #16012, #41656 ) ;
#23377 = CARTESIAN_POINT ( 'NONE',  ( 803.4237431249931660, -375.1800572038739574, 331.2633955100225194 ) ) ;
#23378 = CARTESIAN_POINT ( 'NONE',  ( 775.8780910478218402, -105.2817908451530968, 364.9511171171680530 ) ) ;
#23379 = CARTESIAN_POINT ( 'NONE',  ( 804.9511171171677688, -53.80559628986930676, -335.8780910478229202 ) ) ;
#23380 = CARTESIAN_POINT ( 'NONE',  ( 814.8230680027162407, -29.80559628986937781, 333.7305795820267917 ) ) ;
#23381 = CARTESIAN_POINT ( 'NONE',  ( 754.8072714833583632, -364.8164208402375266, 338.1981804954721156 ) ) ;
#23382 = AXIS2_PLACEMENT_3D ( 'NONE', #10066, #31539, #24357 ) ;
#23383 = CARTESIAN_POINT ( 'NONE',  ( 999.9999999999992042, -600.0000000000001137, -360.0000000000000000 ) ) ;
#23384 = CARTESIAN_POINT ( 'NONE',  ( 787.4999999999992042, -462.9681489794447771, -309.9999999999998863 ) ) ;
#23385 = CARTESIAN_POINT ( 'NONE',  ( 771.1735550268778070, -441.1800572038735027, 316.3353852180827630 ) ) ;
#23386 = ORIENTED_EDGE ( 'NONE', *, *, #43860, .T. ) ;
#23387 = VECTOR ( 'NONE', #23417, 1000.000000000000000 ) ;
#23388 = CARTESIAN_POINT ( 'NONE',  ( 755.8398074228967971, -355.4419599262319593, -333.4516893846970333 ) ) ;
#23390 = CARTESIAN_POINT ( 'NONE',  ( 802.1676090361155502, -206.6346026584198796, 327.8955696845344505 ) ) ;
#23389 = CARTESIAN_POINT ( 'NONE',  ( 803.4237431249931660, -207.1800572038744406, 331.2633955100225194 ) ) ;
#23391 = CARTESIAN_POINT ( 'NONE',  ( 752.4576283171824116, -381.0783235625954717, -317.7880784355627952 ) ) ;
#23392 = DIRECTION ( 'NONE',  ( 0.000000000000000000, 0.000000000000000000, 1.000000000000000000 ) ) ;
#23393 = ORIENTED_EDGE ( 'NONE', *, *, #3799, .F. ) ;
#23394 = CARTESIAN_POINT ( 'NONE',  ( 759.9864689768902508, -386.0891481129647786, 354.9819416627836404 ) ) ;
#23395 = ORIENTED_EDGE ( 'NONE', *, *, #2079, .T. ) ;
#23396 = CARTESIAN_POINT ( 'NONE',  ( 746.8695393053150156, -221.9073299311470464, -327.6429770376306010 ) ) ;
#23397 = CARTESIAN_POINT ( 'NONE',  ( 796.9462024416508257, -132.4527844766019200, 308.9653473494370246 ) ) ;
#23398 = ORIENTED_EDGE ( 'NONE', *, *, #18811, .T. ) ;
#23399 = CARTESIAN_POINT ( 'NONE',  ( 767.8955696845334842, -216.4527844766016926, -362.1676090361161755 ) ) ;
#23400 = VERTEX_POINT ( 'NONE', #13783 ) ;
#23401 = CARTESIAN_POINT ( 'NONE',  ( 756.3353852180819104, -317.9073299311468190, -331.1735550268788302 ) ) ;
#23402 = CARTESIAN_POINT ( 'NONE',  ( 780.5236548040995785, -452.7363362996975411, -314.9735926884559944 ) ) ;
#23403 = CARTESIAN_POINT ( 'NONE',  ( 814.5518280994195948, -255.7255117493287742, 332.4837098697145734 ) ) ;
#23404 = CARTESIAN_POINT ( 'NONE',  ( 798.7617431975189675, -195.6237781080506863, 323.0428371773161871 ) ) ;
#23405 = AXIS2_PLACEMENT_3D ( 'NONE', #35251, #31779, #38727 ) ;
#23407 = CARTESIAN_POINT ( 'NONE',  ( 927.9999999999990905, 154.9999999999998863, -360.0000000000000000 ) ) ;
#23406 = DIRECTION ( 'NONE',  ( -1.000000000000000000, -0.000000000000000000, 0.000000000000000000 ) ) ;
#23408 = CARTESIAN_POINT ( 'NONE',  ( 999.9999999999992042, 249.9999999999998863, 360.0000000000000000 ) ) ;
#23409 = ORIENTED_EDGE ( 'NONE', *, *, #20739, .F. ) ;
#23410 = CARTESIAN_POINT ( 'NONE',  ( 801.5560724626406000, -456.5545181178792404, -326.7756240680316182 ) ) ;
#23411 = CARTESIAN_POINT ( 'NONE',  ( 777.0937506421101943, 18.86692508245304367, -309.9999999999999432 ) ) ;
#23412 = LINE ( 'NONE', #8884, #32204 ) ;
#23413 = ORIENTED_EDGE ( 'NONE', *, *, #39098, .T. ) ;
#23414 = CARTESIAN_POINT ( 'NONE',  ( 814.8207195650702488, -242.1908817542435770, -336.2433038121456548 ) ) ;
#23415 = CARTESIAN_POINT ( 'NONE',  ( 814.8207195650702488, -98.19088175424404596, 336.2433038121456548 ) ) ;
#23416 = CIRCLE ( 'NONE', #21228, 8.024999999999948841 ) ;
#23418 = CARTESIAN_POINT ( 'NONE',  ( 759.9864689768902508, -194.0891481129654039, -354.9819416627836404 ) ) ;
#23417 = DIRECTION ( 'NONE',  ( 0.000000000000000000, 0.000000000000000000, 1.000000000000000000 ) ) ;
#23419 = CARTESIAN_POINT ( 'NONE',  ( 758.6633372737375112, -356.5328690171410813, -326.9102291470432533 ) ) ;
#23420 = CARTESIAN_POINT ( 'NONE',  ( 773.7305795820266212, -225.2817908451527273, -374.8230680027170365 ) ) ;
#23421 = PLANE ( 'NONE',  #28175 ) ;
#23422 = DIRECTION ( 'NONE',  ( 0.000000000000000000, 0.000000000000000000, -1.000000000000000000 ) ) ;
#23423 = CARTESIAN_POINT ( 'NONE',  ( 787.5531968255692163, -69.82724539060775726, -316.1348686366205811 ) ) ;
#23424 = CARTESIAN_POINT ( 'NONE',  ( 761.4292242960306112, -425.4636090269703459, 323.2154366446414429 ) ) ;
#23425 = FACE_OUTER_BOUND ( 'NONE', #43616, .T. ) ;
#23426 = CARTESIAN_POINT ( 'NONE',  ( 799.4546378042377910, -417.0783235625954148, -356.1575198192848006 ) ) ;
#23427 = CARTESIAN_POINT ( 'NONE',  ( 751.9810565676468741, -266.0891481129651197, -360.9747183278973921 ) ) ;
#23428 = CARTESIAN_POINT ( 'NONE',  ( -786.4999999999993179, -512.9681489794448908, -329.9999999999999432 ) ) ;
#23429 = DIRECTION ( 'NONE',  ( 1.000000000000000000, 0.000000000000000000, 0.000000000000000000 ) ) ;
#23430 = CARTESIAN_POINT ( 'NONE',  ( 801.9419747391806368, -66.45278447660216159, -351.9812246680014027 ) ) ;
#23431 = CARTESIAN_POINT ( 'NONE',  ( 760.0363995740630116, -202.9181544815164386, 368.7758568127991907 ) ) ;
#23432 = CARTESIAN_POINT ( 'NONE',  ( 807.5423716828161105, -153.0783235625962675, -362.2119215644372048 ) ) ;
#23433 = CARTESIAN_POINT ( 'NONE',  ( 787.4397851343537695, -165.7255117493291152, 374.2001403089903988 ) ) ;
#23434 = CARTESIAN_POINT ( 'NONE',  ( 745.0891759886404770, -412.2709662947829088, -342.4968714119734159 ) ) ;
#23435 = CARTESIAN_POINT ( 'NONE',  ( 571.1634899080285095, 259.9999999999999432, -199.9999999999981526 ) ) ;
#23436 = CARTESIAN_POINT ( 'NONE',  ( 757.8323909638827445, -242.6346026584197659, 352.1044303154654358 ) ) ;
#23437 = CARTESIAN_POINT ( 'NONE',  ( 800.9840315886518738, -52.91815448151692891, 354.1144889064786412 ) ) ;
#23438 = CARTESIAN_POINT ( 'NONE',  ( 771.1735550268778070, -441.1800572038735027, -316.3353852180827630 ) ) ;
#23439 = DIRECTION ( 'NONE',  ( 1.880165489482579047E-16, 1.000000000000000000, -0.000000000000000000 ) ) ;
#23440 = DIRECTION ( 'NONE',  ( 1.000000000000000000, 0.000000000000000000, 0.000000000000000000 ) ) ;
#23441 = CARTESIAN_POINT ( 'NONE',  ( 804.1601925771018387, -103.4419599262327836, 346.5483106153029098 ) ) ;
#23442 = ORIENTED_EDGE ( 'NONE', *, *, #31181, .T. ) ;
#23443 = CARTESIAN_POINT ( 'NONE',  ( 761.2382568024794409, -231.6237781080504874, -356.9571628226838129 ) ) ;
#23444 = CARTESIAN_POINT ( 'NONE',  ( 781.7834795799800531, -130.8164208402383224, -315.0636971347436202 ) ) ;
#23445 = CARTESIAN_POINT ( 'NONE',  ( 758.0580252608178853, -54.45278447660219001, 328.0187753319985404 ) ) ;
#23446 = CARTESIAN_POINT ( 'NONE',  ( 761.9338519418445230, -254.5328690171413655, -370.4231160770881957 ) ) ;
#23447 = LINE ( 'NONE', #26246, #21655 ) ;
#23448 = CARTESIAN_POINT ( 'NONE',  ( 747.3154664389472828, -379.9874144716865203, 326.4474001241230781 ) ) ;
#23449 = ORIENTED_EDGE ( 'NONE', *, *, #4417, .F. ) ;
#23450 = CARTESIAN_POINT ( 'NONE',  ( 810.7187646348534145, 5.547215523397618142, 356.7737145352016341 ) ) ;
#23451 = CARTESIAN_POINT ( 'NONE',  ( 791.9812246680005501, -188.6346026584199365, -361.9419747391813189 ) ) ;
#23452 = CARTESIAN_POINT ( 'NONE',  ( 791.9812246680005501, -380.6346026584192828, 361.9419747391813189 ) ) ;
#23453 = CARTESIAN_POINT ( 'NONE',  ( 772.4837098697144029, -119.3618753856928691, -374.5518280994205611 ) ) ;
#23454 = EDGE_CURVE ( 'NONE', #38198, #10343, #21823, .T. ) ;
#23455 = CARTESIAN_POINT ( 'NONE',  ( 788.7366044899766848, -59.90732993114762905, -316.5762568750059813 ) ) ;
#23456 = ORIENTED_EDGE ( 'NONE', *, *, #34274, .F. ) ;
#23457 = CARTESIAN_POINT ( 'NONE',  ( 766.0291762391763086, -34.91815448151697154, -360.7704444035551319 ) ) ;
#23458 = EDGE_LOOP ( 'NONE', ( #35670, #1680, #28111 ) ) ;
#23459 = CARTESIAN_POINT ( 'NONE',  ( 755.1538015810308480, -350.1908817542433212, -343.0433043558613804 ) ) ;
#23461 = CARTESIAN_POINT ( 'NONE',  ( 783.0745993439762742, -416.1908817542430938, 365.1016975059196739 ) ) ;
#23460 = CARTESIAN_POINT ( 'NONE',  ( 788.7366044899766848, -83.90732993114754379, 316.5762568750059813 ) ) ;
#23462 = CARTESIAN_POINT ( 'NONE',  ( 786.6156483768007774, -97.44195992623281199, 315.5913626894246136 ) ) ;
#23465 = CARTESIAN_POINT ( 'NONE',  ( 800.1688906516307043, -370.1692326535045936, 369.0717654672308186 ) ) ;
#23464 = LINE ( 'NONE', #5237, #12940 ) ;
#23463 = CARTESIAN_POINT ( 'NONE',  ( 800.9747183278959710, -444.9982390220554862, 311.9810565676471583 ) ) ;
#23466 = CARTESIAN_POINT ( 'NONE',  ( 755.3028492785439312, -327.2817908451525000, -335.9200461376539693 ) ) ;
#23467 = CARTESIAN_POINT ( 'NONE',  ( 804.6798772138708955, -327.7255117493285184, -334.6312213355107019 ) ) ;
#23468 = CARTESIAN_POINT ( 'NONE',  ( 752.7379699480933368, -132.0090635724257595, -361.9858362298580232 ) ) ;
#23469 = CARTESIAN_POINT ( 'NONE',  ( 814.8207195650702488, -2.190881754244347945, 336.2433038121456548 ) ) ;
#23471 = CARTESIAN_POINT ( 'NONE',  ( 51.16348990802859475, 240.0000000000000568, -197.2499999999946851 ) ) ;
#23470 = CARTESIAN_POINT ( 'NONE',  ( 200.7583438952258916, 294.6698570112193920, -274.9999999999999432 ) ) ;
#23472 = CARTESIAN_POINT ( 'NONE',  ( 766.7756240680305382, -254.5328690171413655, -361.5560724626415663 ) ) ;
#23473 = CARTESIAN_POINT ( 'NONE',  ( 809.0717654672305343, -124.9181544815167086, -360.1688906516309885 ) ) ;
#23474 = CARTESIAN_POINT ( 'NONE',  ( -949.5497976682736407, 240.0000000000002274, 339.9999999999998863 ) ) ;
#23475 = DIRECTION ( 'NONE',  ( -0.000000000000000000, 1.000000000000000000, -0.000000000000000000 ) ) ;
#23476 = CARTESIAN_POINT ( 'NONE',  ( 766.9102291470427417, -330.5545181178796952, 318.6633372737382501 ) ) ;
#23477 = ORIENTED_EDGE ( 'NONE', *, *, #3549, .F. ) ;
#23478 = CARTESIAN_POINT ( 'NONE',  ( 807.2620300519052989, -312.0090635724251911, 318.0141637701419768 ) ) ;
#23479 = CARTESIAN_POINT ( 'NONE',  ( 758.8095938919644823, -176.0891481129654039, -311.6929314249762797 ) ) ;
#23480 = CARTESIAN_POINT ( 'NONE',  ( 794.9999999999993179, 205.0000000000000568, -274.9999999999999432 ) ) ;
#23481 = VECTOR ( 'NONE', #34912, 1000.000000000000000 ) ;
#23482 = CARTESIAN_POINT ( 'NONE',  ( 805.6418435158337843, -101.4636090269713264, 363.8556311672236916 ) ) ;
#23483 = CARTESIAN_POINT ( 'NONE',  ( 812.7932403749906598, -303.1800572038740711, -327.7687537140311633 ) ) ;
#23484 = EDGE_CURVE ( 'NONE', #18090, #24825, #5593, .T. ) ;
#23485 = LINE ( 'NONE', #38285, #35532 ) ;
#23486 = CARTESIAN_POINT ( 'NONE',  ( 792.1044303154645831, -156.4527844766018916, 317.8323909638837677 ) ) ;
#23487 = ORIENTED_EDGE ( 'NONE', *, *, #8323, .F. ) ;
#23488 = CARTESIAN_POINT ( 'NONE',  ( 748.6759233522253680, -424.3726999360612808, 324.3348316497537098 ) ) ;
#23489 = CARTESIAN_POINT ( 'NONE',  ( 813.9316612368132837, -343.4419599262320162, -348.6739635108323228 ) ) ;
#23490 = CARTESIAN_POINT ( 'NONE',  ( 800.9747183278959710, -132.9982390220564810, -311.9810565676471583 ) ) ;
#23491 = CARTESIAN_POINT ( 'NONE',  ( 779.4763451958990572, -56.73633629969872771, 365.0264073115438919 ) ) ;
#23492 = CARTESIAN_POINT ( 'NONE',  ( 767.7687537140311633, -383.9073299311466485, -372.7932403749916830 ) ) ;
#23493 = LINE ( 'NONE', #41300, #24677 ) ;
#23494 = CARTESIAN_POINT ( 'NONE',  ( 759.8311093483677041, 25.83076734649409545, 310.9282345327691814 ) ) ;
#23495 = ORIENTED_EDGE ( 'NONE', *, *, #16791, .T. ) ;
#23496 = CARTESIAN_POINT ( 'NONE',  ( 799.4546378042377910, -81.07832356259649487, 356.1575198192848006 ) ) ;
#23497 = CARTESIAN_POINT ( 'NONE',  ( 798.0661480581538854, -170.5328690171416781, -309.5768839229118043 ) ) ;
#23498 = CARTESIAN_POINT ( 'NONE',  ( 959.5497976682736407, 229.9999999999998579, -122.7905160835440768 ) ) ;
#23499 = CARTESIAN_POINT ( 'NONE',  ( 805.9055244015594326, -267.6237781080504305, 315.8990559732753240 ) ) ;
#23500 = CARTESIAN_POINT ( 'NONE',  ( 802.1676090361155502, -86.63460265842024910, 327.8955696845344505 ) ) ;
#23501 = ORIENTED_EDGE ( 'NONE', *, *, #33439, .F. ) ;
#23502 = CARTESIAN_POINT ( 'NONE',  ( 802.1676090361156639, -254.6346026584196238, 327.8955696845344505 ) ) ;
#23503 = CARTESIAN_POINT ( 'NONE',  ( 798.0661480581538854, -434.5328690171407970, -309.5768839229118043 ) ) ;
#23504 = ADVANCED_FACE ( 'NONE', ( #10520, #24595, #21155 ), #10999, .F. ) ;
#23505 = DIRECTION ( 'NONE',  ( 0.000000000000000000, 1.000000000000000000, 0.000000000000000000 ) ) ;
#23506 = VERTEX_POINT ( 'NONE', #4297 ) ;
#23507 = CARTESIAN_POINT ( 'NONE',  ( 786.2694204179717872, -381.2817908451523294, -305.1769319972829067 ) ) ;
#23508 = CIRCLE ( 'NONE', #42002, 6.118999999999985562 ) ;
#23509 = CARTESIAN_POINT ( 'NONE',  ( 801.9419747391806368, -234.4527844766016358, -351.9812246680014027 ) ) ;
#23511 = CARTESIAN_POINT ( 'NONE',  ( 788.7631598425961101, -265.4419599262323004, 305.7194118038759143 ) ) ;
#23510 = CARTESIAN_POINT ( 'NONE',  ( 772.4837098697145166, -335.3618753856921444, 374.5518280994205611 ) ) ;
#23512 = CARTESIAN_POINT ( 'NONE',  ( 763.8424801807145741, -234.0090635724255037, -320.5453621957614700 ) ) ;
#23513 = CARTESIAN_POINT ( 'NONE',  ( 785.3687786644884454, -227.3618753856925707, -315.3201227861279676 ) ) ;
#23514 = CARTESIAN_POINT ( 'NONE',  ( 804.6798772138710092, -423.7255117493282341, -334.6312213355106451 ) ) ;
#23515 = CARTESIAN_POINT ( 'NONE',  ( 758.0580252608178853, -198.4527844766017495, 328.0187753319985404 ) ) ;
#23516 = CARTESIAN_POINT ( 'NONE',  ( 781.7834795799800531, -106.8164208402383935, -315.0636971347436202 ) ) ;
#23517 = ORIENTED_EDGE ( 'NONE', *, *, #44081, .F. ) ;
#23518 = CARTESIAN_POINT ( 'NONE',  ( 777.4774526936600978, -346.2709662947830793, 304.7301800767027657 ) ) ;
#23519 = LINE ( 'NONE', #33927, #35133 ) ;
#23520 = CARTESIAN_POINT ( 'NONE',  ( 762.3223304703356007, 16.45630643248849267, 322.3223304703362828 ) ) ;
#23521 = DIRECTION ( 'NONE',  ( 0.000000000000000000, 0.000000000000000000, 1.000000000000000000 ) ) ;
#23522 = ADVANCED_FACE ( 'NONE', ( #31991 ), #14224, .F. ) ;
#23523 = CARTESIAN_POINT ( 'NONE',  ( 755.8894580844503253, -231.8272453906072315, 332.3691319403863531 ) ) ;
#23524 = CARTESIAN_POINT ( 'NONE',  ( 774.6858677611749044, -81.72551174932937101, 315.5713283507209894 ) ) ;
#23525 = ORIENTED_EDGE ( 'NONE', *, *, #12291, .T. ) ;
#23526 = CARTESIAN_POINT ( 'NONE',  ( 793.5525998758768083, -439.0999726633339719, -372.6845335610516941 ) ) ;
#23527 = CARTESIAN_POINT ( 'NONE',  ( 747.2067596250078623, -75.18005720387485269, -352.2312462859687230 ) ) ;
#23528 = CARTESIAN_POINT ( 'NONE',  ( 798.7617431975189675, -267.6237781080504305, 323.0428371773161871 ) ) ;
#23529 = CARTESIAN_POINT ( 'NONE',  ( 804.9363028652555840, -424.2709662947829088, -338.2165204200192079 ) ) ;
#23530 = CARTESIAN_POINT ( 'NONE',  ( 778.1981804954715471, -34.27096629478407408, -314.8072714833591021 ) ) ;
#23531 = CARTESIAN_POINT ( 'NONE',  ( 745.1792804349281596, -14.19088175424431242, 343.7566961878542884 ) ) ;
#23532 = CARTESIAN_POINT ( 'NONE',  ( 781.7834795799800531, 13.18357915976123174, -315.0636971347436202 ) ) ;
#23533 = CARTESIAN_POINT ( 'NONE',  ( 804.8461984189677878, -290.1908817542434349, -336.9566956441385628 ) ) ;
#23534 = CARTESIAN_POINT ( 'NONE',  ( 777.4774526936600978, -202.2709662947834772, -304.7301800767027657 ) ) ;
#23535 = EDGE_CURVE ( 'NONE', #39949, #30067, #41016, .T. ) ;
#23536 = CARTESIAN_POINT ( 'NONE',  ( 763.0537975583475827, -96.45278447660203369, 371.0346526505627480 ) ) ;
#23537 = CARTESIAN_POINT ( 'NONE',  ( 796.7737145352015204, -140.6346026584201070, 370.7187646348536987 ) ) ;
#23538 = CARTESIAN_POINT ( 'NONE',  ( -728.8365100919714905, 240.0000000000001990, -199.9999999999890861 ) ) ;
#23539 = CARTESIAN_POINT ( 'NONE',  ( 810.1134526219336749, -224.5328690171415076, -357.8822607201570349 ) ) ;
#23540 = VECTOR ( 'NONE', #13264, 1000.000000000000000 ) ;
#23541 = CARTESIAN_POINT ( 'NONE',  ( 766.4474001241216001, -403.0999726633339719, 307.3154664389482491 ) ) ;
#23542 = CARTESIAN_POINT ( 'NONE',  ( 751.9810565676468741, -290.0891481129650629, -360.9747183278973921 ) ) ;
#23543 = LINE ( 'NONE', #23082, #33876 ) ;
#23544 = CARTESIAN_POINT ( 'NONE',  ( 801.1904061080336987, -380.0891481129646650, 368.3070685750235498 ) ) ;
#23545 = CARTESIAN_POINT ( 'NONE',  ( 782.5225473063383106, 1.729033705215812233, 375.2698199232970637 ) ) ;
#23546 = CARTESIAN_POINT ( 'NONE',  ( 792.1044303154645831, -348.4527844766012663, -317.8323909638837677 ) ) ;
#23547 = CARTESIAN_POINT ( 'NONE',  ( 759.2295555964440155, -16.16923265350578021, 353.9708237608231229 ) ) ;
#23548 = CARTESIAN_POINT ( 'NONE',  ( 745.5313806188320314, -87.28179084515316788, -333.7943932421247268 ) ) ;
#23549 = CARTESIAN_POINT ( 'NONE',  ( 795.9930595647434757, -171.0783235625962106, -320.7433823573372820 ) ) ;
#23550 = EDGE_CURVE ( 'NONE', #36814, #2255, #7838, .T. ) ;
#23551 = CARTESIAN_POINT ( 'NONE',  ( 766.5853460496234675, -157.9874144716871456, 372.3518521366060554 ) ) ;
#23552 = CARTESIAN_POINT ( 'NONE',  ( 786.4999999999993179, -563.3203001761230553, -342.3463313526983143 ) ) ;
#23553 = EDGE_CURVE ( 'NONE', #19003, #21254, #25520, .T. ) ;
#23554 = EDGE_LOOP ( 'NONE', ( #8928, #21651 ) ) ;
#23555 = CARTESIAN_POINT ( 'NONE',  ( 794.9819416627830151, -60.99823902205671544, -319.9864689768909898 ) ) ;
#23556 = CARTESIAN_POINT ( 'NONE',  ( 796.7845633553578182, -153.6237781080508000, -358.5707757039688204 ) ) ;
#23557 = CARTESIAN_POINT ( 'NONE',  ( 756.5762568750052424, -147.1800572038746395, 348.7366044899774238 ) ) ;
#23558 = CARTESIAN_POINT ( 'NONE',  ( 810.1134526219336749, 15.46713098285775878, -357.8822607201570349 ) ) ;
#23559 = CARTESIAN_POINT ( 'NONE',  ( 755.5713283507202505, -293.3618753856923718, 334.6858677611754729 ) ) ;
#23560 = EDGE_CURVE ( 'NONE', #34305, #2122, #17416, .T. ) ;
#23561 = DIRECTION ( 'NONE',  ( -0.000000000000000000, 1.000000000000000000, -0.000000000000000000 ) ) ;
#23562 = ORIENTED_EDGE ( 'NONE', *, *, #7983, .T. ) ;
#23563 = CARTESIAN_POINT ( 'NONE',  ( 793.2243759319678702, -2.532869017142183932, 318.4439275373583200 ) ) ;
#23564 = CARTESIAN_POINT ( 'NONE',  ( 757.7880784355613741, -258.0090635724253616, -312.4576283171834916 ) ) ;
#23565 = VERTEX_POINT ( 'NONE', #17704 ) ;
#23566 = DIRECTION ( 'NONE',  ( 1.000000000000000000, 0.000000000000000000, 0.000000000000000000 ) ) ;
#23567 = CARTESIAN_POINT ( 'NONE',  ( 805.0032342141413437, -205.5436935675108145, 314.9967657858572352 ) ) ;
#23568 = CARTESIAN_POINT ( 'NONE',  ( 805.2837595273609850, -338.7363362996978822, 340.5290396650784714 ) ) ;
#23569 = CARTESIAN_POINT ( 'NONE',  ( 780.5290396650775619, -420.3510508353225532, 365.2837595273619513 ) ) ;
#23570 = ORIENTED_EDGE ( 'NONE', *, *, #35112, .T. ) ;
#23571 = CARTESIAN_POINT ( 'NONE',  ( 760.7433823573367135, -108.0090635724258448, -355.9930595647440441 ) ) ;
#23572 = CARTESIAN_POINT ( 'NONE',  ( 803.4237431249931660, -111.1800572038747532, -331.2633955100225194 ) ) ;
#23573 = CARTESIAN_POINT ( 'NONE',  ( 804.4286716492782716, -305.3618753856922581, -345.3141322388244703 ) ) ;
#23574 = ORIENTED_EDGE ( 'NONE', *, *, #37138, .T. ) ;
#23575 = CARTESIAN_POINT ( 'NONE',  ( 794.9819416627830151, -444.9982390220554862, -319.9864689768909898 ) ) ;
#23576 = ADVANCED_FACE ( 'NONE', ( #817 ), #39868, .T. ) ;
#23577 = CARTESIAN_POINT ( 'NONE',  ( 798.7617431975189675, -315.6237781080503169, 323.0428371773161871 ) ) ;
#23578 = CARTESIAN_POINT ( 'NONE',  ( 793.4459926374332781, -455.5444164708248422, 371.6295267004306879 ) ) ;
#23579 = DIRECTION ( 'NONE',  ( 0.000000000000000000, -1.000000000000000000, -0.000000000000000000 ) ) ;
#23580 = ADVANCED_FACE ( 'NONE', ( #14917 ), #32693, .F. ) ;
#23581 = CARTESIAN_POINT ( 'NONE',  ( 798.5707757039680246, -125.4636090269712412, 356.7845633553585003 ) ) ;
#23582 = CARTESIAN_POINT ( 'NONE',  ( 800.0135310231082713, 9.910851887033969021, 325.0180583372163028 ) ) ;
#23583 = VERTEX_POINT ( 'NONE', #21386 ) ;
#23584 = CARTESIAN_POINT ( 'NONE',  ( 788.6739635108323228, -343.6454272087887603, -373.9316612368139090 ) ) ;
#23585 = CARTESIAN_POINT ( 'NONE',  ( 762.1177392798416577, -210.5545181178800647, 309.8865473780659272 ) ) ;
#23586 = CARTESIAN_POINT ( 'NONE',  ( 756.5762568750052424, -339.1800572038740142, -348.7366044899774238 ) ) ;
#23587 = DIRECTION ( 'NONE',  ( 0.000000000000000000, 0.000000000000000000, 1.000000000000000000 ) ) ;
#23588 = CARTESIAN_POINT ( 'NONE',  ( 804.8461984189677878, -170.1908817542438328, -336.9566956441385628 ) ) ;
#23589 = CARTESIAN_POINT ( 'NONE',  ( 808.0189434323515343, -62.08914811296580183, 319.0252816721025511 ) ) ;
#23590 = CARTESIAN_POINT ( 'NONE',  ( 809.0082352070306797, -452.9681489794448908, 335.5949598064873385 ) ) ;
#23591 = CARTESIAN_POINT ( 'NONE',  ( 747.2067596250078623, -387.1800572038738437, -352.2312462859687230 ) ) ;
#23592 = CARTESIAN_POINT ( 'NONE',  ( 779.9999999999992042, -462.9681489794448339, 339.9999999999999432 ) ) ;
#23593 = CARTESIAN_POINT ( 'NONE',  ( 746.4236121716829757, -303.8272453906071178, 328.8385539511384650 ) ) ;
#23594 = CYLINDRICAL_SURFACE ( 'NONE', #43416, 9.999999999999980460 ) ;
#23595 = CARTESIAN_POINT ( 'NONE',  ( 814.5518280994195948, -303.7255117493287457, 332.4837098697145734 ) ) ;
#23596 = CARTESIAN_POINT ( 'NONE',  ( 744.7301800767019131, -4.816420840238714085, -337.4774526936615757 ) ) ;
#23597 = CARTESIAN_POINT ( 'NONE',  ( 788.8264449731200330, -237.1800572038742985, -363.6646147819171233 ) ) ;
#23598 = DIRECTION ( 'NONE',  ( -1.000000000000000000, 0.000000000000000000, 0.000000000000000000 ) ) ;
#23599 = CARTESIAN_POINT ( 'NONE',  ( 778.1981804954714335, -394.2709662947827951, 314.8072714833589885 ) ) ;
#23600 = CARTESIAN_POINT ( 'NONE',  ( 758.4439275373578084, -132.5545181178802920, 353.2243759319684386 ) ) ;
#23601 = CARTESIAN_POINT ( 'NONE',  ( 795.9930595647434757, -51.07832356259657303, -320.7433823573372820 ) ) ;
#23602 = CARTESIAN_POINT ( 'NONE',  ( 745.1769319972822814, -65.80559628986925702, 346.2694204179732083 ) ) ;
#23603 = CARTESIAN_POINT ( 'NONE',  ( 785.3687786644885591, -371.3618753856920307, 315.3201227861280813 ) ) ;
#23604 = DIRECTION ( 'NONE',  ( -0.000000000000000000, -0.000000000000000000, 1.000000000000000000 ) ) ;
#23605 = CARTESIAN_POINT ( 'NONE',  ( 779.9999999999992042, -462.9681489794448339, 339.9999999999999432 ) ) ;
#23606 = CARTESIAN_POINT ( 'NONE',  ( 803.4237431249931660, -423.1800572038737300, 331.2633955100225194 ) ) ;
#23607 = ORIENTED_EDGE ( 'NONE', *, *, #43619, .T. ) ;
#23608 = CARTESIAN_POINT ( 'NONE',  ( 803.6646147819161570, -65.90732993114758642, -348.8264449731210561 ) ) ;
#23609 = CARTESIAN_POINT ( 'NONE',  ( 764.0069404352550464, -375.0783235625955285, -359.2566176426627180 ) ) ;
#23611 = CARTESIAN_POINT ( 'NONE',  ( 803.4237431249931660, -207.1800572038744406, 331.2633955100225194 ) ) ;
#23610 = CARTESIAN_POINT ( 'NONE',  ( 754.8072714833581358, -196.8164208402380950, 338.1981804954720587 ) ) ;
#23612 = CARTESIAN_POINT ( 'NONE',  ( 745.1769319972822814, -353.8055962898683333, -346.2694204179732083 ) ) ;
#23613 = CARTESIAN_POINT ( 'NONE',  ( 831.1634899080286232, 259.9999999999998863, -199.9999999999999432 ) ) ;
#23614 = ORIENTED_EDGE ( 'NONE', *, *, #26674, .T. ) ;
#23615 = CARTESIAN_POINT ( 'NONE',  ( 765.0180583372156207, -384.9982390220556567, 360.0135310231089534 ) ) ;
#23616 = ORIENTED_EDGE ( 'NONE', *, *, #640, .F. ) ;
#23617 = CARTESIAN_POINT ( 'NONE',  ( 745.0891759886404770, -220.2709662947834772, -342.4968714119734159 ) ) ;
#23618 = CARTESIAN_POINT ( 'NONE',  ( 782.4968714119720516, -106.8164208402383935, 305.0891759886411023 ) ) ;
#23619 = VERTEX_POINT ( 'NONE', #35459 ) ;
#23620 = CARTESIAN_POINT ( 'NONE',  ( 781.8018195045267476, -214.2709662947834772, -365.1927285166407273 ) ) ;
#23621 = ORIENTED_EDGE ( 'NONE', *, *, #21836, .T. ) ;
#23622 = CARTESIAN_POINT ( 'NONE',  ( 767.8955696845333705, -312.4527844766012663, -362.1676090361162323 ) ) ;
#23623 = CARTESIAN_POINT ( 'NONE',  ( 757.4527132478984868, -448.3726999360611103, -329.1273215169538844 ) ) ;
#23624 = CARTESIAN_POINT ( 'NONE',  ( 751.6929314249748586, -270.9982390220561115, 318.8095938919659034 ) ) ;
#23625 = CARTESIAN_POINT ( 'NONE',  ( 780.5290396650775619, -204.3510508353233774, 365.2837595273619513 ) ) ;
#23627 = DIRECTION ( 'NONE',  ( 0.000000000000000000, 0.000000000000000000, -1.000000000000000000 ) ) ;
#23626 = CARTESIAN_POINT ( 'NONE',  ( 809.4421496042219815, -454.3218287316016699, 345.7584569706272077 ) ) ;
#23628 = DIRECTION ( 'NONE',  ( 1.892425610156518354E-16, 1.000000000000000000, -0.000000000000000000 ) ) ;
#23629 = ORIENTED_EDGE ( 'NONE', *, *, #15427, .F. ) ;
#23630 = CARTESIAN_POINT ( 'NONE',  ( 799.2566176426618085, -456.0090635724247932, -324.0069404352559559 ) ) ;
#23631 = DIRECTION ( 'NONE',  ( 0.000000000000000000, 0.000000000000000000, 1.000000000000000000 ) ) ;
#23632 = CARTESIAN_POINT ( 'NONE',  ( 199.6009925648704098, 290.0000000000001137, -274.9999999999999432 ) ) ;
#23633 = ORIENTED_EDGE ( 'NONE', *, *, #43019, .F. ) ;
#23634 = CARTESIAN_POINT ( 'NONE',  ( 795.8262568251477660, -238.3726999360617640, -308.3538107759623585 ) ) ;
#23635 = CARTESIAN_POINT ( 'NONE',  ( 799.9636004259356241, -94.91815448151677970, 311.2241431872006956 ) ) ;
#23637 = CARTESIAN_POINT ( 'NONE',  ( 805.1927285166397041, -208.8164208402380666, -341.8018195045277707 ) ) ;
#23636 = DIRECTION ( 'NONE',  ( -0.000000000000000000, 1.000000000000000000, -0.000000000000000000 ) ) ;
#23638 = CARTESIAN_POINT ( 'NONE',  ( 794.1144889064781864, -370.1692326535045936, -360.9840315886528401 ) ) ;
#23639 = CARTESIAN_POINT ( 'NONE',  ( 764.1737431748507561, -250.3726999360618208, -371.6461892240376415 ) ) ;
#23640 = DIRECTION ( 'NONE',  ( 0.000000000000000000, 0.000000000000000000, 1.000000000000000000 ) ) ;
#23641 = DIRECTION ( 'NONE',  ( 0.000000000000000000, 0.000000000000000000, 1.000000000000000000 ) ) ;
#23642 = CARTESIAN_POINT ( 'NONE',  ( 786.5483106153019435, -79.64542720878957027, -364.1601925771022366 ) ) ;
#23643 = CARTESIAN_POINT ( 'NONE',  ( 757.0176451133909268, -445.0999726633338582, 349.9200121543848354 ) ) ;
#23644 = CARTESIAN_POINT ( 'NONE',  ( 815.3608509340175488, -362.7363362996977116, 341.2497674668889545 ) ) ;
#23645 = CARTESIAN_POINT ( 'NONE',  ( 187.1337867209877857, -190.2822455671962985, -69.00746428064726956 ) ) ;
#23646 = CARTESIAN_POINT ( 'NONE',  ( 805.0264073115434940, -438.3510508353226669, -339.4763451958999099 ) ) ;
#23647 = CARTESIAN_POINT ( 'NONE',  ( 746.8695393053151292, -269.9073299311469327, -327.6429770376306578 ) ) ;
#23648 = DIRECTION ( 'NONE',  ( 0.000000000000000000, 0.7517448203044204691, -0.6594541114781790059 ) ) ;
#23649 = LINE ( 'NONE', #20431, #32765 ) ;
#23650 = CARTESIAN_POINT ( 'NONE',  ( 767.8955696845333705, -48.45278447660219712, -362.1676090361162323 ) ) ;
#23651 = CARTESIAN_POINT ( 'NONE',  ( 797.8822607201568644, -222.5545181178800362, 370.1134526219340160 ) ) ;
#23652 = CARTESIAN_POINT ( 'NONE',  ( 795.6651683502461765, -154.7146871989598935, -371.3240766477733814 ) ) ;
#23653 = CARTESIAN_POINT ( 'NONE',  ( 782.5225473063381969, -190.2709662947835909, 375.2698199232970637 ) ) ;
#23654 = CARTESIAN_POINT ( 'NONE',  ( 796.9462024416508257, -396.4527844766010389, -308.9653473494370246 ) ) ;
#23655 = DIRECTION ( 'NONE',  ( 0.000000000000000000, -1.000000000000000000, 0.000000000000000000 ) ) ;
#23656 = CARTESIAN_POINT ( 'NONE',  ( 755.5713283507202505, -269.3618753856924286, 334.6858677611754729 ) ) ;
#23657 = CARTESIAN_POINT ( 'NONE',  ( 780.5236548040995785, -68.73633629969867798, 314.9735926884559944 ) ) ;
#23658 = CARTESIAN_POINT ( 'NONE',  ( 755.3201227861273992, -435.7255117493282341, -345.3687786644892981 ) ) ;
#23659 = DIRECTION ( 'NONE',  ( -0.000000000000000000, 1.000000000000000000, -0.000000000000000000 ) ) ;
#23660 = DIRECTION ( 'NONE',  ( -0.000000000000000000, 1.000000000000000000, -0.000000000000000000 ) ) ;
#23662 = CARTESIAN_POINT ( 'NONE',  ( 755.5713283507202505, -341.3618753856922012, 334.6858677611754729 ) ) ;
#23661 = CARTESIAN_POINT ( 'NONE',  ( 775.9200461376533440, -95.80559628986917176, 315.3028492785443291 ) ) ;
#23663 = ORIENTED_EDGE ( 'NONE', *, *, #30014, .F. ) ;
#23664 = CARTESIAN_POINT ( 'NONE',  ( 763.2154366446407039, -261.6237781080504305, -321.4292242960311228 ) ) ;
#23665 = CARTESIAN_POINT ( 'NONE',  ( 755.3201227861273992, -75.72551174932937101, 345.3687786644892981 ) ) ;
#23666 = CARTESIAN_POINT ( 'NONE',  ( 805.9055244015594326, -267.6237781080504305, -315.8990559732753240 ) ) ;
#23667 = LINE ( 'NONE', #9142, #258 ) ;
#23668 = CARTESIAN_POINT ( 'NONE',  ( 788.7631598425961101, -385.4419599262319593, 305.7194118038759143 ) ) ;
#23669 = VERTEX_POINT ( 'NONE', #28775 ) ;
#23670 = CARTESIAN_POINT ( 'NONE',  ( 797.8594530101008786, -301.5436935675105588, 322.1405469898980982 ) ) ;
#23671 = CARTESIAN_POINT ( 'NONE',  ( 812.7932403749906598, 8.819942796124882634, 327.7687537140311633 ) ) ;
#23672 = CARTESIAN_POINT ( 'NONE',  ( 789.9200121543843807, -25.98741447168755769, -317.0176451133914384 ) ) ;
#23673 = CARTESIAN_POINT ( 'NONE',  ( 757.8323909638827445, -170.6346026584199649, -352.1044303154654358 ) ) ;
#23674 = CARTESIAN_POINT ( 'NONE',  ( 801.9419747391806368, -378.4527844766011526, 351.9812246680014027 ) ) ;
#23675 = CARTESIAN_POINT ( 'NONE',  ( 755.2512626584698410, -127.5436935675110561, -315.2512626584710915 ) ) ;
#23676 = CIRCLE ( 'NONE', #14110, 30.00000000000008171 ) ;
#23677 = CARTESIAN_POINT ( 'NONE',  ( 802.1676090361155502, -110.6346026584201923, -327.8955696845344505 ) ) ;
#23678 = EDGE_LOOP ( 'NONE', ( #37906, #26507, #19424, #40923 ) ) ;
#23679 = CARTESIAN_POINT ( 'NONE',  ( 755.3028492785439312, -39.28179084515331709, -335.9200461376539693 ) ) ;
#23680 = CARTESIAN_POINT ( 'NONE',  ( 779.4763451958990572, -344.7363362996978253, -365.0264073115438919 ) ) ;
#23682 = CARTESIAN_POINT ( 'NONE',  ( 776.9254006560222479, -404.1908817542431507, 314.8983024940802125 ) ) ;
#23681 = CARTESIAN_POINT ( 'NONE',  ( 755.3201227861273992, -99.72551174932928575, 345.3687786644892981 ) ) ;
#23683 = CARTESIAN_POINT ( 'NONE',  ( 775.9200461376533440, -95.80559628986917176, 315.3028492785443291 ) ) ;
#23686 = CARTESIAN_POINT ( 'NONE',  ( 751.2241431872005251, -352.1692326535046504, 359.9636004259367610 ) ) ;
#23685 = DIRECTION ( 'NONE',  ( -0.000000000000000000, 1.000000000000000000, -0.000000000000000000 ) ) ;
#23684 = CARTESIAN_POINT ( 'NONE',  ( 813.1304606946831655, -449.9073299311464211, 352.3570229623691716 ) ) ;
#23687 = CARTESIAN_POINT ( 'NONE',  ( 744.8212110874229666, -114.8965053807782226, 336.2046728542121627 ) ) ;
#23688 = CARTESIAN_POINT ( 'NONE',  ( 784.1219089521767955, -357.2817908451523294, -315.0488828828318333 ) ) ;
#23689 = CARTESIAN_POINT ( 'NONE',  ( 781.7834795799800531, -322.8164208402377540, -315.0636971347436202 ) ) ;
#23690 = CARTESIAN_POINT ( 'NONE',  ( 814.4686193811664907, -147.2817908451529547, -346.2056067578752732 ) ) ;
#23691 = CARTESIAN_POINT ( 'NONE',  ( 796.9462024416508257, -444.4527844766009821, 308.9653473494370246 ) ) ;
#23693 = CARTESIAN_POINT ( 'NONE',  ( 767.9999999999992042, 240.0000000000000853, 320.0000000000000000 ) ) ;
#23692 = CARTESIAN_POINT ( 'NONE',  ( 775.4999999999993179, -355.4967352946684969, -16.45562775363632113 ) ) ;
#23694 = CARTESIAN_POINT ( 'NONE',  ( 786.6156483768007774, -265.4419599262323004, -315.5913626894246136 ) ) ;
#23695 = CARTESIAN_POINT ( 'NONE',  ( 781.2370466360911223, -140.7363362996984506, -304.9990715423533629 ) ) ;
#23696 = CYLINDRICAL_SURFACE ( 'NONE', #1986, 10.00000000000000888 ) ;
#23697 = CARTESIAN_POINT ( 'NONE',  ( 701.1634899080286232, 256.4999999999999432, -199.9999999999990337 ) ) ;
#23698 = CARTESIAN_POINT ( 'NONE',  ( 784.1219089521767955, -333.2817908451523863, 315.0488828828318333 ) ) ;
#23699 = ORIENTED_EDGE ( 'NONE', *, *, #32627, .F. ) ;
#23700 = CARTESIAN_POINT ( 'NONE',  ( 771.3260364891663130, -307.6454272087888171, 306.0683387631859773 ) ) ;
#23701 = CARTESIAN_POINT ( 'NONE',  ( 755.2512626584698410, -175.5436935675108998, -315.2512626584710915 ) ) ;
#23702 = DIRECTION ( 'NONE',  ( 0.000000000000000000, 0.000000000000000000, -1.000000000000000000 ) ) ;
#23703 = CARTESIAN_POINT ( 'NONE',  ( 813.5763878283155464, -99.82724539060768620, 351.1614460488615350 ) ) ;
#23704 = CARTESIAN_POINT ( 'NONE',  ( 754.9967657858570647, -313.5436935675102745, -365.0032342141425374 ) ) ;
#23705 = DIRECTION ( 'NONE',  ( 0.000000000000000000, 0.7517448203044204691, 0.6594541114781790059 ) ) ;
#23706 = CARTESIAN_POINT ( 'NONE',  ( -784.4999999999993179, -513.1383975375929367, -367.9999999999999432 ) ) ;
#23707 = APPLICATION_CONTEXT ( 'automotive_design' ) ;
#23708 = CARTESIAN_POINT ( 'NONE',  ( 755.5713283507202505, -149.3618753856928265, 334.6858677611754729 ) ) ;
#23709 = ORIENTED_EDGE ( 'NONE', *, *, #41497, .F. ) ;
#23710 = CARTESIAN_POINT ( 'NONE',  ( 804.1009440267234822, -431.4636090269702322, 314.0944755984392600 ) ) ;
#23711 = CARTESIAN_POINT ( 'NONE',  ( 815.1787889125755555, -390.8965053807772279, -343.7953271457877804 ) ) ;
#23712 = CARTESIAN_POINT ( 'NONE',  ( 777.4774526936600978, -130.2709662947837899, -304.7301800767027657 ) ) ;
#23713 = CARTESIAN_POINT ( 'NONE',  ( 793.9708237608222134, -46.91815448151694312, 319.2295555964448681 ) ) ;
#23714 = CARTESIAN_POINT ( 'NONE',  ( 754.9967657858570647, -385.5436935675102745, -365.0032342141425374 ) ) ;
#23715 = CARTESIAN_POINT ( 'NONE',  ( 784.4999999999993179, -857.0166862835568509, -63.94525337997358605 ) ) ;
#23716 = CARTESIAN_POINT ( 'NONE',  ( 788.7631598425961101, 22.55804007376682918, 305.7194118038759143 ) ) ;
#23717 = EDGE_LOOP ( 'NONE', ( #4226, #41991, #17970, #4186 ) ) ;
#23718 = CARTESIAN_POINT ( 'NONE',  ( 810.1134526219336749, -152.5328690171416781, -357.8822607201570349 ) ) ;
#23719 = CARTESIAN_POINT ( 'NONE',  ( 8.295132257852746908E-14, 200.0000000000001421, 350.0000000000000000 ) ) ;
#23720 = CARTESIAN_POINT ( 'NONE',  ( 815.1787889125755555, -270.8965053807777394, 343.7953271457877804 ) ) ;
#23721 = CARTESIAN_POINT ( 'NONE',  ( 754.8072714833583632, -100.8164208402383935, 338.1981804954721156 ) ) ;
#23722 = ORIENTED_EDGE ( 'NONE', *, *, #19325, .F. ) ;
#23723 = CARTESIAN_POINT ( 'NONE',  ( 786.6156483768007774, -1.441959926233096656, -315.5913626894246136 ) ) ;
#23724 = CARTESIAN_POINT ( 'NONE',  ( 800.0135310231082713, -278.0891481129651197, 325.0180583372163028 ) ) ;
#23725 = CARTESIAN_POINT ( 'NONE',  ( 800.9747183278959710, -12.99823902205686821, -311.9810565676471583 ) ) ;
#23726 = LINE ( 'NONE', #24645, #18036 ) ;
#23727 = ORIENTED_EDGE ( 'NONE', *, *, #23300, .T. ) ;
#23728 = ORIENTED_EDGE ( 'NONE', *, *, #13648, .T. ) ;
#23729 = CARTESIAN_POINT ( 'NONE',  ( 785.3687786644884454, -179.3618753856927128, -315.3201227861279676 ) ) ;
#23730 = CARTESIAN_POINT ( 'NONE',  ( 755.8990559732751535, -395.4636090269705164, -365.9055244015606831 ) ) ;
#23731 = CARTESIAN_POINT ( 'NONE',  ( 771.1735550268778070, -249.1800572038742416, -316.3353852180827630 ) ) ;
#23732 = EDGE_CURVE ( 'NONE', #34939, #8196, #39643, .T. ) ;
#23734 = CARTESIAN_POINT ( 'NONE',  ( 756.1443688327750579, -261.6237781080504305, 314.3581564841659315 ) ) ;
#23733 = CARTESIAN_POINT ( 'NONE',  ( 814.2001403089898304, -353.3618753856922012, 347.4397851343538264 ) ) ;
#23735 = CARTESIAN_POINT ( 'NONE',  ( 804.6971507214547046, -267.2817908451526137, -344.0799538623459739 ) ) ;
#23736 = CARTESIAN_POINT ( 'NONE',  ( 788.8264449731200330, -213.1800572038743553, -363.6646147819171233 ) ) ;
#23737 = CIRCLE ( 'NONE', #22270, 6.118999999999985562 ) ;
#23738 = CARTESIAN_POINT ( 'NONE',  ( 755.3201227861273992, -411.7255117493282910, -345.3687786644892981 ) ) ;
#23739 = CARTESIAN_POINT ( 'NONE',  ( 758.0580252608178853, -246.4527844766016074, 328.0187753319985404 ) ) ;
#23740 = ORIENTED_EDGE ( 'NONE', *, *, #5490, .T. ) ;
#23741 = LINE ( 'NONE', #37852, #26274 ) ;
#23742 = DIRECTION ( 'NONE',  ( 0.000000000000000000, 0.000000000000000000, -1.000000000000000000 ) ) ;
#23743 = CARTESIAN_POINT ( 'NONE',  ( -28.63011601220122415, -512.9681489794448908, -327.9999999999999432 ) ) ;
#23744 = CARTESIAN_POINT ( 'NONE',  ( 766.0291762391763086, -226.9181544815163534, 360.7704444035551319 ) ) ;
#23745 = CARTESIAN_POINT ( 'NONE',  ( 755.0636971347428243, -76.27096629478394618, 341.7834795799807353 ) ) ;
#23746 = VERTEX_POINT ( 'NONE', #3832 ) ;
#23747 = CARTESIAN_POINT ( 'NONE',  ( 815.3608509340175488, -434.7363362996975980, -341.2497674668889545 ) ) ;
#23748 = CARTESIAN_POINT ( 'NONE',  ( 758.8095938919644823, -80.08914811296574499, -311.6929314249762797 ) ) ;
#23749 = CARTESIAN_POINT ( 'NONE',  ( 775.9200461376533440, -263.8055962898686175, 315.3028492785443291 ) ) ;
#23750 = CARTESIAN_POINT ( 'NONE',  ( 762.3223304703356007, -415.5436935675102177, -322.3223304703362828 ) ) ;
#23751 = CARTESIAN_POINT ( 'NONE',  ( 774.6312213355098493, -47.36187538569312494, -364.6798772138717482 ) ) ;
#23752 = CARTESIAN_POINT ( 'NONE',  ( 811.3240766477731540, -4.372699936062523385, 355.6651683502462902 ) ) ;
#23753 = CARTESIAN_POINT ( 'NONE',  ( 803.4237431249931660, 8.819942796124882634, -331.2633955100225194 ) ) ;
#23754 = CARTESIAN_POINT ( 'NONE',  ( 769.9779781133707957, -283.0999726633344267, -316.7813123517150871 ) ) ;
#23755 = CARTESIAN_POINT ( 'NONE',  ( 787.4397851343537695, -213.7255117493289731, -374.2001403089903988 ) ) ;
#23756 = CARTESIAN_POINT ( 'NONE',  ( 751.9810565676468741, -74.08914811296577341, 360.9747183278973921 ) ) ;
#23757 = EDGE_CURVE ( 'NONE', #4574, #21203, #32145, .T. ) ;
#23758 = CARTESIAN_POINT ( 'NONE',  ( 810.7187646348534145, -138.4527844766019200, 356.7737145352016341 ) ) ;
#23759 = CARTESIAN_POINT ( 'NONE',  ( 879.9999999999992042, 249.9999999999998295, 199.9999999999997442 ) ) ;
#23760 = CARTESIAN_POINT ( 'NONE',  ( 779.9911637788978851, -452.9681489794448339, 340.0036600600989232 ) ) ;
#23761 = CARTESIAN_POINT ( 'NONE',  ( 773.7943932421234194, -263.8055962898686175, -305.5313806188329409 ) ) ;
#23762 = CARTESIAN_POINT ( 'NONE',  ( 814.4686193811664907, -411.2817908451521589, 346.2056067578752732 ) ) ;
#23763 = CARTESIAN_POINT ( 'NONE',  ( 767.6429770376289525, -273.1800572038742985, -306.8695393053162093 ) ) ;
#23764 = CARTESIAN_POINT ( 'NONE',  ( 799.9999999999993179, 197.3292319334027241, -273.4704985657796783 ) ) ;
#23765 = CARTESIAN_POINT ( 'NONE',  ( 787.5162901302840055, -395.3618753856918602, 305.4481719005792684 ) ) ;
#23766 = CARTESIAN_POINT ( 'NONE',  ( 767.7687537140311633, 0.09267006885218045942, 372.7932403749916830 ) ) ;
#23767 = CARTESIAN_POINT ( 'NONE',  ( 802.1676090361156639, -350.6346026584192828, -327.8955696845344505 ) ) ;
#23768 = CARTESIAN_POINT ( 'NONE',  ( 776.9566956441375396, -12.89650538077851216, 364.8461984189686405 ) ) ;
#23769 = CARTESIAN_POINT ( 'NONE',  ( 761.9338519418445230, -38.53286901714206891, -370.4231160770881957 ) ) ;
#23770 = CARTESIAN_POINT ( 'NONE',  ( 800.7704444035546203, -148.1692326535053610, -326.0291762391768771 ) ) ;
#23771 = CARTESIAN_POINT ( 'NONE',  ( 771.2368401574024119, -181.4419599262325278, 374.2805881961240857 ) ) ;
#23772 = CARTESIAN_POINT ( 'NONE',  ( 785.3141322388236176, 2.274488250670355871, 364.4286716492789537 ) ) ;
#23773 = ORIENTED_EDGE ( 'NONE', *, *, #42141, .F. ) ;
#23774 = CARTESIAN_POINT ( 'NONE',  ( 771.2633955100217236, -71.90732993114760063, -363.4237431249939618 ) ) ;
#23775 = CARTESIAN_POINT ( 'NONE',  ( 787.6308680596127942, -155.2601417444144261, -364.1105419155492768 ) ) ;
#23776 = PRODUCT_DEFINITION_CONTEXT ( 'detailed design', #14295, 'design' ) ;
#23777 = CARTESIAN_POINT ( 'NONE',  ( 795.1360043628807261, -164.0891481129655176, 360.2193346964456282 ) ) ;
#23778 = EDGE_CURVE ( 'NONE', #38196, #9202, #31415, .T. ) ;
#23779 = CARTESIAN_POINT ( 'NONE',  ( 758.0141637701419768, 8.921676437403235127, -367.2620300519063790 ) ) ;
#23781 = CARTESIAN_POINT ( 'NONE',  ( 781.8018195045267476, -310.2709662947832499, 365.1927285166407273 ) ) ;
#23780 = CARTESIAN_POINT ( 'NONE',  ( 801.9419747391806368, -282.4527844766014937, 351.9812246680014027 ) ) ;
#23782 = CARTESIAN_POINT ( 'NONE',  ( 999.9999999999992042, -599.0000000000001137, -360.0000000000000000 ) ) ;
#23783 = VERTEX_POINT ( 'NONE', #28544 ) ;
#23784 = CARTESIAN_POINT ( 'NONE',  ( 758.6633372737375112, -20.53286901714212931, 326.9102291470432533 ) ) ;
#23785 = CARTESIAN_POINT ( 'NONE',  ( 764.1737431748507561, -322.3726999360615082, -371.6461892240376415 ) ) ;
#23786 = ITEM_DEFINED_TRANSFORMATION ( 'NONE', 'NONE', #15708,  #26858 ) ;
#23787 = ADVANCED_FACE ( 'NONE', ( #11220 ), #42638, .F. ) ;
#23788 = CARTESIAN_POINT ( 'NONE',  ( 787.4397851343537695, -213.7255117493289731, 374.2001403089903988 ) ) ;
#23789 = CARTESIAN_POINT ( 'NONE',  ( 763.8424801807145741, -330.0090635724251342, 320.5453621957614700 ) ) ;
#23790 = CARTESIAN_POINT ( 'NONE',  ( 755.0488828828309806, -425.8055962898680491, 344.1219089521771934 ) ) ;
#23791 = CARTESIAN_POINT ( 'NONE',  ( 769.0155153010367712, -106.3726999360621903, -362.7791456095907279 ) ) ;
#23792 = CARTESIAN_POINT ( 'NONE',  ( 781.8018195045266339, -118.2709662947837899, -365.1927285166406705 ) ) ;
#23793 = AXIS2_PLACEMENT_3D ( 'NONE', #32253, #24855, #25080 ) ;
#23794 = CARTESIAN_POINT ( 'NONE',  ( 791.9812246680005501, -308.6346026584195670, -361.9419747391813189 ) ) ;
#23795 = EDGE_LOOP ( 'NONE', ( #2867, #14157, #4686, #7241 ) ) ;
#23796 = CARTESIAN_POINT ( 'NONE',  ( 800.0135310231082713, -446.0891481129646081, -325.0180583372163028 ) ) ;
#23797 = CARTESIAN_POINT ( 'NONE',  ( 754.9735926884551418, -306.3510508353230648, 340.5236548041000333 ) ) ;
#23798 = LINE ( 'NONE', #2810, #11576 ) ;
#23799 = CARTESIAN_POINT ( 'NONE',  ( 791.8656671112827325, -456.3250812000245560, -367.5545208264068719 ) ) ;
#23800 = CARTESIAN_POINT ( 'NONE',  ( 773.4516893846965786, -115.6454272087894424, 315.8398074228977066 ) ) ;
#23801 = DIRECTION ( 'NONE',  ( 0.000000000000000000, 0.000000000000000000, 1.000000000000000000 ) ) ;
#23802 = ORIENTED_EDGE ( 'NONE', *, *, #25847, .F. ) ;
#23803 = CARTESIAN_POINT ( 'NONE',  ( 746.4236121716829757, -327.8272453906069472, -328.8385539511384650 ) ) ;
#23804 = EDGE_CURVE ( 'NONE', #21321, #18281, #4842, .T. ) ;
#23805 = CARTESIAN_POINT ( 'NONE',  ( 776.2046728542105711, -236.1908817542436338, 304.8212110874238761 ) ) ;
#23806 = CARTESIAN_POINT ( 'NONE',  ( 803.4237431249931660, -327.1800572038741279, -331.2633955100225194 ) ) ;
#23807 = ADVANCED_FACE ( 'NONE', ( #39403 ), #4061, .T. ) ;
#23808 = CARTESIAN_POINT ( 'NONE',  ( 759.9999999999992042, -462.9681489794448339, -370.0000000000000568 ) ) ;
#23809 = CARTESIAN_POINT ( 'NONE',  ( 790.0220218866281812, -199.0999726633346825, -363.2186876482849129 ) ) ;
#23810 = CARTESIAN_POINT ( 'NONE',  ( 811.0346526505616112, -62.63460265842031305, 323.0537975583477532 ) ) ;
#23811 = DIRECTION ( 'NONE',  ( -0.000000000000000000, 1.000000000000000000, -0.000000000000000000 ) ) ;
#23812 = CARTESIAN_POINT ( 'NONE',  ( 767.6429770376291799, -369.1800572038739006, -306.8695393053162093 ) ) ;
#23813 = FACE_OUTER_BOUND ( 'NONE', #41053, .T. ) ;
#23814 = CARTESIAN_POINT ( 'NONE',  ( 749.5768839229115201, -324.5545181178796952, 358.0661480581553064 ) ) ;
#23815 = DIRECTION ( 'NONE',  ( 0.000000000000000000, 0.000000000000000000, -1.000000000000000000 ) ) ;
#23816 = CARTESIAN_POINT ( 'NONE',  ( 808.3070685750230950, -306.9982390220558273, 361.1904061080339261 ) ) ;
#23817 = CARTESIAN_POINT ( 'NONE',  ( 745.4481719005789273, -3.725511749329622813, -347.5162901302853129 ) ) ;
#23818 = CARTESIAN_POINT ( 'NONE',  ( 774.6312213355099630, -239.3618753856924570, -364.6798772138717482 ) ) ;
#23819 = DIRECTION ( 'NONE',  ( -0.000000000000000000, 1.000000000000000000, 0.000000000000000000 ) ) ;
#23820 = CARTESIAN_POINT ( 'NONE',  ( 804.4286716492782716, -401.3618753856920307, 345.3141322388244703 ) ) ;
#23821 = AXIS2_PLACEMENT_3D ( 'NONE', #44981, #155, #35256 ) ;
#23822 = CARTESIAN_POINT ( 'NONE',  ( 793.9708237608222134, -142.9181544815166376, 319.2295555964448681 ) ) ;
#23823 = CARTESIAN_POINT ( 'NONE',  ( 787.6308680596127942, -35.26014174441480264, -364.1105419155492768 ) ) ;
#23824 = CARTESIAN_POINT ( 'NONE',  ( 759.8311093483677041, -70.16923265350563099, 310.9282345327691814 ) ) ;
#23825 = CARTESIAN_POINT ( 'NONE',  ( 795.1360043628808398, -356.0891481129648355, 360.2193346964456282 ) ) ;
#23826 = CARTESIAN_POINT ( 'NONE',  ( -769.9999999999992042, 205.0000000000000568, -329.9999999999999432 ) ) ;
#23827 = EDGE_CURVE ( 'NONE', #7478, #1429, #25530, .T. ) ;
#23828 = SURFACE_STYLE_FILL_AREA ( #37711 ) ;
#23829 = CARTESIAN_POINT ( 'NONE',  ( 758.0580252608178853, -414.4527844766010389, 328.0187753319985404 ) ) ;
#23830 = ORIENTED_EDGE ( 'NONE', *, *, #32349, .F. ) ;
#23831 = ADVANCED_FACE ( 'NONE', ( #22062 ), #19488, .F. ) ;
#23832 = CARTESIAN_POINT ( 'NONE',  ( 784.0799538623451781, -371.8055962898682765, -364.6971507214555572 ) ) ;
#23834 = CARTESIAN_POINT ( 'NONE',  ( 759.9864689768902508, -194.0891481129654039, 354.9819416627836404 ) ) ;
#23833 = CARTESIAN_POINT ( 'NONE',  ( 800.0135310231082713, -206.0891481129653471, 325.0180583372163028 ) ) ;
#23835 = CARTESIAN_POINT ( 'NONE',  ( 744.8212110874229666, -354.8965053807774552, -336.2046728542121627 ) ) ;
#23836 = DIRECTION ( 'NONE',  ( -1.000000000000000000, 0.000000000000000000, 0.000000000000000000 ) ) ;
#23837 = EDGE_LOOP ( 'NONE', ( #5805, #30341, #26034, #21581 ) ) ;
#23838 = CARTESIAN_POINT ( 'NONE',  ( 804.9363028652555840, -376.2709662947829656, 338.2165204200192079 ) ) ;
#23839 = EDGE_LOOP ( 'NONE', ( #21950, #28233, #26436, #19351, #15798, #31109, #25853 ) ) ;
#23840 =( NAMED_UNIT ( * ) PLANE_ANGLE_UNIT ( ) SI_UNIT ( $, .RADIAN. ) );
#23841 = EDGE_CURVE ( 'NONE', #39212, #40621, #33585, .T. ) ;
#23842 = EDGE_CURVE ( 'NONE', #17589, #20167, #42468, .T. ) ;
#23843 = CARTESIAN_POINT ( 'NONE',  ( 796.9462024416508257, -228.4527844766015789, -308.9653473494370246 ) ) ;
#23844 = CARTESIAN_POINT ( 'NONE',  ( 751.6929314249750860, -126.9982390220565094, 318.8095938919659034 ) ) ;
#23845 = ORIENTED_EDGE ( 'NONE', *, *, #5113, .F. ) ;
#23846 = CARTESIAN_POINT ( 'NONE',  ( 758.0580252608178853, -222.4527844766016642, -328.0187753319985404 ) ) ;
#23847 = ORIENTED_EDGE ( 'NONE', *, *, #29307, .F. ) ;
#23848 = CARTESIAN_POINT ( 'NONE',  ( 778.2165204200184689, -334.8164208402376403, -364.9363028652563230 ) ) ;
#23849 = CARTESIAN_POINT ( 'NONE',  ( 804.8461984189677878, -458.1908817542429802, -336.9566956441385628 ) ) ;
#23850 = CARTESIAN_POINT ( 'NONE',  ( 756.1348686366196716, -185.2601417444143692, 347.5531968255698416 ) ) ;
#23852 = LINE ( 'NONE', #34255, #34366 ) ;
#23851 = CARTESIAN_POINT ( 'NONE',  ( 808.6142084849417415, -454.8672832770561740, 349.9915990122670451 ) ) ;
#23853 = CARTESIAN_POINT ( 'NONE',  ( 786.4999999999993179, -436.2161768796786987, 399.7184814855371542 ) ) ;
#23854 = ORIENTED_EDGE ( 'NONE', *, *, #3799, .T. ) ;
#23855 = CARTESIAN_POINT ( 'NONE',  ( 768.0187753319979720, 15.36539734157940629, -318.0580252608186242 ) ) ;
#23856 = CARTESIAN_POINT ( 'NONE',  ( 799.9999999999993179, -462.9681489794448339, -370.0000000000000568 ) ) ;
#23857 = FACE_OUTER_BOUND ( 'NONE', #21429, .T. ) ;
#23858 = VERTEX_POINT ( 'NONE', #36829 ) ;
#23859 = CARTESIAN_POINT ( 'NONE',  ( 745.1792804349281596, -254.1908817542435770, -343.7566961878542884 ) ) ;
#23860 = AXIS2_PLACEMENT_3D ( 'NONE', #16973, #20870, #95 ) ;
#23861 = CARTESIAN_POINT ( 'NONE',  ( 781.2370466360911223, -92.73633629969860692, 304.9990715423533629 ) ) ;
#23863 = CARTESIAN_POINT ( 'NONE',  ( 794.9819416627830151, -228.9982390220561683, -319.9864689768909898 ) ) ;
#23862 = LINE ( 'NONE', #20859, #23140 ) ;
#23864 = CARTESIAN_POINT ( 'NONE',  ( 779.4709603349208464, -384.3510508353227806, -314.7162404726379918 ) ) ;
#23865 = CARTESIAN_POINT ( 'NONE',  ( 805.6418435158337843, -245.4636090269709143, -363.8556311672236916 ) ) ;
#23866 = PLANE ( 'NONE',  #21553 ) ;
#23867 = DIRECTION ( 'NONE',  ( -0.000000000000000000, 1.000000000000000000, -0.000000000000000000 ) ) ;
#23868 = CARTESIAN_POINT ( 'NONE',  ( 799.2566176426618085, -72.00906357242594424, -324.0069404352559559 ) ) ;
#23869 = CARTESIAN_POINT ( 'NONE',  ( 755.1538015810308480, -422.1908817542430370, 343.0433043558613804 ) ) ;
#23870 = CARTESIAN_POINT ( 'NONE',  ( 811.3240766477731540, -364.3726999360614514, 355.6651683502462902 ) ) ;
#23871 = DIRECTION ( 'NONE',  ( 0.000000000000000000, 0.000000000000000000, 1.000000000000000000 ) ) ;
#23872 = CARTESIAN_POINT ( 'NONE',  ( 744.7301800767020268, -268.8164208402378677, -337.4774526936615189 ) ) ;
#23873 = CARTESIAN_POINT ( 'NONE',  ( 998.9999999999992042, -599.0000000000001137, 360.0000000000000000 ) ) ;
#23874 = CARTESIAN_POINT ( 'NONE',  ( 768.0187753319979720, 15.36539734157940629, 318.0580252608186242 ) ) ;
#23875 = CARTESIAN_POINT ( 'NONE',  ( 805.1927285166397041, -40.81642084023859951, -341.8018195045277707 ) ) ;
#23876 = VECTOR ( 'NONE', #21555, 1000.000000000000000 ) ;
#23877 = CARTESIAN_POINT ( 'NONE',  ( 812.3518521366052028, -217.0999726633345972, 326.5853460496235243 ) ) ;
#23878 = CARTESIAN_POINT ( 'NONE',  ( 783.7566961878529810, -168.8965053807780237, -305.1792804349288417 ) ) ;
#23879 = CARTESIAN_POINT ( 'NONE',  ( 763.2262854647970016, -200.6346026584199365, 309.2812353651462445 ) ) ;
#23880 = CARTESIAN_POINT ( 'NONE',  ( 759.0252816721024374, -408.9982390220556567, -368.0189434323527280 ) ) ;
#23881 = CARTESIAN_POINT ( 'NONE',  ( 989.9999999999992042, -419.8175818341089780, -209.9999999999999716 ) ) ;
#23882 = CARTESIAN_POINT ( 'NONE',  ( 762.3223304703356007, -295.5436935675105588, 322.3223304703362828 ) ) ;
#23883 = CARTESIAN_POINT ( 'NONE',  ( 805.2837595273609850, -74.73633629969866377, 340.5290396650784714 ) ) ;
#23884 = CARTESIAN_POINT ( 'NONE',  ( 764.8639956371174549, -440.0891481129644944, -319.7806653035542013 ) ) ;
#23885 = PLANE ( 'NONE',  #24681 ) ;
#23886 = ADVANCED_FACE ( 'NONE', ( #22944 ), #30121, .F. ) ;
#23887 = FACE_OUTER_BOUND ( 'NONE', #31341, .T. ) ;
#23889 = CARTESIAN_POINT ( 'NONE',  ( 757.8323909638827445, -338.6346026584195101, 352.1044303154654358 ) ) ;
#23888 = CARTESIAN_POINT ( 'NONE',  ( 756.7813123517142913, -115.9874144716872877, 329.9779781133712504 ) ) ;
#23890 = ORIENTED_EDGE ( 'NONE', *, *, #24119, .T. ) ;
#23891 = CARTESIAN_POINT ( 'NONE',  ( 800.7704444035546203, -244.1692326535050768, -326.0291762391768771 ) ) ;
#23892 =( GEOMETRIC_REPRESENTATION_CONTEXT ( 3 ) GLOBAL_UNCERTAINTY_ASSIGNED_CONTEXT ( ( #22716 ) ) GLOBAL_UNIT_ASSIGNED_CONTEXT ( ( #35391, #23840, #21088 ) ) REPRESENTATION_CONTEXT ( 'NONE', 'WORKASPACE' ) );
#23893 = CARTESIAN_POINT ( 'NONE',  ( 797.8594530101008786, -133.5436935675110135, -322.1405469898980982 ) ) ;
#23894 = CARTESIAN_POINT ( 'NONE',  ( 762.1405469898971887, -97.54369356751112718, 357.8594530101015607 ) ) ;
#23895 = AXIS2_PLACEMENT_3D ( 'NONE', #7434, #733, #35587 ) ;
#23896 = CARTESIAN_POINT ( 'NONE',  ( 803.8556311672234642, -273.6237781080504305, -365.6418435158340117 ) ) ;
#23897 = DIRECTION ( 'NONE',  ( -1.880165489482579047E-16, -1.000000000000000000, -0.000000000000000000 ) ) ;
#23898 = CARTESIAN_POINT ( 'NONE',  ( 786.2056067578752163, -395.8055962898682765, 374.4686193811670023 ) ) ;
#23899 = VERTEX_POINT ( 'NONE', #43978 ) ;
#23900 = CARTESIAN_POINT ( 'NONE',  ( 756.3353852180819104, -293.9073299311468759, 331.1735550268788302 ) ) ;
#23901 = CARTESIAN_POINT ( 'NONE',  ( 759.2295555964440155, -40.16923265350570915, -353.9708237608231229 ) ) ;
#23902 = CARTESIAN_POINT ( 'NONE',  ( 788.8264449731200330, -165.1800572038745258, -363.6646147819171233 ) ) ;
#23903 = CARTESIAN_POINT ( 'NONE',  ( 797.8594530101008786, -373.5436935675101040, 322.1405469898980982 ) ) ;
#23904 = EDGE_CURVE ( 'NONE', #7856, #33261, #35102, .T. ) ;
#23905 = CARTESIAN_POINT ( 'NONE',  ( 759.0252816721024374, -96.99823902205660886, -368.0189434323527280 ) ) ;
#23906 = CARTESIAN_POINT ( 'NONE',  ( 785.3141322388236176, -93.72551174932934259, -364.4286716492789537 ) ) ;
#23907 = VERTEX_POINT ( 'NONE', #33148 ) ;
#23908 = CARTESIAN_POINT ( 'NONE',  ( 796.9571628226829034, -47.46360902697148987, -321.2382568024804641 ) ) ;
#23909 = CARTESIAN_POINT ( 'NONE',  ( 796.9571628226829034, -359.4636090269705164, -321.2382568024804641 ) ) ;
#23910 = VECTOR ( 'NONE', #27903, 1000.000000000000000 ) ;
#23911 = CARTESIAN_POINT ( 'NONE',  ( 754.7162404726377645, -422.7363362996975980, 339.4709603349214717 ) ) ;
#23914 = CARTESIAN_POINT ( 'NONE',  ( 814.8230680027162407, -341.8055962898683333, 333.7305795820267917 ) ) ;
#23913 = CARTESIAN_POINT ( 'NONE',  ( 989.9999999999992042, -418.3138125091626307, 201.9999999999998010 ) ) ;
#23912 = CARTESIAN_POINT ( 'NONE',  ( 773.4999999999993179, -512.9681489794448908, -350.0000000000000000 ) ) ;
#23915 = VECTOR ( 'NONE', #12596, 1000.000000000000000 ) ;
#23916 = CARTESIAN_POINT ( 'NONE',  ( 763.0428371773158460, -371.4636090269705164, -358.7617431975195359 ) ) ;
#23917 = CARTESIAN_POINT ( 'NONE',  ( 785.3687786644884454, -371.3618753856919739, -315.3201227861279676 ) ) ;
#23918 = CARTESIAN_POINT ( 'NONE',  ( 814.8207195650702488, -122.1908817542439749, -336.2433038121456548 ) ) ;
#23919 = CARTESIAN_POINT ( 'NONE',  ( 749.5768839229115201, -12.55451811788067751, 358.0661480581553064 ) ) ;
#23921 = CARTESIAN_POINT ( 'NONE',  ( 51.16348990802859475, 260.0000000000000568, -208.0249999999945203 ) ) ;
#23920 = DIRECTION ( 'NONE',  ( -0.000000000000000000, 1.000000000000000000, -0.000000000000000000 ) ) ;
#23922 = CARTESIAN_POINT ( 'NONE',  ( 772.3691319403857278, -263.2601417444141134, -315.8894580844506663 ) ) ;
#23923 = CARTESIAN_POINT ( 'NONE',  ( 814.2805881961230625, -169.6454272087892718, -331.2368401574024119 ) ) ;
#23924 = FACE_OUTER_BOUND ( 'NONE', #415, .T. ) ;
#23925 = DIRECTION ( 'NONE',  ( 0.000000000000000000, 0.000000000000000000, 1.000000000000000000 ) ) ;
#23926 = CARTESIAN_POINT ( 'NONE',  ( 783.0745993439762742, -320.1908817542434349, 365.1016975059196739 ) ) ;
#23927 = ORIENTED_EDGE ( 'NONE', *, *, #28021, .F. ) ;
#23928 = CARTESIAN_POINT ( 'NONE',  ( 813.5763878283155464, -291.8272453906071746, 351.1614460488615350 ) ) ;
#23929 = CIRCLE ( 'NONE', #12902, 6.118999999999985562 ) ;
#23930 = CARTESIAN_POINT ( 'NONE',  ( 814.9108240113580450, -184.2709662947835909, -337.5031285880265273 ) ) ;
#23931 = CARTESIAN_POINT ( 'NONE',  ( 879.9999999999992042, 239.9999999999998863, -224.9999999999999716 ) ) ;
#23932 = AXIS2_PLACEMENT_3D ( 'NONE', #33993, #33779, #43940 ) ;
#23933 = CARTESIAN_POINT ( 'NONE',  ( 755.8990559732751535, -107.4636090269713122, 365.9055244015606831 ) ) ;
#23934 = CARTESIAN_POINT ( 'NONE',  ( 746.8695393053150156, -317.9073299311468190, -327.6429770376306010 ) ) ;
#23935 = DIRECTION ( 'NONE',  ( -1.000000000000000000, -0.000000000000000000, -0.000000000000000000 ) ) ;
#23936 = DIRECTION ( 'NONE',  ( 1.000000000000000000, 0.000000000000000000, 0.000000000000000000 ) ) ;
#23937 = CARTESIAN_POINT ( 'NONE',  ( 803.4237431249931660, -183.1800572038744974, 331.2633955100225194 ) ) ;
#23938 = ORIENTED_EDGE ( 'NONE', *, *, #34245, .T. ) ;
#23939 = CARTESIAN_POINT ( 'NONE',  ( 797.8822607201568644, -438.5545181178793541, 370.1134526219340160 ) ) ;
#23940 = CARTESIAN_POINT ( 'NONE',  ( 812.6845335610512393, -367.9874144716865203, -353.5525998758768651 ) ) ;
#23941 = CARTESIAN_POINT ( 'NONE',  ( 782.5225473063381969, -118.2709662947837899, -375.2698199232970637 ) ) ;
#23942 = AXIS2_PLACEMENT_3D ( 'NONE', #1072, #11030, #15181 ) ;
#23943 = CARTESIAN_POINT ( 'NONE',  ( 758.4439275373578084, -60.55451811788051941, 353.2243759319684386 ) ) ;
#23944 = CARTESIAN_POINT ( 'NONE',  ( 808.0189434323515343, -398.0891481129647218, -319.0252816721025511 ) ) ;
#23945 = CARTESIAN_POINT ( 'NONE',  ( 51.16348990802859475, 256.5000000000000568, -206.1189999999945428 ) ) ;
#23946 = CARTESIAN_POINT ( 'NONE',  ( 772.3691319403857278, -431.2601417444136018, 315.8894580844506663 ) ) ;
#23947 = EDGE_LOOP ( 'NONE', ( #14518, #37960, #42200, #7690 ) ) ;
#23948 = VECTOR ( 'NONE', #11412, 1000.000000000000000 ) ;
#23949 = VECTOR ( 'NONE', #28194, 1000.000000000000000 ) ;
#23950 = CARTESIAN_POINT ( 'NONE',  ( 756.1443688327750579, -165.6237781080507716, -314.3581564841659315 ) ) ;
#23951 = CARTESIAN_POINT ( 'NONE',  ( 803.8556311672234642, -273.6237781080504305, 365.6418435158340117 ) ) ;
#23952 = CARTESIAN_POINT ( 'NONE',  ( 774.6312213355098493, -119.3618753856928834, 364.6798772138717482 ) ) ;
#23953 = VERTEX_POINT ( 'NONE', #29666 ) ;
#23954 = CARTESIAN_POINT ( 'NONE',  ( 781.7834795799800531, -274.8164208402378108, 315.0636971347436202 ) ) ;
#23955 = AXIS2_PLACEMENT_3D ( 'NONE', #18064, #36072, #39311 ) ;
#23956 = CARTESIAN_POINT ( 'NONE',  ( 796.9462024416508257, -12.45278447660232146, -308.9653473494370246 ) ) ;
#23957 = FACE_OUTER_BOUND ( 'NONE', #33858, .T. ) ;
#23958 = CIRCLE ( 'NONE', #30604, 6.119000000000013095 ) ;
#23959 = ORIENTED_EDGE ( 'NONE', *, *, #19682, .T. ) ;
#23960 = ORIENTED_EDGE ( 'NONE', *, *, #36478, .T. ) ;
#23961 = CARTESIAN_POINT ( 'NONE',  ( 747.6481478633932056, -397.0999726633340288, -353.4146539503763620 ) ) ;
#23962 = VECTOR ( 'NONE', #22642, 1000.000000000000000 ) ;
#23963 = CARTESIAN_POINT ( 'NONE',  ( 768.0187753319979720, -248.6346026584197659, -318.0580252608186242 ) ) ;
#23965 = CARTESIAN_POINT ( 'NONE',  ( 801.9858362298568863, -267.0783235625958696, 312.7379699480935642 ) ) ;
#23964 = CARTESIAN_POINT ( 'NONE',  ( 808.3070685750232087, -354.9982390220557136, 361.1904061080339829 ) ) ;
#23966 = CARTESIAN_POINT ( 'NONE',  ( 805.2837595273609850, -242.7363362996980811, -340.5290396650784714 ) ) ;
#23967 = CARTESIAN_POINT ( 'NONE',  ( 755.5713283507202505, -245.3618753856925139, -334.6858677611754729 ) ) ;
#23968 = CARTESIAN_POINT ( 'NONE',  ( 764.8639956371174549, -416.0891481129646650, -319.7806653035542581 ) ) ;
#23969 = CARTESIAN_POINT ( 'NONE',  ( 762.1405469898971887, -73.54369356751118403, -357.8594530101015607 ) ) ;
#23970 = CARTESIAN_POINT ( 'NONE',  ( 764.8639956371174549, -248.0891481129651481, 319.7806653035542013 ) ) ;
#23971 = CARTESIAN_POINT ( 'NONE',  ( 814.5518280994195948, -351.7255117493284047, 332.4837098697145734 ) ) ;
#23972 = CIRCLE ( 'NONE', #19570, 2.749999999999919176 ) ;
#23973 = DIRECTION ( 'NONE',  ( -0.000000000000000000, -0.000000000000000000, -1.000000000000000000 ) ) ;
#23974 = CARTESIAN_POINT ( 'NONE',  ( 814.2805881961230625, -49.64542720878965554, -331.2368401574024119 ) ) ;
#23975 = CARTESIAN_POINT ( 'NONE',  ( 794.6702036691820012, 16.45630643248850689, 314.5864782580647443 ) ) ;
#23976 = CYLINDRICAL_SURFACE ( 'NONE', #18714, 7.999999999999896083 ) ;
#23977 = VECTOR ( 'NONE', #38180, 1000.000000000000000 ) ;
#23978 = CARTESIAN_POINT ( 'NONE',  ( 804.4086373105744769, -241.6454272087890729, 333.3843516231986541 ) ) ;
#23979 = CARTESIAN_POINT ( 'NONE',  ( 792.1044303154645831, -132.4527844766018916, 317.8323909638837677 ) ) ;
#23980 = ORIENTED_EDGE ( 'NONE', *, *, #41132, .T. ) ;
#23981 = CARTESIAN_POINT ( 'NONE',  ( 805.2837595273609850, -26.73633629969882008, -340.5290396650784714 ) ) ;
#23982 = CARTESIAN_POINT ( 'NONE',  ( 749.2812353651451076, -78.45278447660211896, -323.2262854647983090 ) ) ;
#23983 = CARTESIAN_POINT ( 'NONE',  ( 758.6633372737375112, -284.5328690171412518, 326.9102291470432533 ) ) ;
#23984 = CARTESIAN_POINT ( 'NONE',  ( 778.2165204200184689, -430.8164208402374129, -364.9363028652563230 ) ) ;
#23985 = CARTESIAN_POINT ( 'NONE',  ( 802.1676090361155502, -38.63460265842041963, -327.8955696845344505 ) ) ;
#23986 = CARTESIAN_POINT ( 'NONE',  ( 795.8262568251477660, 1.627300063937458408, 308.3538107759623585 ) ) ;
#23987 = CARTESIAN_POINT ( 'NONE',  ( 796.9462024416508257, -204.4527844766016926, -308.9653473494370246 ) ) ;
#23988 = CARTESIAN_POINT ( 'NONE',  ( 796.7737145352015204, -92.63460265842026331, 370.7187646348536987 ) ) ;
#23989 = CARTESIAN_POINT ( 'NONE',  ( 813.1304606946830518, -161.9073299311472454, 352.3570229623690580 ) ) ;
#23990 = CARTESIAN_POINT ( 'NONE',  ( 1007.605605532488426, 262.9227088301245203, 634.7515695135432452 ) ) ;
#23991 = VECTOR ( 'NONE', #16956, 1000.000000000000000 ) ;
#23992 = CARTESIAN_POINT ( 'NONE',  ( 759.9999999999992042, 205.0000000000000568, 360.0000000000000000 ) ) ;
#23993 = CARTESIAN_POINT ( 'NONE',  ( 808.7758568127978833, -268.1692326535049347, -320.0363995740631822 ) ) ;
#23994 = AXIS2_PLACEMENT_3D ( 'NONE', #35239, #27179, #20909 ) ;
#23995 = CARTESIAN_POINT ( 'NONE',  ( 781.2370466360911223, -428.7363362996975980, 304.9990715423533629 ) ) ;
#23996 = CARTESIAN_POINT ( 'NONE',  ( 792.3570229623688874, -285.1800572038740711, -373.1304606946836202 ) ) ;
#23997 = LINE ( 'NONE', #35089, #38308 ) ;
#23998 = CARTESIAN_POINT ( 'NONE',  ( 796.9462024416508257, -396.4527844766010389, 308.9653473494370246 ) ) ;
#23999 = CARTESIAN_POINT ( 'NONE',  ( 811.0346526505617248, -14.63460265842049779, 323.0537975583478101 ) ) ;
#24001 = AXIS2_PLACEMENT_3D ( 'NONE', #21166, #24382, #38272 ) ;
#24000 = CARTESIAN_POINT ( 'NONE',  ( 801.9419747391806368, -354.4527844766012095, -351.9812246680014027 ) ) ;
#24002 = CARTESIAN_POINT ( 'NONE',  ( 794.1144889064781864, -34.16923265350572336, 360.9840315886528401 ) ) ;
#24003 = CARTESIAN_POINT ( 'NONE',  ( 788.8264449731200330, -189.1800572038744122, -363.6646147819171233 ) ) ;
#24004 = CARTESIAN_POINT ( 'NONE',  ( 808.7758568127978833, -52.16923265350567362, -320.0363995740631822 ) ) ;
#24005 = CARTESIAN_POINT ( 'NONE',  ( 754.9735926884551418, -138.3510508353236048, -340.5236548041000333 ) ) ;
#24006 = CARTESIAN_POINT ( 'NONE',  ( 756.1443688327750579, -165.6237781080507716, 314.3581564841659315 ) ) ;
#24007 = CARTESIAN_POINT ( 'NONE',  ( 774.6312213355098493, 0.6381246143067237364, 364.6798772138717482 ) ) ;
#24008 = ORIENTED_EDGE ( 'NONE', *, *, #10551, .T. ) ;
#24009 = CARTESIAN_POINT ( 'NONE',  ( 774.6858677611749044, -57.72551174932945628, -315.5713283507209894 ) ) ;
#24010 = CARTESIAN_POINT ( 'NONE',  ( 755.8398074228967971, -163.4419599262325846, -333.4516893846970333 ) ) ;
#24011 = CARTESIAN_POINT ( 'NONE',  ( 764.8639956371174549, -176.0891481129653755, 319.7806653035542013 ) ) ;
#24012 = AXIS2_PLACEMENT_3D ( 'NONE', #32238, #11446, #7754 ) ;
#24013 = PRODUCT_DEFINITION_SHAPE ( 'NONE', 'NONE',  #45730 ) ;
#24014 = CARTESIAN_POINT ( 'NONE',  ( 746.7653713866222915, 6.739858255585061464, -351.0478386215610271 ) ) ;
#24016 = CARTESIAN_POINT ( 'NONE',  ( 797.6776695296629214, -283.5436935675105019, 357.6776695296636603 ) ) ;
#24015 = CARTESIAN_POINT ( 'NONE',  ( 768.0187753319979720, -296.6346026584195670, 318.0580252608186242 ) ) ;
#24017 = CIRCLE ( 'NONE', #41754, 9.999999999999980460 ) ;
#24018 = DIRECTION ( 'NONE',  ( -0.000000000000000000, 1.000000000000000000, 0.000000000000000000 ) ) ;
#24019 = ORIENTED_EDGE ( 'NONE', *, *, #14281, .F. ) ;
#24020 = CARTESIAN_POINT ( 'NONE',  ( 773.3843516231979720, -13.44195992623305713, 364.4086373105754433 ) ) ;
#24021 = CARTESIAN_POINT ( 'NONE',  ( 776.2046728542105711, -308.1908817542434349, -304.8212110874238761 ) ) ;
#24022 = CARTESIAN_POINT ( 'NONE',  ( 748.9653473494365699, -266.6346026584197375, 356.9462024416520762 ) ) ;
#24023 = CARTESIAN_POINT ( 'NONE',  ( 761.4292242960306112, -329.4636090269706870, 323.2154366446414429 ) ) ;
#24024 = CARTESIAN_POINT ( 'NONE',  ( 773.7943932421234194, 24.19440371013046231, 305.5313806188329409 ) ) ;
#24025 = CARTESIAN_POINT ( 'NONE',  ( 796.9571628226829034, -167.4636090269711133, -321.2382568024804641 ) ) ;
#24026 = CARTESIAN_POINT ( 'NONE',  ( 762.1405469898971887, -121.5436935675110419, -357.8594530101015607 ) ) ;
#24027 = CARTESIAN_POINT ( 'NONE',  ( 767.8955696845334842, -312.4527844766013800, -362.1676090361161755 ) ) ;
#24028 = ORIENTED_EDGE ( 'NONE', *, *, #32371, .F. ) ;
#24029 = CARTESIAN_POINT ( 'NONE',  ( 764.0069404352550464, -351.0783235625955854, 359.2566176426627180 ) ) ;
#24030 = AXIS2_PLACEMENT_3D ( 'NONE', #33319, #12530, #1895 ) ;
#24031 = FACE_OUTER_BOUND ( 'NONE', #30915, .T. ) ;
#24032 = CARTESIAN_POINT ( 'NONE',  ( 759.0159684113467620, -136.9181544815166376, 325.8855110935213020 ) ) ;
#24033 = CARTESIAN_POINT ( 'NONE',  ( 759.7806653035534055, -30.99823902205680071, 324.8639956371180801 ) ) ;
#24034 = ORIENTED_EDGE ( 'NONE', *, *, #6043, .T. ) ;
#24035 = CARTESIAN_POINT ( 'NONE',  ( 814.4686193811664907, -363.2817908451523294, -346.2056067578752732 ) ) ;
#24036 = DIRECTION ( 'NONE',  ( 0.000000000000000000, -0.7651688349527138167, -0.6438296778008192334 ) ) ;
#24037 = CARTESIAN_POINT ( 'NONE',  ( 757.7880784355613741, -234.0090635724255037, 312.4576283171834916 ) ) ;
#24038 = CARTESIAN_POINT ( 'NONE',  ( 789.9200121543843807, -193.9874144716870319, 317.0176451133914384 ) ) ;
#24039 = AXIS2_PLACEMENT_3D ( 'NONE', #29755, #26055, #10442 ) ;
#24040 = CARTESIAN_POINT ( 'NONE',  ( 788.7366044899766848, -323.9073299311468190, -316.5762568750059813 ) ) ;
#24041 = SURFACE_STYLE_USAGE ( .BOTH. , #27751 ) ;
#24042 = CARTESIAN_POINT ( 'NONE',  ( 798.5707757039680246, -197.4636090269709996, -356.7845633553585003 ) ) ;
#24043 = AXIS2_PLACEMENT_3D ( 'NONE', #31875, #6322, #27119 ) ;
#24044 = EDGE_CURVE ( 'NONE', #17589, #10014, #5180, .T. ) ;
#24045 = CARTESIAN_POINT ( 'NONE',  ( 794.5458710602071051, -452.9681489794447771, 360.4198067286714604 ) ) ;
#24046 = CARTESIAN_POINT ( 'NONE',  ( 754.9967657858570647, -433.5436935675100472, -365.0032342141425943 ) ) ;
#24047 = DIRECTION ( 'NONE',  ( 0.000000000000000000, 0.000000000000000000, 1.000000000000000000 ) ) ;
#24048 = CARTESIAN_POINT ( 'NONE',  ( 745.7194118038753459, -325.6454272087888739, 348.7631598425976449 ) ) ;
#24049 = CARTESIAN_POINT ( 'NONE',  ( 779.9999999999992042, -462.9681489794448339, 339.9999999999999432 ) ) ;
#24050 = CARTESIAN_POINT ( 'NONE',  ( 796.7737145352015204, -308.6346026584195670, 370.7187646348536987 ) ) ;
#24051 = CARTESIAN_POINT ( 'NONE',  ( 759.0252816721024374, -24.99823902205683268, -368.0189434323527280 ) ) ;
#24052 = ADVANCED_FACE ( 'NONE', ( #15584 ), #8433, .F. ) ;
#24053 = CARTESIAN_POINT ( 'NONE',  ( 759.7806653035534055, -246.9982390220560546, -324.8639956371180801 ) ) ;
#24054 = PLANE ( 'NONE',  #21768 ) ;
#24055 = CARTESIAN_POINT ( 'NONE',  ( 767.8955696845333705, -408.4527844766009252, 362.1676090361162323 ) ) ;
#24056 = CARTESIAN_POINT ( 'NONE',  ( 780.5236548040995785, -140.7363362996984506, 314.9735926884559944 ) ) ;
#24057 = CARTESIAN_POINT ( 'NONE',  ( 766.4474001241216001, -19.09997266333520116, -307.3154664389482491 ) ) ;
#24058 = CARTESIAN_POINT ( 'NONE',  ( 799.4546378042377910, -57.07832356259658013, -356.1575198192848006 ) ) ;
#24059 = CARTESIAN_POINT ( 'NONE',  ( 813.9316612368132837, -55.44195992623293989, 348.6739635108323228 ) ) ;
#24060 = CARTESIAN_POINT ( 'NONE',  ( 795.1360043628808398, -380.0891481129647218, 360.2193346964456282 ) ) ;
#24061 = AXIS2_PLACEMENT_3D ( 'NONE', #43697, #22681, #2118 ) ;
#24062 = DIRECTION ( 'NONE',  ( 0.000000000000000000, 0.000000000000000000, -1.000000000000000000 ) ) ;
#24063 =( LENGTH_UNIT ( ) NAMED_UNIT ( * ) SI_UNIT ( .MILLI., .METRE. ) );
#24064 = CARTESIAN_POINT ( 'NONE',  ( 792.1044303154645831, -420.4527844766009252, 317.8323909638837677 ) ) ;
#24065 = ORIENTED_EDGE ( 'NONE', *, *, #25793, .F. ) ;
#24066 = CARTESIAN_POINT ( 'NONE',  ( 758.0580252608178853, -78.45278447660211896, -328.0187753319985404 ) ) ;
#24067 = VECTOR ( 'NONE', #35408, 1000.000000000000000 ) ;
#24068 = CARTESIAN_POINT ( 'NONE',  ( 780.5290396650775619, -348.3510508353228943, -365.2837595273619513 ) ) ;
#24070 = CARTESIAN_POINT ( 'NONE',  ( 795.1360043628808398, -188.0891481129653755, 360.2193346964456282 ) ) ;
#24069 = CARTESIAN_POINT ( 'NONE',  ( 781.8018195045266339, -190.2709662947835909, 365.1927285166406705 ) ) ;
#24071 = VERTEX_POINT ( 'NONE', #16038 ) ;
#24072 = CARTESIAN_POINT ( 'NONE',  ( 812.6845335610512393, -367.9874144716865203, -353.5525998758768651 ) ) ;
#24073 = PLANE ( 'NONE',  #33017 ) ;
#24074 = EDGE_LOOP ( 'NONE', ( #20943, #28596, #24777, #40608 ) ) ;
#24075 = CARTESIAN_POINT ( 'NONE',  ( 792.1044303154645831, -396.4527844766010389, 317.8323909638837677 ) ) ;
#24076 = ADVANCED_FACE ( 'NONE', ( #22502 ), #40317, .F. ) ;
#24077 = ORIENTED_EDGE ( 'NONE', *, *, #45318, .F. ) ;
#24078 = VERTEX_POINT ( 'NONE', #5393 ) ;
#24079 = VECTOR ( 'NONE', #32059, 1000.000000000000000 ) ;
#24080 = CARTESIAN_POINT ( 'NONE',  ( 811.0346526505616112, -206.6346026584198512, -323.0537975583477532 ) ) ;
#24081 = CARTESIAN_POINT ( 'NONE',  ( 814.5518280994195948, -135.7255117493291721, 332.4837098697145166 ) ) ;
#24082 = ORIENTED_EDGE ( 'NONE', *, *, #35964, .T. ) ;
#24083 = CARTESIAN_POINT ( 'NONE',  ( 804.4286716492782716, -209.3618753856926276, -345.3141322388244703 ) ) ;
#24084 = ORIENTED_EDGE ( 'NONE', *, *, #21315, .F. ) ;
#24085 = CARTESIAN_POINT ( 'NONE',  ( 794.9819416627830151, -324.9982390220559409, -319.9864689768909898 ) ) ;
#24086 = CARTESIAN_POINT ( 'NONE',  ( 755.0636971347428243, -4.270966294784170003, -341.7834795799807353 ) ) ;
#24087 = CARTESIAN_POINT ( 'NONE',  ( 757.2208543904082489, -208.7146871989596946, 350.9844846989624330 ) ) ;
#24088 = FACE_OUTER_BOUND ( 'NONE', #10927, .T. ) ;
#24089 = CARTESIAN_POINT ( 'NONE',  ( -190.7583438952258916, 294.6698570112193920, -274.9999999999999432 ) ) ;
#24090 = ORIENTED_EDGE ( 'NONE', *, *, #919, .T. ) ;
#24091 = CARTESIAN_POINT ( 'NONE',  ( 801.9419747391806368, 5.547215523397618142, -351.9812246680014027 ) ) ;
#24092 = DIRECTION ( 'NONE',  ( 0.000000000000000000, 0.000000000000000000, 1.000000000000000000 ) ) ;
#24093 = PLANE ( 'NONE',  #36628 ) ;
#24094 = ORIENTED_EDGE ( 'NONE', *, *, #38114, .T. ) ;
#24095 = CARTESIAN_POINT ( 'NONE',  ( 771.3260364891663130, -235.6454272087890729, -306.0683387631859773 ) ) ;
#24096 = CARTESIAN_POINT ( 'NONE',  ( 797.8822607201568644, -126.5545181178803205, 370.1134526219340160 ) ) ;
#24097 = CIRCLE ( 'NONE', #16006, 6.119000000000013095 ) ;
#24099 = CARTESIAN_POINT ( 'NONE',  ( 802.1676090361156639, -230.6346026584197659, -327.8955696845344505 ) ) ;
#24098 = CARTESIAN_POINT ( 'NONE',  ( -769.9999999999992042, 205.0000000000000568, -339.9999999999999432 ) ) ;
#24100 = EDGE_CURVE ( 'NONE', #33818, #4120, #32395, .T. ) ;
#24101 = CARTESIAN_POINT ( 'NONE',  ( 794.1144889064781864, -394.1692326535045368, -360.9840315886528401 ) ) ;
#24102 = CARTESIAN_POINT ( 'NONE',  ( 773.4999999999993179, -563.3203001761230553, -342.3463313526983143 ) ) ;
#24103 = DIRECTION ( 'NONE',  ( 0.000000000000000000, 0.000000000000000000, 1.000000000000000000 ) ) ;
#24104 = CARTESIAN_POINT ( 'NONE',  ( 790.9844846989617508, -94.37269993606224716, -317.2208543904092721 ) ) ;
#24105 = VECTOR ( 'NONE', #879, 1000.000000000000000 ) ;
#24106 = ADVANCED_FACE ( 'NONE', ( #1275, #26643 ), #40739, .F. ) ;
#24107 = CARTESIAN_POINT ( 'NONE',  ( 773.7305795820266212, -369.2817908451523294, 374.8230680027170365 ) ) ;
#24108 = CARTESIAN_POINT ( 'NONE',  ( 999.9999999999992042, 479.5857864376268935, 359.5857864376268935 ) ) ;
#24109 = CARTESIAN_POINT ( 'NONE',  ( 815.0009284576459549, 17.64894916467593688, -338.7629533639073429 ) ) ;
#24110 = CARTESIAN_POINT ( 'NONE',  ( 787.5162901302840055, -275.3618753856924286, -305.4481719005793252 ) ) ;
#24111 = PLANE ( 'NONE',  #20217 ) ;
#24112 = CARTESIAN_POINT ( 'NONE',  ( 999.9999999999992042, -590.0000000000001137, 360.0000000000000000 ) ) ;
#24113 = CARTESIAN_POINT ( 'NONE',  ( 802.1676090361156639, -86.63460265842023489, -327.8955696845344505 ) ) ;
#24114 = VECTOR ( 'NONE', #27966, 1000.000000000000000 ) ;
#24115 = CARTESIAN_POINT ( 'NONE',  ( 745.1792804349281596, -206.1908817542437191, 343.7566961878542884 ) ) ;
#24116 = CARTESIAN_POINT ( 'NONE',  ( 793.4146539503750546, -169.9874144716871172, -307.6481478633938877 ) ) ;
#24117 = CARTESIAN_POINT ( 'NONE',  ( 805.0032342141412300, -205.5436935675108430, 314.9967657858571783 ) ) ;
#24118 = CARTESIAN_POINT ( 'NONE',  ( 814.2001403089898304, -401.3618753856920307, -347.4397851343538264 ) ) ;
#24119 = EDGE_CURVE ( 'NONE', #11372, #38196, #29453, .T. ) ;
#24120 = VECTOR ( 'NONE', #1945, 1000.000000000000000 ) ;
#24121 = ADVANCED_FACE ( 'NONE', ( #26430 ), #29892, .F. ) ;
#24122 = DIRECTION ( 'NONE',  ( -0.000000000000000000, 1.000000000000000000, -0.000000000000000000 ) ) ;
#24123 = CARTESIAN_POINT ( 'NONE',  ( 792.1044303154645831, -276.4527844766013800, 317.8323909638837677 ) ) ;
#24124 = CARTESIAN_POINT ( 'NONE',  ( 804.4086373105744769, -49.64542720878965554, 333.3843516231986541 ) ) ;
#24125 = CARTESIAN_POINT ( 'NONE',  ( 800.0135310231082713, -422.0891481129647218, -325.0180583372163028 ) ) ;
#24126 = CARTESIAN_POINT ( 'NONE',  ( -521.6730038022808458, 200.0000000000001421, 350.0000000000000000 ) ) ;
#24127 = CARTESIAN_POINT ( 'NONE',  ( -37.63011601220122770, -359.5698779088871788, -26.28906389436296109 ) ) ;
#24129 = CARTESIAN_POINT ( 'NONE',  ( 803.4237431249931660, -327.1800572038741279, 331.2633955100225194 ) ) ;
#24128 = CARTESIAN_POINT ( 'NONE',  ( 773.3843516231979720, -133.4419599262326699, 364.4086373105754433 ) ) ;
#24130 = ORIENTED_EDGE ( 'NONE', *, *, #44450, .F. ) ;
#24131 = CARTESIAN_POINT ( 'NONE',  ( 793.2243759319678702, -242.5328690171414507, -318.4439275373583200 ) ) ;
#24132 = CARTESIAN_POINT ( 'NONE',  ( 756.3353852180819104, -77.90732993114757221, 331.1735550268788302 ) ) ;
#24133 = CARTESIAN_POINT ( 'NONE',  ( 798.0661480581538854, -266.5328690171413655, -309.5768839229118043 ) ) ;
#24134 = DIRECTION ( 'NONE',  ( -0.000000000000000000, 1.000000000000000000, -0.000000000000000000 ) ) ;
#24135 = CARTESIAN_POINT ( 'NONE',  ( 778.7502325331095108, -432.3510508353226669, 304.6391490659818828 ) ) ;
#24136 = EDGE_CURVE ( 'NONE', #36984, #34629, #23165, .T. ) ;
#24137 = ORIENTED_EDGE ( 'NONE', *, *, #39430, .T. ) ;
#24138 = CARTESIAN_POINT ( 'NONE',  ( 765.0180583372156207, -288.9982390220559978, 360.0135310231089534 ) ) ;
#24139 =( BOUNDED_CURVE ( )  B_SPLINE_CURVE ( 2, ( #22570, #429, #43152, #14533, #11747, #14979, #4137 ),
 .UNSPECIFIED., .F., .T. ) 
 B_SPLINE_CURVE_WITH_KNOTS ( ( 3, 2, 2, 3 ),
 ( 0.000000000000000000, 0.002272727272727272617, 0.004545454545454545234, 0.006081874955971018626 ),
 .UNSPECIFIED. ) 
 CURVE ( )  GEOMETRIC_REPRESENTATION_ITEM ( )  RATIONAL_B_SPLINE_CURVE ( ( 0.5000002209606653203, 0.4949109396520706694, 0.5000002209606653203, 0.4949109396520706694, 0.5000002209606653203, 0.4965597396626160176, 0.4977709609702910543 ) ) 
 REPRESENTATION_ITEM ( '' )  );
#24140 = ADVANCED_FACE ( 'NONE', ( #16259 ), #12784, .F. ) ;
#24141 = CARTESIAN_POINT ( 'NONE',  ( 780.5290396650775619, -36.35105083532390324, -365.2837595273619513 ) ) ;
#24142 = CARTESIAN_POINT ( 'NONE',  ( 762.1405469898971887, -193.5436935675108714, -357.8594530101015607 ) ) ;
#24143 = CARTESIAN_POINT ( 'NONE',  ( 771.1735550268778070, -417.1800572038736163, 316.3353852180827630 ) ) ;
#24144 = CARTESIAN_POINT ( 'NONE',  ( 767.7687537140311633, -119.9073299311474443, -372.7932403749916830 ) ) ;
#24145 = CARTESIAN_POINT ( 'NONE',  ( 765.0180583372156207, -120.9982390220565378, -360.0135310231089534 ) ) ;
#24146 = ORIENTED_EDGE ( 'NONE', *, *, #10015, .T. ) ;
#24147 = CARTESIAN_POINT ( 'NONE',  ( 755.1538015810308480, -38.19088175424422360, -343.0433043558613804 ) ) ;
#24148 = AXIS2_PLACEMENT_3D ( 'NONE', #35668, #11203, #39164 ) ;
#24149 = CARTESIAN_POINT ( 'NONE',  ( 784.1219089521767955, -357.2817908451523294, -315.0488828828318333 ) ) ;
#24151 = CARTESIAN_POINT ( 'NONE',  ( 755.8894580844503253, -447.8272453906067199, 332.3691319403863531 ) ) ;
#24150 = CARTESIAN_POINT ( 'NONE',  ( 755.3201227861273992, -123.7255117493292147, 345.3687786644892981 ) ) ;
#24152 = CARTESIAN_POINT ( 'NONE',  ( 805.0264073115434940, -102.3510508353236901, 339.4763451958999099 ) ) ;
#24155 = CARTESIAN_POINT ( 'NONE',  ( 776.2433038121456548, -372.8965053807773415, 374.8207195650711014 ) ) ;
#24154 = CARTESIAN_POINT ( 'NONE',  ( 799.9999999999993179, 205.0000000000000568, 360.0000000000000000 ) ) ;
#24153 = CARTESIAN_POINT ( 'NONE',  ( 799.9999999999993179, 197.3292319334027241, 273.4704985657796783 ) ) ;
#24156 = EDGE_LOOP ( 'NONE', ( #15377, #34878, #36680, #27894 ) ) ;
#24157 = CARTESIAN_POINT ( 'NONE',  ( 783.0745993439762742, -344.1908817542433212, -365.1016975059196739 ) ) ;
#24158 = CARTESIAN_POINT ( 'NONE',  ( 781.7834795799800531, -346.8164208402376971, -315.0636971347436202 ) ) ;
#24159 = CARTESIAN_POINT ( 'NONE',  ( 814.2805881961230625, -121.6454272087894282, -331.2368401574024119 ) ) ;
#24160 = ADVANCED_FACE ( 'NONE', ( #14589 ), #16487, .T. ) ;
#24161 = CARTESIAN_POINT ( 'NONE',  ( 776.2046728542105711, -44.19088175424421649, 304.8212110874238761 ) ) ;
#24162 = EDGE_CURVE ( 'NONE', #34493, #38419, #3786, .T. ) ;
#24164 = CARTESIAN_POINT ( 'NONE',  ( 787.4999999999992042, -462.9681489794447202, -270.0000000000000568 ) ) ;
#24163 = CARTESIAN_POINT ( 'NONE',  ( -78.83651009197140525, 260.0000000000000568, -199.9999999999936051 ) ) ;
#24165 = EDGE_CURVE ( 'NONE', #34816, #7404, #31655, .T. ) ;
#24166 = CARTESIAN_POINT ( 'NONE',  ( 754.8983024940795303, -282.8965053807776258, -336.9254006560228163 ) ) ;
#24167 = CARTESIAN_POINT ( 'NONE',  ( 814.4686193811664907, -147.2817908451529547, -346.2056067578752732 ) ) ;
#24168 = DIRECTION ( 'NONE',  ( -0.000000000000000000, -0.000000000000000000, 1.000000000000000000 ) ) ;
#24169 = FACE_OUTER_BOUND ( 'NONE', #12388, .T. ) ;
#24170 = CARTESIAN_POINT ( 'NONE',  ( 772.4468031744293057, -321.8272453906070609, 363.8651313633793620 ) ) ;
#24171 = EDGE_CURVE ( 'NONE', #33185, #22001, #30809, .T. ) ;
#24172 = CARTESIAN_POINT ( 'NONE',  ( 810.4231160770870019, -288.5545181178798657, 321.9338519418446936 ) ) ;
#24173 = CARTESIAN_POINT ( 'NONE',  ( 813.1304606946831655, -161.9073299311472738, -352.3570229623691716 ) ) ;
#24174 = CARTESIAN_POINT ( 'NONE',  ( 786.4999999999993179, -512.9681489794448908, -339.9999999999999432 ) ) ;
#24175 = CARTESIAN_POINT ( 'NONE',  ( 793.5525998758768083, -103.0999726633349525, 372.6845335610516941 ) ) ;
#24176 = CARTESIAN_POINT ( 'NONE',  ( 751.9810565676468741, -314.0891481129650629, -360.9747183278973921 ) ) ;
#24177 = EDGE_CURVE ( 'NONE', #41429, #37578, #10754, .T. ) ;
#24178 = DIRECTION ( 'NONE',  ( 0.000000000000000000, 0.000000000000000000, -1.000000000000000000 ) ) ;
#24179 = DIRECTION ( 'NONE',  ( 0.000000000000000000, 0.000000000000000000, 1.000000000000000000 ) ) ;
#24180 = CARTESIAN_POINT ( 'NONE',  ( 774.6858677611749044, -201.7255117493290015, 315.5713283507209894 ) ) ;
#24181 = VERTEX_POINT ( 'NONE', #3943 ) ;
#24182 = CARTESIAN_POINT ( 'NONE',  ( 799.9636004259356241, -430.9181544815157849, 311.2241431872006956 ) ) ;
#24183 = CARTESIAN_POINT ( 'NONE',  ( 746.7653713866222915, -377.2601417444137724, -351.0478386215610271 ) ) ;
#24184 = AXIS2_PLACEMENT_3D ( 'NONE', #27105, #31245, #13015 ) ;
#24185 = CARTESIAN_POINT ( 'NONE',  ( 772.4837098697144029, -119.3618753856928691, -374.5518280994205611 ) ) ;
#24186 = CARTESIAN_POINT ( 'NONE',  ( 757.4527132478984868, -64.37269993606231822, 329.1273215169538844 ) ) ;
#24187 = CARTESIAN_POINT ( 'NONE',  ( 804.7487373415286811, -403.5436935675101608, -364.7487373415288516 ) ) ;
#24188 = DIRECTION ( 'NONE',  ( 0.000000000000000000, 0.000000000000000000, 1.000000000000000000 ) ) ;
#24189 = CARTESIAN_POINT ( 'NONE',  ( 813.2346286133761168, 18.73985825558501972, 328.9521613784389160 ) ) ;
#24190 = VERTEX_POINT ( 'NONE', #37735 ) ;
#24191 = CARTESIAN_POINT ( 'NONE',  ( 759.8311093483677041, -142.1692326535054178, -310.9282345327691814 ) ) ;
#24192 = CARTESIAN_POINT ( 'NONE',  ( -728.8365100919714905, 256.5000000000001705, -197.2499999999891429 ) ) ;
#24193 = CARTESIAN_POINT ( 'NONE',  ( 744.8212110874229666, -282.8965053807776258, 336.2046728542121627 ) ) ;
#24194 = CARTESIAN_POINT ( 'NONE',  ( 771.1735550268780344, -105.1800572038747390, 316.3353852180828198 ) ) ;
#24195 = ORIENTED_EDGE ( 'NONE', *, *, #5145, .F. ) ;
#24196 = CARTESIAN_POINT ( 'NONE',  ( 771.2633955100217236, -311.9073299311468759, 363.4237431249939618 ) ) ;
#24197 = CARTESIAN_POINT ( 'NONE',  ( 814.9108240113580450, -16.27096629478413092, -337.5031285880265273 ) ) ;
#24198 = CARTESIAN_POINT ( 'NONE',  ( 791.9445882927475395, -448.7226863535211123, 370.2744874727277420 ) ) ;
#24199 = ORIENTED_EDGE ( 'NONE', *, *, #43343, .T. ) ;
#24200 = CARTESIAN_POINT ( 'NONE',  ( 747.6481478633932056, -421.0999726633340288, -353.4146539503763620 ) ) ;
#24201 = CARTESIAN_POINT ( 'NONE',  ( 804.4286716492782716, -41.36187538569314626, 345.3141322388244703 ) ) ;
#24202 = CARTESIAN_POINT ( 'NONE',  ( 778.2165204200184689, -262.8164208402379245, -364.9363028652563230 ) ) ;
#24204 = CARTESIAN_POINT ( 'NONE',  ( 754.0944755984390895, -255.6237781080504874, 364.1009440267246760 ) ) ;
#24203 = CARTESIAN_POINT ( 'NONE',  ( 812.7932403749906598, -375.1800572038739574, 327.7687537140311633 ) ) ;
#24205 = CARTESIAN_POINT ( 'NONE',  ( 804.4086373105744769, -241.6454272087890729, -333.3843516231986541 ) ) ;
#24206 = CARTESIAN_POINT ( 'NONE',  ( 755.3201227861273992, -267.7255117493286320, -345.3687786644892981 ) ) ;
#24207 = CARTESIAN_POINT ( 'NONE',  ( 774.6858677611749044, -441.7255117493282910, -315.5713283507209894 ) ) ;
#24208 = CARTESIAN_POINT ( 'NONE',  ( 771.2633955100217236, -71.90732993114760063, -363.4237431249939618 ) ) ;
#24209 = CARTESIAN_POINT ( 'NONE',  ( 797.8594530101008786, -253.5436935675104735, 322.1405469898980982 ) ) ;
#24210 = VERTEX_POINT ( 'NONE', #30568 ) ;
#24211 = AXIS2_PLACEMENT_3D ( 'NONE', #16812, #24397, #27642 ) ;
#24212 = CARTESIAN_POINT ( 'NONE',  ( 800.9747183278959710, -348.9982390220558273, 311.9810565676471583 ) ) ;
#24213 = DIRECTION ( 'NONE',  ( -0.000000000000000000, -0.000000000000000000, 1.000000000000000000 ) ) ;
#24214 = PRODUCT_DEFINITION ( 'UNKNOWN', '', #1676, #8864 ) ;
#24215 = CARTESIAN_POINT ( 'NONE',  ( 750.9282345327678740, -40.91815448151695023, -319.8311093483690115 ) ) ;
#24216 = CYLINDRICAL_SURFACE ( 'NONE', #4932, 24.99999999999991118 ) ;
#24217 = CARTESIAN_POINT ( 'NONE',  ( -208.8365100919714052, 260.0000000000001137, -199.9999999999926956 ) ) ;
#24218 = CARTESIAN_POINT ( 'NONE',  ( 761.4292242960306112, -233.4636090269708575, 323.2154366446414429 ) ) ;
#24219 = CARTESIAN_POINT ( 'NONE',  ( 765.0180583372156207, -120.9982390220565378, 360.0135310231089534 ) ) ;
#24220 = ORIENTED_EDGE ( 'NONE', *, *, #22962, .F. ) ;
#24221 = CARTESIAN_POINT ( 'NONE',  ( 783.0745993439762742, -8.190881754244330182, -365.1016975059196739 ) ) ;
#24222 = CARTESIAN_POINT ( 'NONE',  ( 751.6929314249750860, -54.99823902205672965, -318.8095938919659034 ) ) ;
#24223 = CARTESIAN_POINT ( 'NONE',  ( 795.9930595647434757, -291.0783235625957559, 320.7433823573372820 ) ) ;
#24224 = CARTESIAN_POINT ( 'NONE',  ( 804.4286716492782716, -449.3618753856918602, -345.3141322388244703 ) ) ;
#24225 = CARTESIAN_POINT ( 'NONE',  ( 803.4237431249931660, -39.18005720387496638, -331.2633955100225194 ) ) ;
#24226 = CARTESIAN_POINT ( 'NONE',  ( 812.3518521366052028, -1.099972663335260226, 326.5853460496235243 ) ) ;
#24227 = CARTESIAN_POINT ( 'NONE',  ( 800.9747183278959710, -204.9982390220562820, -311.9810565676471583 ) ) ;
#24228 = CARTESIAN_POINT ( 'NONE',  ( 751.6929314249748586, -174.9982390220563673, 318.8095938919659034 ) ) ;
#24229 = CARTESIAN_POINT ( 'NONE',  ( 797.6776695296629214, -91.54369356751116982, 357.6776695296636603 ) ) ;
#24230 = CARTESIAN_POINT ( 'NONE',  ( -208.8365100919714052, 230.0000000000000853, -202.7499999999925251 ) ) ;
#24231 = CARTESIAN_POINT ( 'NONE',  ( 999.9999999999992042, 478.9999999999999432, -359.0000000000000000 ) ) ;
#24232 = CARTESIAN_POINT ( 'NONE',  ( 781.2497674668890113, -276.3510508353231785, -375.3608509340180603 ) ) ;
#24233 = CARTESIAN_POINT ( 'NONE',  ( 746.4236121716829757, -423.8272453906067199, 328.8385539511384650 ) ) ;
#24234 = CARTESIAN_POINT ( 'NONE',  ( 811.0346526505616112, -278.6346026584196807, -323.0537975583477532 ) ) ;
#24235 = DIRECTION ( 'NONE',  ( 0.000000000000000000, 0.000000000000000000, 1.000000000000000000 ) ) ;
#24236 = CARTESIAN_POINT ( 'NONE',  ( 745.0891759886404770, -388.2709662947829656, 342.4968714119734159 ) ) ;
#24237 = CARTESIAN_POINT ( 'NONE',  ( 772.5602148656447525, -9.725511749329603717, 305.7998596910095443 ) ) ;
#24238 = CARTESIAN_POINT ( 'NONE',  ( 788.7366044899766848, -395.9073299311465348, -316.5762568750059813 ) ) ;
#24239 = CARTESIAN_POINT ( 'NONE',  ( 803.2186876482843445, -7.987414471687621642, 350.0220218866286928 ) ) ;
#24240 = CARTESIAN_POINT ( 'NONE',  ( 745.1769319972822814, -65.80559628986925702, -346.2694204179732083 ) ) ;
#24241 = CARTESIAN_POINT ( 'NONE',  ( 803.8651313633788504, -173.2601417444143692, -332.4468031744301015 ) ) ;
#24242 = CARTESIAN_POINT ( 'NONE',  ( 759.8311093483677041, -166.1692326535053041, 310.9282345327691814 ) ) ;
#24243 = CARTESIAN_POINT ( 'NONE',  ( 800.2193346964446619, -18.99823902205684689, 355.1360043628816925 ) ) ;
#24244 = AXIS2_PLACEMENT_3D ( 'NONE', #44868, #34215, #2590 ) ;
#24245 = ORIENTED_EDGE ( 'NONE', *, *, #14278, .F. ) ;
#24246 = CARTESIAN_POINT ( 'NONE',  ( 778.1981804954714335, -58.27096629478398171, -314.8072714833589885 ) ) ;
#24247 = CARTESIAN_POINT ( 'NONE',  ( 784.0799538623451781, -203.8055962898688449, -364.6971507214555572 ) ) ;
#24248 = UNCERTAINTY_MEASURE_WITH_UNIT (LENGTH_MEASURE( 1.000000000000000082E-05 ), #37231, 'distance_accuracy_value', 'NONE');
#24249 = CARTESIAN_POINT ( 'NONE',  ( 797.6776695296629214, -163.5436935675109567, 357.6776695296636603 ) ) ;
#24250 = CARTESIAN_POINT ( 'NONE',  ( 791.1614460488616487, 12.73985825558503926, -373.5763878283158874 ) ) ;
#24251 = CARTESIAN_POINT ( 'NONE',  ( 759.7806653035535192, -318.9982390220558841, 324.8639956371181370 ) ) ;
#24252 = CARTESIAN_POINT ( 'NONE',  ( 794.9999999999993179, 205.0000000000000568, -245.0000000000000284 ) ) ;
#24253 = ORIENTED_EDGE ( 'NONE', *, *, #5775, .T. ) ;
#24254 = CARTESIAN_POINT ( 'NONE',  ( 804.1601925771018387, -31.44195992623299674, 346.5483106153029098 ) ) ;
#24255 = CARTESIAN_POINT ( 'NONE',  ( 764.1737431748507561, -298.3726999360616787, -371.6461892240376415 ) ) ;
#24256 = CARTESIAN_POINT ( 'NONE',  ( 796.7737145352015204, -260.6346026584197375, 370.7187646348536987 ) ) ;
#24257 = CARTESIAN_POINT ( 'NONE',  ( 793.0897708529556667, -318.5545181178796952, 361.3366627262616362 ) ) ;
#24258 = CARTESIAN_POINT ( 'NONE',  ( 760.5453621957607311, -429.0783235625953580, 323.8424801807151425 ) ) ;
#24259 = CARTESIAN_POINT ( 'NONE',  ( 802.9823548866075953, -145.0999726633347677, -330.0799878456151077 ) ) ;
#24260 = CARTESIAN_POINT ( 'NONE',  ( 805.1927285166397041, -136.8164208402382371, -341.8018195045277707 ) ) ;
#24261 = CARTESIAN_POINT ( 'NONE',  ( 759.9864689768902508, -314.0891481129650629, -354.9819416627836404 ) ) ;
#24262 = ORIENTED_EDGE ( 'NONE', *, *, #7816, .T. ) ;
#24263 = CARTESIAN_POINT ( 'NONE',  ( 798.7617431975189675, -339.6237781080502600, 323.0428371773161871 ) ) ;
#24264 = CARTESIAN_POINT ( 'NONE',  ( 784.4999999999993179, -512.9681489794448908, -327.9999999999999432 ) ) ;
#24265 = CARTESIAN_POINT ( 'NONE',  ( 766.9102291470427417, -138.5545181178802636, 318.6633372737382501 ) ) ;
#24266 = CARTESIAN_POINT ( 'NONE',  ( 785.3687786644884454, -11.36187538569323863, 315.3201227861279676 ) ) ;
#24267 = VERTEX_POINT ( 'NONE', #28420 ) ;
#24268 = CARTESIAN_POINT ( 'NONE',  ( 809.0717654672305343, -388.9181544815158986, -360.1688906516309885 ) ) ;
#24269 = EDGE_CURVE ( 'NONE', #5117, #518, #5867, .T. ) ;
#24270 = PLANE ( 'NONE',  #3337 ) ;
#24271 = CARTESIAN_POINT ( 'NONE',  ( 796.1575198192839480, -222.0090635724254184, 359.4546378042384163 ) ) ;
#24272 = CARTESIAN_POINT ( 'NONE',  ( 746.4236121716829757, -231.8272453906072315, 328.8385539511384650 ) ) ;
#24273 = AXIS2_PLACEMENT_3D ( 'NONE', #27937, #10379, #24455 ) ;
#24274 = CARTESIAN_POINT ( 'NONE',  ( 787.6308680596127942, -203.2601417444143124, 364.1105419155492768 ) ) ;
#24275 = CARTESIAN_POINT ( 'NONE',  ( 762.1405469898971887, -313.5436935675102745, -357.8594530101015607 ) ) ;
#24276 = LINE ( 'NONE', #23808, #36256 ) ;
#24277 = CARTESIAN_POINT ( 'NONE',  ( 769.9779781133707957, -235.0999726633344835, -316.7813123517150871 ) ) ;
#24278 = CARTESIAN_POINT ( 'NONE',  ( 772.5602148656447525, -81.72551174932937101, 305.7998596910095443 ) ) ;
#24279 = CARTESIAN_POINT ( 'NONE',  ( 799.5976253717891495, -452.9681489794447771, 356.1016198435977458 ) ) ;
#24280 = CARTESIAN_POINT ( 'NONE',  ( 808.0189434323515343, -422.0891481129647218, -319.0252816721025511 ) ) ;
#24281 = DIRECTION ( 'NONE',  ( -1.880165489482579047E-16, -1.000000000000000000, -0.000000000000000000 ) ) ;
#24282 = CARTESIAN_POINT ( 'NONE',  ( 802.2119215644370342, -366.0090635724250774, 367.5423716828165084 ) ) ;
#24283 = DIRECTION ( 'NONE',  ( 1.000000000000000000, 0.000000000000000000, -0.000000000000000000 ) ) ;
#24284 = CARTESIAN_POINT ( 'NONE',  ( 787.4397851343537695, -45.72551174932949181, -374.2001403089903988 ) ) ;
#24285 = CARTESIAN_POINT ( 'NONE',  ( 759.9864689768902508, -266.0891481129651197, -354.9819416627836404 ) ) ;
#24286 = CARTESIAN_POINT ( 'NONE',  ( -208.8365100919714052, 256.5000000000001137, -199.9999999999926956 ) ) ;
#24287 = ADVANCED_FACE ( 'NONE', ( #21266 ), #17584, .F. ) ;
#24288 = CARTESIAN_POINT ( 'NONE',  ( 805.1927285166397041, -400.8164208402373561, 341.8018195045277707 ) ) ;
#24289 = CARTESIAN_POINT ( 'NONE',  ( 800.9840315886518738, -148.9181544815166092, 354.1144889064786412 ) ) ;
#24290 = CARTESIAN_POINT ( 'NONE',  ( 745.7194118038753459, -13.64542720878976390, -348.7631598425976449 ) ) ;
#24291 = CARTESIAN_POINT ( 'NONE',  ( 800.7704444035546203, -52.16923265350567362, -326.0291762391768771 ) ) ;
#24292 = CARTESIAN_POINT ( 'NONE',  ( 803.8556311672234642, -81.62377810805104161, 365.6418435158340117 ) ) ;
#24293 = CARTESIAN_POINT ( 'NONE',  ( 802.1676090361155502, -422.6346026584191691, 327.8955696845344505 ) ) ;
#24294 = CARTESIAN_POINT ( 'NONE',  ( 787.5162901302840055, 12.63812461430668677, 305.4481719005793252 ) ) ;
#24295 = CARTESIAN_POINT ( 'NONE',  ( -28.63011601220122415, -512.9681489794448908, -339.9999999999999432 ) ) ;
#24296 = CARTESIAN_POINT ( 'NONE',  ( 754.0944755984390895, -135.6237781080508853, 364.1009440267246760 ) ) ;
#24297 = CARTESIAN_POINT ( 'NONE',  ( 797.8594530101008786, -421.5436935675101040, 322.1405469898980982 ) ) ;
#24298 = ORIENTED_EDGE ( 'NONE', *, *, #42804, .F. ) ;
#24299 = CARTESIAN_POINT ( 'NONE',  ( 755.3201227861273992, -75.72551174932937101, -345.3687786644892981 ) ) ;
#24300 = CARTESIAN_POINT ( 'NONE',  ( 790.8726784830453198, -370.7146871989592114, -362.5472867521010585 ) ) ;
#24302 = CARTESIAN_POINT ( 'NONE',  ( 800.0135310231082713, -182.0891481129654323, 325.0180583372163028 ) ) ;
#24301 = CARTESIAN_POINT ( 'NONE',  ( 795.1360043628807261, -212.0891481129652902, 360.2193346964456282 ) ) ;
#24303 = CARTESIAN_POINT ( 'NONE',  ( 754.0944755984390895, -399.6237781080500326, -364.1009440267246760 ) ) ;
#24304 = CARTESIAN_POINT ( 'NONE',  ( -775.4999999999993179, -110.5936016518799221, 750.6326042729449455 ) ) ;
#24305 = EDGE_LOOP ( 'NONE', ( #11205, #9275, #42207, #34889 ) ) ;
#24306 = CARTESIAN_POINT ( 'NONE',  ( 781.8018195045266339, -382.2709662947828519, 365.1927285166406705 ) ) ;
#24307 = VECTOR ( 'NONE', #43145, 1000.000000000000000 ) ;
#24308 = ORIENTED_EDGE ( 'NONE', *, *, #11210, .T. ) ;
#24309 =( LENGTH_UNIT ( ) NAMED_UNIT ( * ) SI_UNIT ( .MILLI., .METRE. ) );
#24310 = CARTESIAN_POINT ( 'NONE',  ( 767.7687537140311633, -215.9073299311471317, -372.7932403749916830 ) ) ;
#24311 = CARTESIAN_POINT ( 'NONE',  ( 787.5162901302840055, -155.3618753856927697, 305.4481719005793252 ) ) ;
#24312 = EDGE_LOOP ( 'NONE', ( #29659, #45110, #34821, #38463 ) ) ;
#24313 = CARTESIAN_POINT ( 'NONE',  ( 803.6646147819162707, -209.9073299311471317, -348.8264449731211130 ) ) ;
#24314 = ADVANCED_FACE ( 'NONE', ( #6087 ), #35566, .T. ) ;
#24315 = ORIENTED_EDGE ( 'NONE', *, *, #18116, .T. ) ;
#24316 = CARTESIAN_POINT ( 'NONE',  ( 804.4286716492782716, -353.3618753856922012, -345.3141322388244703 ) ) ;
#24317 = CARTESIAN_POINT ( 'NONE',  ( 774.6312213355099630, 0.6381246143067236254, -364.6798772138717482 ) ) ;
#24318 = CARTESIAN_POINT ( 'NONE',  ( 804.1601925771018387, -247.4419599262323004, 346.5483106153029098 ) ) ;
#24319 = FACE_OUTER_BOUND ( 'NONE', #19320, .T. ) ;
#24320 = ADVANCED_FACE ( 'NONE', ( #37508 ), #42519, .T. ) ;
#24321 = CARTESIAN_POINT ( 'NONE',  ( -468.8365100919714337, 260.0000000000001705, -199.9999999999908766 ) ) ;
#24322 = VERTEX_POINT ( 'NONE', #14114 ) ;
#24323 = CARTESIAN_POINT ( 'NONE',  ( 767.8955696845333705, -0.4527844766023628176, -362.1676090361162323 ) ) ;
#24324 = DIRECTION ( 'NONE',  ( -1.000000000000000000, -0.000000000000000000, -0.000000000000000000 ) ) ;
#24325 = CARTESIAN_POINT ( 'NONE',  ( -26.63011601220122060, -544.8427095258973623, -350.0000000000000000 ) ) ;
#24326 = CARTESIAN_POINT ( 'NONE',  ( 812.3518521366052028, -265.0999726633344267, -326.5853460496235243 ) ) ;
#24327 = CARTESIAN_POINT ( 'NONE',  ( 748.6759233522253680, -136.3726999360621051, 324.3348316497537098 ) ) ;
#24329 = CARTESIAN_POINT ( 'NONE',  ( 804.9363028652555840, -208.2709662947835341, -338.2165204200192079 ) ) ;
#24328 = DIRECTION ( 'NONE',  ( 1.000000000000000000, -0.000000000000000000, -0.000000000000000000 ) ) ;
#24330 = CARTESIAN_POINT ( 'NONE',  ( 793.2243759319678702, -386.5328690171409676, -318.4439275373583200 ) ) ;
#24331 = DIRECTION ( 'NONE',  ( 0.000000000000000000, 0.000000000000000000, 1.000000000000000000 ) ) ;
#24332 = CARTESIAN_POINT ( 'NONE',  ( 785.3687786644885591, 12.63812461430668677, -315.3201227861280813 ) ) ;
#24333 = CARTESIAN_POINT ( 'NONE',  ( 763.8424801807145741, -114.0090635724258163, -320.5453621957614700 ) ) ;
#24334 = CARTESIAN_POINT ( 'NONE',  ( 788.6739635108323228, -391.6454272087885897, 373.9316612368139090 ) ) ;
#24335 = FACE_OUTER_BOUND ( 'NONE', #39346, .T. ) ;
#24336 = CARTESIAN_POINT ( 'NONE',  ( 788.7631598425961101, 22.55804007376682918, -305.7194118038759143 ) ) ;
#24337 = CARTESIAN_POINT ( 'NONE',  ( 745.0891759886404770, -316.2709662947832499, -342.4968714119734159 ) ) ;
#24338 = PLANE ( 'NONE',  #13569 ) ;
#24339 = DIRECTION ( 'NONE',  ( 0.000000000000000000, 0.000000000000000000, 1.000000000000000000 ) ) ;
#24340 = CARTESIAN_POINT ( 'NONE',  ( 762.1405469898971887, -73.54369356751118403, -357.8594530101015607 ) ) ;
#24341 = CARTESIAN_POINT ( 'NONE',  ( 812.3518521366052028, -241.0999726633345119, 326.5853460496235243 ) ) ;
#24342 = CARTESIAN_POINT ( 'NONE',  ( 746.0683387631852383, -163.4419599262325846, -331.3260364891676204 ) ) ;
#24343 = CARTESIAN_POINT ( 'NONE',  ( 782.4968714119720516, -178.8164208402381519, 305.0891759886411023 ) ) ;
#24344 = CARTESIAN_POINT ( 'NONE',  ( 801.1904061080336987, -428.0891481129644944, -368.3070685750235498 ) ) ;
#24345 = CARTESIAN_POINT ( 'NONE',  ( 779.9999999999992042, -452.9681489794448339, 339.9999999999999432 ) ) ;
#24346 = CARTESIAN_POINT ( 'NONE',  ( 785.3141322388236176, -285.7255117493286889, 364.4286716492789537 ) ) ;
#24347 = CARTESIAN_POINT ( 'NONE',  ( 757.0176451133909268, -61.09997266333506616, 349.9200121543848354 ) ) ;
#24348 = CARTESIAN_POINT ( 'NONE',  ( 755.5713283507202505, -437.3618753856919170, -334.6858677611754729 ) ) ;
#24349 = DIRECTION ( 'NONE',  ( 0.000000000000000000, -1.000000000000000000, 0.000000000000000000 ) ) ;
#24350 = DIRECTION ( 'NONE',  ( -0.000000000000000000, -0.000000000000000000, 1.000000000000000000 ) ) ;
#24352 = CARTESIAN_POINT ( 'NONE',  ( 771.1735550268778070, -321.1800572038740142, 316.3353852180827630 ) ) ;
#24351 = CARTESIAN_POINT ( 'NONE',  ( 757.2208543904082489, -136.7146871989600072, 350.9844846989624330 ) ) ;
#24353 = ORIENTED_EDGE ( 'NONE', *, *, #30000, .F. ) ;
#24354 = CARTESIAN_POINT ( 'NONE',  ( 779.4709603349208464, -264.3510508353232353, -314.7162404726379918 ) ) ;
#24355 = CARTESIAN_POINT ( 'NONE',  ( 788.7366044899766848, -83.90732993114754379, 316.5762568750059813 ) ) ;
#24356 = CARTESIAN_POINT ( 'NONE',  ( 807.5423716828161105, -273.0783235625958696, -362.2119215644372048 ) ) ;
#24357 = DIRECTION ( 'NONE',  ( 0.000000000000000000, 0.000000000000000000, 1.000000000000000000 ) ) ;
#24358 = CARTESIAN_POINT ( 'NONE',  ( 803.8556311672234642, -417.6237781080499190, 365.6418435158340117 ) ) ;
#24359 = EDGE_LOOP ( 'NONE', ( #11730, #35107 ) ) ;
#24360 = CARTESIAN_POINT ( 'NONE',  ( 797.8594530101008786, -277.5436935675105019, 322.1405469898980982 ) ) ;
#24361 = CARTESIAN_POINT ( 'NONE',  ( 787.6308680596127942, -35.26014174441480264, -364.1105419155492768 ) ) ;
#24362 = CARTESIAN_POINT ( 'NONE',  ( 762.3223304703356007, -151.5436935675109851, -322.3223304703362828 ) ) ;
#24363 = CARTESIAN_POINT ( 'NONE',  ( 804.9363028652555840, -208.2709662947835341, -338.2165204200192079 ) ) ;
#24364 = CARTESIAN_POINT ( 'NONE',  ( 797.8594530101008786, -397.5436935675100472, 322.1405469898980982 ) ) ;
#24365 = ADVANCED_FACE ( 'NONE', ( #42280, #41210 ), #10885, .F. ) ;
#24366 = CARTESIAN_POINT ( 'NONE',  ( 749.2812353651451076, -102.4527844766020337, -323.2262854647983090 ) ) ;
#24367 = CARTESIAN_POINT ( 'NONE',  ( 756.3353852180820240, -101.9073299311474869, -331.1735550268787733 ) ) ;
#24368 = ORIENTED_EDGE ( 'NONE', *, *, #28336, .T. ) ;
#24369 = CARTESIAN_POINT ( 'NONE',  ( 804.4086373105744769, -385.6454272087888171, -333.3843516231986541 ) ) ;
#24370 = CARTESIAN_POINT ( 'NONE',  ( 788.7366044899766848, -131.9073299311473875, 316.5762568750059813 ) ) ;
#24371 = CARTESIAN_POINT ( 'NONE',  ( 760.5453621957607311, -117.0783235625963528, 323.8424801807151425 ) ) ;
#24374 = CARTESIAN_POINT ( 'NONE',  ( 813.2346286133761168, -365.2601417444137155, 328.9521613784389160 ) ) ;
#24373 = CARTESIAN_POINT ( 'NONE',  ( -78.83651009197140525, 260.0000000000000568, -208.0249999999936108 ) ) ;
#24372 = LINE ( 'NONE', #14005, #11523 ) ;
#24375 = EDGE_CURVE ( 'NONE', #17707, #5383, #38841, .T. ) ;
#24376 = ORIENTED_EDGE ( 'NONE', *, *, #25533, .T. ) ;
#24377 = CARTESIAN_POINT ( 'NONE',  ( 804.8461984189677878, -362.1908817542432644, -336.9566956441385628 ) ) ;
#24378 = CARTESIAN_POINT ( 'NONE',  ( 802.1676090361156639, -350.6346026584192828, -327.8955696845344505 ) ) ;
#24379 = CARTESIAN_POINT ( 'NONE',  ( 757.7880784355613741, -162.0090635724256742, -312.4576283171834916 ) ) ;
#24380 = CARTESIAN_POINT ( 'NONE',  ( 791.0478386215596629, -21.82724539060792424, 306.7653713866226326 ) ) ;
#24382 = DIRECTION ( 'NONE',  ( -4.625929269271485914E-16, 1.000000000000000000, 0.000000000000000000 ) ) ;
#24381 = CARTESIAN_POINT ( 'NONE',  ( 200.7583438952259485, 394.6698570112193920, -274.9999999999999432 ) ) ;
#24383 = CARTESIAN_POINT ( 'NONE',  ( 800.7704444035546203, -292.1692326535048210, -326.0291762391768771 ) ) ;
#24384 = CARTESIAN_POINT ( 'NONE',  ( 785.3687786644884454, -443.3618753856917465, -315.3201227861279676 ) ) ;
#24385 = CARTESIAN_POINT ( 'NONE',  ( 795.8262568251477660, -142.3726999360620766, -308.3538107759623585 ) ) ;
#24386 = LINE ( 'NONE', #6403, #164 ) ;
#24387 = CARTESIAN_POINT ( 'NONE',  ( 799.9999999999993179, 205.0000000000000568, 265.0000000000000000 ) ) ;
#24388 = CARTESIAN_POINT ( 'NONE',  ( 755.8894580844503253, -375.8272453906069472, 332.3691319403863531 ) ) ;
#24389 = CARTESIAN_POINT ( 'NONE',  ( 812.3518521366052028, -337.0999726633342561, 326.5853460496235243 ) ) ;
#24390 = CARTESIAN_POINT ( 'NONE',  ( 772.4837098697145166, -191.3618753856926276, -374.5518280994205611 ) ) ;
#24391 = EDGE_CURVE ( 'NONE', #27295, #8740, #7193, .T. ) ;
#24392 = DIRECTION ( 'NONE',  ( -0.000000000000000000, 1.000000000000000000, -0.000000000000000000 ) ) ;
#24393 = CARTESIAN_POINT ( 'NONE',  ( 745.7194118038753459, -157.6454272087893287, 348.7631598425976449 ) ) ;
#24394 = EDGE_CURVE ( 'NONE', #13729, #22001, #17808, .T. ) ;
#24395 = CARTESIAN_POINT ( 'NONE',  ( 805.0032342141412300, -325.5436935675105019, -314.9967657858571783 ) ) ;
#24396 = CYLINDRICAL_SURFACE ( 'NONE', #32883, 30.00000000000008171 ) ;
#24397 = DIRECTION ( 'NONE',  ( -0.000000000000000000, 1.000000000000000000, -0.000000000000000000 ) ) ;
#24398 = EDGE_CURVE ( 'NONE', #20663, #29615, #32805, .T. ) ;
#24399 = CARTESIAN_POINT ( 'NONE',  ( 795.1360043628807261, -188.0891481129653187, 360.2193346964456282 ) ) ;
#24400 = VERTEX_POINT ( 'NONE', #22619 ) ;
#24401 = CARTESIAN_POINT ( 'NONE',  ( 810.4231160770870019, -432.5545181178793541, 321.9338519418446936 ) ) ;
#24402 = CARTESIAN_POINT ( 'NONE',  ( 783.7566961878529810, -384.8965053807772847, -305.1792804349288417 ) ) ;
#24403 = CARTESIAN_POINT ( 'NONE',  ( 792.3570229623688874, -141.1800572038746395, -373.1304606946836202 ) ) ;
#24404 = CARTESIAN_POINT ( 'NONE',  ( 792.3570229623688874, -429.1800572038737869, -373.1304606946836202 ) ) ;
#24405 = CARTESIAN_POINT ( 'NONE',  ( -338.8365100919713200, 256.5000000000001137, -193.8809999999918148 ) ) ;
#24406 = CARTESIAN_POINT ( 'NONE',  ( 815.1787889125755555, -6.896505380778533478, 343.7953271457877804 ) ) ;
#24407 = VERTEX_POINT ( 'NONE', #1385 ) ;
#24408 = CARTESIAN_POINT ( 'NONE',  ( 758.0141637701419768, -159.0783235625962391, -367.2620300519063790 ) ) ;
#24409 = CARTESIAN_POINT ( 'NONE',  ( 999.9999999999992042, 479.5857864376268935, 200.4142135623730496 ) ) ;
#24410 = CARTESIAN_POINT ( 'NONE',  ( 815.0009284576459549, -318.3510508353230080, 338.7629533639073429 ) ) ;
#24411 = CARTESIAN_POINT ( 'NONE',  ( 794.9819416627830151, -132.9982390220564810, 319.9864689768909898 ) ) ;
#24412 = ORIENTED_EDGE ( 'NONE', *, *, #16520, .F. ) ;
#24413 = EDGE_CURVE ( 'NONE', #44613, #36817, #25173, .T. ) ;
#24414 = CARTESIAN_POINT ( 'NONE',  ( 755.3201227861273992, -315.7255117493286320, 345.3687786644892981 ) ) ;
#24415 = ADVANCED_FACE ( 'NONE', ( #11793 ), #29568, .F. ) ;
#24416 = CARTESIAN_POINT ( 'NONE',  ( 804.7487373415286811, 4.456306432488530866, -364.7487373415288516 ) ) ;
#24417 = CARTESIAN_POINT ( 'NONE',  ( 789.4860707548003802, -452.3212000445050762, 363.1417840971553233 ) ) ;
#24418 = VERTEX_POINT ( 'NONE', #36048 ) ;
#24419 = CARTESIAN_POINT ( 'NONE',  ( 811.3240766477731540, -412.3726999360612808, -355.6651683502462902 ) ) ;
#24420 = VERTEX_POINT ( 'NONE', #39530 ) ;
#24421 = CARTESIAN_POINT ( 'NONE',  ( 803.4237431249931660, -39.18005720387496638, 331.2633955100225194 ) ) ;
#24422 = CARTESIAN_POINT ( 'NONE',  ( 759.7806653035534055, -246.9982390220560546, -324.8639956371180801 ) ) ;
#24423 = EDGE_CURVE ( 'NONE', #30803, #34298, #15264, .T. ) ;
#24425 = CARTESIAN_POINT ( 'NONE',  ( 759.8311093483677041, -238.1692326535050768, 310.9282345327691814 ) ) ;
#24424 = CARTESIAN_POINT ( 'NONE',  ( 787.5162901302840055, -347.3618753856922012, 305.4481719005793252 ) ) ;
#24426 = ADVANCED_FACE ( 'NONE', ( #43198 ), #43257, .F. ) ;
#24427 = CARTESIAN_POINT ( 'NONE',  ( 805.9055244015594326, -75.62377810805104161, 315.8990559732753240 ) ) ;
#24428 = CARTESIAN_POINT ( 'NONE',  ( 780.5236548040995785, -260.7363362996981095, -314.9735926884559944 ) ) ;
#24429 = CARTESIAN_POINT ( 'NONE',  ( 757.8323909638827445, -266.6346026584197375, -352.1044303154654358 ) ) ;
#24430 = DIRECTION ( 'NONE',  ( -1.880165489482579047E-16, -1.000000000000000000, -0.000000000000000000 ) ) ;
#24431 = CARTESIAN_POINT ( 'NONE',  ( 762.1405469898971887, -97.54369356751112718, -357.8594530101015607 ) ) ;
#24432 = CARTESIAN_POINT ( 'NONE',  ( 792.1044303154645831, -228.4527844766015789, 317.8323909638837677 ) ) ;
#24433 = ORIENTED_EDGE ( 'NONE', *, *, #24100, .T. ) ;
#24434 = CARTESIAN_POINT ( 'NONE',  ( 767.7687537140311633, -407.9073299311465348, 372.7932403749916830 ) ) ;
#24435 = FACE_OUTER_BOUND ( 'NONE', #5174, .T. ) ;
#24436 = CARTESIAN_POINT ( 'NONE',  ( 768.9521613784389729, -57.82724539060780700, -373.2346286133773106 ) ) ;
#24437 = DIRECTION ( 'NONE',  ( 0.000000000000000000, 0.000000000000000000, -1.000000000000000000 ) ) ;
#24438 = CYLINDRICAL_SURFACE ( 'NONE', #18650, 24.99999999999991118 ) ;
#24439 = CARTESIAN_POINT ( 'NONE',  ( 761.4292242960306112, -257.4636090269708575, 323.2154366446414429 ) ) ;
#24440 = CARTESIAN_POINT ( 'NONE',  ( 768.0187753319979720, -104.6346026584202207, 318.0580252608186242 ) ) ;
#24441 = ORIENTED_EDGE ( 'NONE', *, *, #22148, .T. ) ;
#24442 = CARTESIAN_POINT ( 'NONE',  ( 796.1575198192839480, -6.009063572426154742, -359.4546378042384163 ) ) ;
#24443 = AXIS2_PLACEMENT_3D ( 'NONE', #29581, #8791, #43657 ) ;
#24444 = CARTESIAN_POINT ( 'NONE',  ( 800.9747183278959710, -60.99823902205671544, -311.9810565676471583 ) ) ;
#24445 = CARTESIAN_POINT ( 'NONE',  ( 757.2208543904082489, -304.7146871989594388, 350.9844846989624330 ) ) ;
#24446 = CARTESIAN_POINT ( 'NONE',  ( 799.9999999999993179, 205.0000000000000568, 319.9999999999999432 ) ) ;
#24447 = CARTESIAN_POINT ( 'NONE',  ( 776.2046728542105711, 3.809118245755632959, 304.8212110874238761 ) ) ;
#24448 = CARTESIAN_POINT ( 'NONE',  ( 810.7187646348534145, -186.4527844766017779, -356.7737145352016341 ) ) ;
#24449 = CARTESIAN_POINT ( 'NONE',  ( 782.5225473063381969, -190.2709662947835909, 375.2698199232970637 ) ) ;
#24450 = CARTESIAN_POINT ( 'NONE',  ( 795.1360043628807261, -68.08914811296575920, 360.2193346964456282 ) ) ;
#24451 = DIRECTION ( 'NONE',  ( 0.000000000000000000, 0.000000000000000000, -1.000000000000000000 ) ) ;
#24452 = CARTESIAN_POINT ( 'NONE',  ( 801.9858362298568863, -267.0783235625958696, -312.7379699480935642 ) ) ;
#24453 = CARTESIAN_POINT ( 'NONE',  ( 748.6759233522253680, -448.3726999360611103, 324.3348316497537098 ) ) ;
#24454 = CARTESIAN_POINT ( 'NONE',  ( 792.2312462859673587, -275.9073299311469896, -307.2067596250082602 ) ) ;
#24455 = DIRECTION ( 'NONE',  ( 1.000000000000000000, 0.000000000000000000, 0.000000000000000000 ) ) ;
#24456 = CARTESIAN_POINT ( 'NONE',  ( 804.1601925771018387, -367.4419599262319025, 346.5483106153029098 ) ) ;
#24457 = CARTESIAN_POINT ( 'NONE',  ( 763.0537975583476964, -48.45278447660221133, 371.0346526505628617 ) ) ;
#24458 = CARTESIAN_POINT ( 'NONE',  ( 813.2346286133761168, -29.26014174441482751, -328.9521613784389160 ) ) ;
#24459 = CARTESIAN_POINT ( 'NONE',  ( 759.7806653035534055, -390.9982390220557136, -324.8639956371180801 ) ) ;
#24460 = CARTESIAN_POINT ( 'NONE',  ( 798.7617431975189675, -3.623778108051270319, 323.0428371773161871 ) ) ;
#24461 = CARTESIAN_POINT ( 'NONE',  ( 810.1134526219336749, -56.53286901714201917, -357.8822607201570349 ) ) ;
#24462 = CARTESIAN_POINT ( 'NONE',  ( 787.6308680596127942, -203.2601417444143124, -364.1105419155492768 ) ) ;
#24463 = CARTESIAN_POINT ( 'NONE',  ( 807.5423716828161105, -201.0783235625961254, 362.2119215644372048 ) ) ;
#24464 = CARTESIAN_POINT ( 'NONE',  ( 785.3687786644885591, -11.36187538569323863, 315.3201227861280813 ) ) ;
#24465 = EDGE_CURVE ( 'NONE', #13889, #32644, #15489, .T. ) ;
#24466 = CARTESIAN_POINT ( 'NONE',  ( 784.0799538623451781, -371.8055962898682765, 364.6971507214555572 ) ) ;
#24467 = ORIENTED_EDGE ( 'NONE', *, *, #32624, .T. ) ;
#24468 = CARTESIAN_POINT ( 'NONE',  ( 754.9735926884551418, -186.3510508353234343, -340.5236548041000333 ) ) ;
#24469 = CARTESIAN_POINT ( 'NONE',  ( 804.4286716492782716, -185.3618753856926844, 345.3141322388244703 ) ) ;
#24470 = CARTESIAN_POINT ( 'NONE',  ( 756.1443688327750579, -45.62377810805114109, -314.3581564841659315 ) ) ;
#24471 = CARTESIAN_POINT ( 'NONE',  ( 765.0180583372156207, -336.9982390220558273, 360.0135310231089534 ) ) ;
#24472 = VECTOR ( 'NONE', #8893, 1000.000000000000000 ) ;
#24473 = CARTESIAN_POINT ( 'NONE',  ( -949.5497976682736407, 120.6654763175833693, 339.9999999999999432 ) ) ;
#24474 = VERTEX_POINT ( 'NONE', #12014 ) ;
#24475 = CARTESIAN_POINT ( 'NONE',  ( 756.7813123517142913, -67.98741447168742980, 329.9779781133712504 ) ) ;
#24476 = CARTESIAN_POINT ( 'NONE',  ( 771.3260364891663130, -307.6454272087888171, -306.0683387631859773 ) ) ;
#24477 = EDGE_CURVE ( 'NONE', #28297, #34711, #20364, .T. ) ;
#24478 = CARTESIAN_POINT ( 'NONE',  ( 763.0537975583476964, -240.4527844766015789, 371.0346526505628617 ) ) ;
#24479 = CARTESIAN_POINT ( 'NONE',  ( 759.0159684113467620, -352.9181544815159555, 325.8855110935213020 ) ) ;
#24480 = CARTESIAN_POINT ( 'NONE',  ( 808.7758568127978833, 19.83076734649410966, 320.0363995740631822 ) ) ;
#24481 = CARTESIAN_POINT ( 'NONE',  ( 757.0176451133909268, -133.0999726633348246, -349.9200121543848354 ) ) ;
#24482 = CARTESIAN_POINT ( 'NONE',  ( 801.9419747391806368, -138.4527844766019200, -351.9812246680014027 ) ) ;
#24483 = CARTESIAN_POINT ( 'NONE',  ( 804.9363028652555840, -352.2709662947830225, -338.2165204200192079 ) ) ;
#24484 = ORIENTED_EDGE ( 'NONE', *, *, #24171, .T. ) ;
#24485 = CARTESIAN_POINT ( 'NONE',  ( 767.6429770376289525, -297.1800572038740711, 306.8695393053162093 ) ) ;
#24486 = CARTESIAN_POINT ( 'NONE',  ( 804.1601925771018387, -319.4419599262320730, 346.5483106153029098 ) ) ;
#24487 = CARTESIAN_POINT ( 'NONE',  ( 799.9999999999993179, -512.9681489794448908, -339.9999999999999432 ) ) ;
#24488 = CARTESIAN_POINT ( 'NONE',  ( 804.1105419155481968, -123.8272453906076009, 347.6308680596136469 ) ) ;
#24489 = CARTESIAN_POINT ( 'NONE',  ( 788.8264449731200330, -21.18005720387502677, 363.6646147819171233 ) ) ;
#24490 = ORIENTED_EDGE ( 'NONE', *, *, #38844, .F. ) ;
#24491 = CARTESIAN_POINT ( 'NONE',  ( 764.1737431748507561, -370.3726999360613377, -371.6461892240376415 ) ) ;
#24492 = AXIS2_PLACEMENT_3D ( 'NONE', #2512, #45027, #16617 ) ;
#24493 = CARTESIAN_POINT ( 'NONE',  ( -26.63011601220122060, -563.3203001761230553, -342.3463313526983143 ) ) ;
#24494 = CARTESIAN_POINT ( 'NONE',  ( 778.7629533639073998, -248.7363362996981380, 375.0009284576466371 ) ) ;
#24495 = CARTESIAN_POINT ( 'NONE',  ( 794.1144889064781864, -178.1692326535052473, 360.9840315886528401 ) ) ;
#24496 = CARTESIAN_POINT ( 'NONE',  ( 774.6858677611749044, -321.7255117493286320, -315.5713283507209894 ) ) ;
#24497 = CARTESIAN_POINT ( 'NONE',  ( -26.63011601220122060, -512.9681489794448908, -339.9999999999999432 ) ) ;
#24498 = CARTESIAN_POINT ( 'NONE',  ( 769.0155153010367712, -226.3726999360617924, -362.7791456095907279 ) ) ;
#24499 = CARTESIAN_POINT ( 'NONE',  ( 747.2067596250078623, -27.18005720387500901, 352.2312462859687230 ) ) ;
#24500 = CARTESIAN_POINT ( 'NONE',  ( 755.2512626584698410, -79.54369356751119824, 315.2512626584710915 ) ) ;
#24501 = LINE ( 'NONE', #20134, #14403 ) ;
#24502 = CARTESIAN_POINT ( 'NONE',  ( 777.4774526936600978, -418.2709662947828519, -304.7301800767028226 ) ) ;
#24503 = DIRECTION ( 'NONE',  ( 0.000000000000000000, 0.000000000000000000, -1.000000000000000000 ) ) ;
#24504 = CARTESIAN_POINT ( 'NONE',  ( 755.8990559732751535, -347.4636090269705733, 365.9055244015606831 ) ) ;
#24505 = DIRECTION ( 'NONE',  ( 0.000000000000000000, 0.000000000000000000, 1.000000000000000000 ) ) ;
#24506 = CARTESIAN_POINT ( 'NONE',  ( 759.0252816721024374, -312.9982390220559409, 368.0189434323527280 ) ) ;
#24507 = CARTESIAN_POINT ( 'NONE',  ( 745.0891759886404770, -52.27096629478401724, -342.4968714119734159 ) ) ;
#24508 = CARTESIAN_POINT ( 'NONE',  ( 762.1405469898971887, -265.5436935675106156, -357.8594530101015607 ) ) ;
#24509 = FACE_BOUND ( 'NONE', #43316, .T. ) ;
#24510 = CARTESIAN_POINT ( 'NONE',  ( 801.9419747391806368, -402.4527844766010389, 351.9812246680014027 ) ) ;
#24511 = CARTESIAN_POINT ( 'NONE',  ( 790.0220218866281812, -151.0999726633347677, 363.2186876482849129 ) ) ;
#24512 = CARTESIAN_POINT ( 'NONE',  ( 750.9282345327678740, -40.91815448151695023, -319.8311093483690115 ) ) ;
#24513 = CARTESIAN_POINT ( 'NONE',  ( 800.7704444035546203, -100.1692326535055315, -326.0291762391768771 ) ) ;
#24514 = CARTESIAN_POINT ( 'NONE',  ( 814.8230680027162407, -53.80559628986930676, 333.7305795820267917 ) ) ;
#24515 = CARTESIAN_POINT ( 'NONE',  ( 759.9864689768902508, -410.0891481129647218, 354.9819416627836404 ) ) ;
#24516 = CARTESIAN_POINT ( 'NONE',  ( -78.83651009197140525, 230.0000000000000568, -197.2499999999937756 ) ) ;
#24517 = CARTESIAN_POINT ( 'NONE',  ( 989.9999999999992042, 56.78581973499402835, 212.6378164459127049 ) ) ;
#24518 = CARTESIAN_POINT ( 'NONE',  ( 807.5423716828161105, -153.0783235625962675, 362.2119215644372048 ) ) ;
#24519 = CARTESIAN_POINT ( 'NONE',  ( 802.1676090361156639, 9.365397341579420498, -327.8955696845344505 ) ) ;
#24521 = ORIENTED_EDGE ( 'NONE', *, *, #45346, .T. ) ;
#24520 = CARTESIAN_POINT ( 'NONE',  ( 796.7845633553578182, -105.6237781080509421, -358.5707757039688204 ) ) ;
#24522 = CARTESIAN_POINT ( 'NONE',  ( 764.8639956371174549, -56.08914811296580893, -319.7806653035542013 ) ) ;
#24523 = CARTESIAN_POINT ( 'NONE',  ( 784.0799538623451781, -395.8055962898682765, -364.6971507214555572 ) ) ;
#24525 = CARTESIAN_POINT ( 'NONE',  ( 756.5762568750052424, -243.1800572038743269, 348.7366044899774238 ) ) ;
#24524 = CARTESIAN_POINT ( 'NONE',  ( 803.4237431249931660, -231.1800572038743553, 331.2633955100225194 ) ) ;
#24526 = CIRCLE ( 'NONE', #42217, 2.749999999999835687 ) ;
#24527 = CARTESIAN_POINT ( 'NONE',  ( 795.6651683502461765, -394.7146871989591546, -371.3240766477733814 ) ) ;
#24528 = CARTESIAN_POINT ( 'NONE',  ( 115.7583438952258774, 290.0000000000001705, -244.9999999999999716 ) ) ;
#24529 = EDGE_LOOP ( 'NONE', ( #10747, #130, #6592, #27288 ) ) ;
#24530 = CARTESIAN_POINT ( 'NONE',  ( 774.6858677611749044, -441.7255117493282910, 315.5713283507209894 ) ) ;
#24531 = EDGE_LOOP ( 'NONE', ( #23845, #43413, #7373, #22212 ) ) ;
#24532 = CARTESIAN_POINT ( 'NONE',  ( 744.7301800767019131, -244.8164208402378961, -337.4774526936615757 ) ) ;
#24533 = CARTESIAN_POINT ( 'NONE',  ( 758.8095938919644823, -152.0891481129655460, 311.6929314249762797 ) ) ;
#24534 = ORIENTED_EDGE ( 'NONE', *, *, #23250, .T. ) ;
#24535 = CARTESIAN_POINT ( 'NONE',  ( 767.8955696845334842, -240.4527844766015789, -362.1676090361161755 ) ) ;
#24536 = EDGE_LOOP ( 'NONE', ( #11336, #3595, #21541, #22358 ) ) ;
#24537 = CARTESIAN_POINT ( 'NONE',  ( 797.8594530101008786, -349.5436935675102745, -322.1405469898980982 ) ) ;
#24538 = CARTESIAN_POINT ( 'NONE',  ( 800.0135310231082713, -14.08914811296595460, -325.0180583372163028 ) ) ;
#24539 = CARTESIAN_POINT ( 'NONE',  ( 786.6156483768007774, -217.4419599262324141, 315.5913626894246136 ) ) ;
#24540 = CARTESIAN_POINT ( 'NONE',  ( -521.6730038022808458, 9.808315785437627339E-14, 350.0000000000000000 ) ) ;
#24541 = FACE_OUTER_BOUND ( 'NONE', #17769, .T. ) ;
#24542 = ORIENTED_EDGE ( 'NONE', *, *, #11724, .T. ) ;
#24543 = CARTESIAN_POINT ( 'NONE',  ( 785.3687786644884454, -11.36187538569323863, -315.3201227861279676 ) ) ;
#24544 = CARTESIAN_POINT ( 'NONE',  ( 775.4999999999993179, -512.9681489794448908, -327.9999999999999432 ) ) ;
#24545 = CARTESIAN_POINT ( 'NONE',  ( 784.9999999999992042, 205.0000000000000568, -255.0000000000000000 ) ) ;
#24546 = ORIENTED_EDGE ( 'NONE', *, *, #36196, .F. ) ;
#24547 = CARTESIAN_POINT ( 'NONE',  ( 746.4236121716829757, -279.8272453906071746, -328.8385539511384650 ) ) ;
#24548 = CARTESIAN_POINT ( 'NONE',  ( 814.4686193811664907, -147.2817908451529547, 346.2056067578752732 ) ) ;
#24550 = CARTESIAN_POINT ( 'NONE',  ( 797.6776695296629214, -235.5436935675107293, -357.6776695296636603 ) ) ;
#24549 = LINE ( 'NONE', #41675, #43090 ) ;
#24551 = CARTESIAN_POINT ( 'NONE',  ( 755.0488828828309806, -401.8055962898681059, -344.1219089521771934 ) ) ;
#24552 = LINE ( 'NONE', #38435, #25242 ) ;
#24553 = FACE_OUTER_BOUND ( 'NONE', #9436, .T. ) ;
#24554 = CARTESIAN_POINT ( 'NONE',  ( 772.4468031744293057, -129.8272453906075725, -363.8651313633793620 ) ) ;
#24555 = LINE ( 'NONE', #38439, #29849 ) ;
#24556 = CARTESIAN_POINT ( 'NONE',  ( 754.0944755984390895, 8.376221891948691933, -364.1009440267246760 ) ) ;
#24557 = CARTESIAN_POINT ( 'NONE',  ( 759.0252816721024374, -312.9982390220559409, -368.0189434323527280 ) ) ;
#24558 = CARTESIAN_POINT ( 'NONE',  ( 187.1337867209877857, 62.85347435602256638, 357.4246812887967053 ) ) ;
#24559 = CARTESIAN_POINT ( 'NONE',  ( 799.9999999999993179, 205.0000000000000568, -339.9999999999999432 ) ) ;
#24560 = CARTESIAN_POINT ( 'NONE',  ( 781.8018195045266339, -94.27096629478386092, -365.1927285166406705 ) ) ;
#24561 = CARTESIAN_POINT ( 'NONE',  ( 812.6845335610512393, -271.9874144716868045, -353.5525998758768651 ) ) ;
#24562 = CARTESIAN_POINT ( 'NONE',  ( 814.2805881961230625, -241.6454272087890729, 331.2368401574024119 ) ) ;
#24563 = CARTESIAN_POINT ( 'NONE',  ( 776.2433038121456548, -204.8965053807779100, -374.8207195650711014 ) ) ;
#24564 = CARTESIAN_POINT ( 'NONE',  ( 796.9462024416508257, -180.4527844766017211, 308.9653473494370246 ) ) ;
#24565 = CARTESIAN_POINT ( 'NONE',  ( 763.0537975583475827, -432.4527844766008684, -371.0346526505627480 ) ) ;
#24566 = DIRECTION ( 'NONE',  ( -1.000000000000000000, 0.000000000000000000, 0.000000000000000000 ) ) ;
#24567 = CARTESIAN_POINT ( 'NONE',  ( 791.9812246680005501, -284.6346026584196807, 361.9419747391813189 ) ) ;
#24568 = CARTESIAN_POINT ( 'NONE',  ( 793.9708237608222134, -94.91815448151677970, 319.2295555964448681 ) ) ;
#24569 = CARTESIAN_POINT ( 'NONE',  ( 775.9200461376533440, 24.19440371013046231, -315.3028492785443291 ) ) ;
#24570 = CARTESIAN_POINT ( 'NONE',  ( -115.7583438952258774, 290.0000000000001137, -244.9999999999999716 ) ) ;
#24571 = MECHANICAL_DESIGN_GEOMETRIC_PRESENTATION_REPRESENTATION (  '', ( #40809 ), #12772 ) ;
#24572 = CARTESIAN_POINT ( 'NONE',  ( 911.9999999999993179, 154.9999999999998863, 360.0000000000000000 ) ) ;
#24574 = CARTESIAN_POINT ( 'NONE',  ( 754.8072714833581358, -316.8164208402377540, 338.1981804954720587 ) ) ;
#24573 = CARTESIAN_POINT ( 'NONE',  ( 756.7813123517142913, -139.9874144716872024, 329.9779781133712504 ) ) ;
#24575 = EDGE_LOOP ( 'NONE', ( #43243, #1042 ) ) ;
#24576 = CARTESIAN_POINT ( 'NONE',  ( 790.8726784830453198, -274.7146871989594388, -362.5472867521010585 ) ) ;
#24577 = CARTESIAN_POINT ( 'NONE',  ( 804.4286716492782716, -89.36187538569299704, 345.3141322388244703 ) ) ;
#24578 = EDGE_CURVE ( 'NONE', #14210, #6074, #39763, .T. ) ;
#24579 = CARTESIAN_POINT ( 'NONE',  ( 810.1134526219336749, -296.5328690171411949, -357.8822607201570349 ) ) ;
#24580 = DIRECTION ( 'NONE',  ( -1.084653538143406060E-16, 0.6594541114781790059, -0.7517448203044204691 ) ) ;
#24581 = CARTESIAN_POINT ( 'NONE',  ( 758.0141637701419768, -423.0783235625953580, 367.2620300519063790 ) ) ;
#24582 = EDGE_LOOP ( 'NONE', ( #7069, #31118, #37248, #39719 ) ) ;
#24583 = CARTESIAN_POINT ( 'NONE',  ( 803.4237431249931660, -303.1800572038740711, 331.2633955100225194 ) ) ;
#24584 = CARTESIAN_POINT ( 'NONE',  ( 776.9566956441375396, -36.89650538077844288, -364.8461984189686405 ) ) ;
#24585 = CARTESIAN_POINT ( 'NONE',  ( 774.6312213355099630, -167.3618753856927412, -364.6798772138717482 ) ) ;
#24586 = CARTESIAN_POINT ( 'NONE',  ( 804.6798772138708955, -207.7255117493289447, -334.6312213355107019 ) ) ;
#24587 = CARTESIAN_POINT ( 'NONE',  ( 794.9819416627830151, -396.9982390220556567, 319.9864689768909898 ) ) ;
#24588 = CARTESIAN_POINT ( 'NONE',  ( 777.4774526936600978, -154.2709662947836478, -304.7301800767027657 ) ) ;
#24589 = CARTESIAN_POINT ( 'NONE',  ( 778.1981804954715471, -106.2709662947838467, -314.8072714833591021 ) ) ;
#24590 = ORIENTED_EDGE ( 'NONE', *, *, #13973, .F. ) ;
#24591 = CARTESIAN_POINT ( 'NONE',  ( 757.0176451133909268, -373.0999726633340856, -349.9200121543848354 ) ) ;
#24593 = CARTESIAN_POINT ( 'NONE',  ( 766.0291762391763086, -442.9181544815157849, 360.7704444035551319 ) ) ;
#24592 = CARTESIAN_POINT ( 'NONE',  ( 804.6798772138708955, -135.7255117493291152, 334.6312213355107019 ) ) ;
#24594 = CARTESIAN_POINT ( 'NONE',  ( 756.7813123517142913, -115.9874144716872877, 329.9779781133712504 ) ) ;
#24597 = CARTESIAN_POINT ( 'NONE',  ( 764.3348316497523456, -406.7146871989590409, 308.6759233522265617 ) ) ;
#24596 = DIRECTION ( 'NONE',  ( -1.000000000000000000, -0.000000000000000000, -0.000000000000000000 ) ) ;
#24595 = FACE_OUTER_BOUND ( 'NONE', #29701, .T. ) ;
#24598 = ORIENTED_EDGE ( 'NONE', *, *, #15628, .T. ) ;
#24599 = EDGE_CURVE ( 'NONE', #2565, #18281, #4410, .T. ) ;
#24600 = CARTESIAN_POINT ( 'NONE',  ( 758.4439275373578084, -348.5545181178796383, -353.2243759319684386 ) ) ;
#24601 = CARTESIAN_POINT ( 'NONE',  ( 767.8955696845333705, -360.4527844766010958, -362.1676090361162323 ) ) ;
#24602 = CARTESIAN_POINT ( 'NONE',  ( 778.7629533639073998, -152.7363362996983938, -375.0009284576466371 ) ) ;
#24603 = CARTESIAN_POINT ( 'NONE',  ( 783.7953271457878373, -32.19088175424425913, 375.1787889125761239 ) ) ;
#24604 = AXIS2_PLACEMENT_3D ( 'NONE', #26598, #9053, #11851 ) ;
#24606 = DIRECTION ( 'NONE',  ( 0.000000000000000000, -0.7651688349527138167, 0.6438296778008192334 ) ) ;
#24605 = DIRECTION ( 'NONE',  ( -0.000000000000000000, -0.000000000000000000, 1.000000000000000000 ) ) ;
#24607 = CARTESIAN_POINT ( 'NONE',  ( 789.9200121543843807, -289.9874144716866908, -317.0176451133914384 ) ) ;
#24608 = CARTESIAN_POINT ( 'NONE',  ( 774.6858677611749044, -441.7255117493282910, -315.5713283507209894 ) ) ;
#24609 = CARTESIAN_POINT ( 'NONE',  ( 804.1009440267234822, -167.4636090269711133, -314.0944755984392600 ) ) ;
#24610 = CYLINDRICAL_SURFACE ( 'NONE', #35963, 30.00000000000002842 ) ;
#24611 = DIRECTION ( 'NONE',  ( -0.000000000000000000, 1.000000000000000000, -0.000000000000000000 ) ) ;
#24612 = CARTESIAN_POINT ( 'NONE',  ( 776.9254006560222479, -356.1908817542432075, 314.8983024940802125 ) ) ;
#24613 = CARTESIAN_POINT ( 'NONE',  ( 814.4686193811664907, -339.2817908451524431, 346.2056067578752732 ) ) ;
#24614 = CARTESIAN_POINT ( 'NONE',  ( 744.7301800767020268, -196.8164208402380950, -337.4774526936615189 ) ) ;
#24615 = CARTESIAN_POINT ( 'NONE',  ( -208.8365100919714052, 240.0000000000001137, -197.2499999999928377 ) ) ;
#24616 = CYLINDRICAL_SURFACE ( 'NONE', #28405, 6.119000000000013095 ) ;
#24617 = CARTESIAN_POINT ( 'NONE',  ( 812.3518521366052028, -145.0999726633347677, 326.5853460496235243 ) ) ;
#24618 = CARTESIAN_POINT ( 'NONE',  ( 748.3538107759620743, -112.7146871989600356, -355.8262568251490165 ) ) ;
#24619 = CARTESIAN_POINT ( 'NONE',  ( 814.2001403089898304, -353.3618753856922012, -347.4397851343538264 ) ) ;
#24620 = EDGE_CURVE ( 'NONE', #28279, #13947, #7640, .T. ) ;
#24621 = DIRECTION ( 'NONE',  ( -0.000000000000000000, 1.000000000000000000, -0.000000000000000000 ) ) ;
#24622 = DIRECTION ( 'NONE',  ( -1.000000000000000000, -0.000000000000000000, -0.000000000000000000 ) ) ;
#24623 = CARTESIAN_POINT ( 'NONE',  ( 781.7834795799800531, -178.8164208402381519, 315.0636971347436202 ) ) ;
#24624 = AXIS2_PLACEMENT_3D ( 'NONE', #24112, #20198, #27143 ) ;
#24625 = CARTESIAN_POINT ( 'NONE',  ( -208.8365100919714052, 260.0000000000001137, -199.9999999999926956 ) ) ;
#24626 = VECTOR ( 'NONE', #29632, 1000.000000000000000 ) ;
#24627 = CARTESIAN_POINT ( 'NONE',  ( 745.1792804349281596, -446.1908817542429802, 343.7566961878542884 ) ) ;
#24628 = CARTESIAN_POINT ( 'NONE',  ( 803.8556311672234642, -369.6237781080500895, -365.6418435158340117 ) ) ;
#24629 = CARTESIAN_POINT ( 'NONE',  ( 787.4397851343537695, -141.7255117493291721, -374.2001403089903988 ) ) ;
#24630 = CARTESIAN_POINT ( 'NONE',  ( 796.9462024416508257, -420.4527844766009252, -308.9653473494370246 ) ) ;
#24631 = FACE_OUTER_BOUND ( 'NONE', #36912, .T. ) ;
#24632 = CARTESIAN_POINT ( 'NONE',  ( 795.6651683502461765, -10.71468719896033761, 371.3240766477733814 ) ) ;
#24633 = ORIENTED_EDGE ( 'NONE', *, *, #42896, .F. ) ;
#24634 = ADVANCED_FACE ( 'NONE', ( #35812, #4619 ), #36488, .F. ) ;
#24635 = CARTESIAN_POINT ( 'NONE',  ( 811.6461892240364477, -196.7146871989598083, -324.1737431748509835 ) ) ;
#24636 = SURFACE_STYLE_USAGE ( .BOTH. , #30905 ) ;
#24637 = CARTESIAN_POINT ( 'NONE',  ( 815.1787889125755555, -294.8965053807775689, 343.7953271457877804 ) ) ;
#24638 = CARTESIAN_POINT ( 'NONE',  ( 785.3687786644885591, -107.3618753856928976, 315.3201227861280813 ) ) ;
#24639 = ORIENTED_EDGE ( 'NONE', *, *, #37651, .T. ) ;
#24640 = EDGE_CURVE ( 'NONE', #791, #282, #22171, .T. ) ;
#24641 = AXIS2_PLACEMENT_3D ( 'NONE', #25622, #22356, #18254 ) ;
#24642 = CARTESIAN_POINT ( 'NONE',  ( 803.4237431249931660, -303.1800572038740711, 331.2633955100225194 ) ) ;
#24643 = CIRCLE ( 'NONE', #8449, 6.118999999999985562 ) ;
#24644 = CARTESIAN_POINT ( 'NONE',  ( 745.4481719005789273, -3.725511749329622813, -347.5162901302853129 ) ) ;
#24645 = CARTESIAN_POINT ( 'NONE',  ( -879.9999999999992042, 260.0000000000002274, -219.9999999999999716 ) ) ;
#24646 = EDGE_CURVE ( 'NONE', #2495, #17065, #1159, .T. ) ;
#24647 = ORIENTED_EDGE ( 'NONE', *, *, #22756, .T. ) ;
#24648 = CARTESIAN_POINT ( 'NONE',  ( 778.7629533639073998, -416.7363362996975980, -375.0009284576466371 ) ) ;
#24649 = ORIENTED_EDGE ( 'NONE', *, *, #39488, .T. ) ;
#24650 = PRODUCT_CONTEXT ( 'NONE', #27853, 'mechanical' ) ;
#24651 = EDGE_CURVE ( 'NONE', #9763, #5059, #712, .T. ) ;
#24652 = CARTESIAN_POINT ( 'NONE',  ( 756.5762568750052424, -27.18005720387500901, 348.7366044899774238 ) ) ;
#24653 = CARTESIAN_POINT ( 'NONE',  ( 788.7366044899766848, -275.9073299311469896, -316.5762568750059813 ) ) ;
#24655 = CARTESIAN_POINT ( 'NONE',  ( 805.9055244015594326, -291.6237781080503169, 315.8990559732753240 ) ) ;
#24654 = CARTESIAN_POINT ( 'NONE',  ( 787.4397851343537695, -357.7255117493285184, 374.2001403089903988 ) ) ;
#24656 = CARTESIAN_POINT ( 'NONE',  ( 795.6651683502461765, -82.71468719896012090, 371.3240766477733814 ) ) ;
#24657 = ADVANCED_FACE ( 'NONE', ( #5079 ), #26080, .T. ) ;
#24658 = CARTESIAN_POINT ( 'NONE',  ( 755.8894580844503253, -255.8272453906072315, -332.3691319403863531 ) ) ;
#24659 = CARTESIAN_POINT ( 'NONE',  ( 759.7806653035534055, -246.9982390220560546, -324.8639956371180801 ) ) ;
#24660 = LINE ( 'NONE', #42229, #26041 ) ;
#24661 = CARTESIAN_POINT ( 'NONE',  ( 804.9363028652555840, -112.2709662947838325, -338.2165204200192079 ) ) ;
#24662 = AXIS2_PLACEMENT_3D ( 'NONE', #6047, #26164, #33547 ) ;
#24663 = CARTESIAN_POINT ( 'NONE',  ( 801.9419747391806368, -258.4527844766016074, 351.9812246680014027 ) ) ;
#24664 = CARTESIAN_POINT ( 'NONE',  ( 767.6429770376289525, -393.1800572038737300, 306.8695393053162093 ) ) ;
#24666 = DIRECTION ( 'NONE',  ( 0.000000000000000000, -0.000000000000000000, -1.000000000000000000 ) ) ;
#24665 = CARTESIAN_POINT ( 'NONE',  ( -338.8365100919713200, 260.0000000000001137, -191.9749999999917804 ) ) ;
#24667 = CARTESIAN_POINT ( 'NONE',  ( 760.0363995740630116, -58.91815448151690759, -368.7758568127991907 ) ) ;
#24668 = CARTESIAN_POINT ( 'NONE',  ( 779.9999999999992042, -452.9681489794448339, -350.0000000000000000 ) ) ;
#24669 = DIRECTION ( 'NONE',  ( 1.000000000000000000, 0.000000000000000000, 0.000000000000000000 ) ) ;
#24670 = CARTESIAN_POINT ( 'NONE',  ( 793.0897708529556667, -246.5545181178799510, 361.3366627262616362 ) ) ;
#24671 = CARTESIAN_POINT ( 'NONE',  ( 788.7366044899766848, -107.9073299311474727, 316.5762568750059813 ) ) ;
#24672 = VERTEX_POINT ( 'NONE', #18284 ) ;
#24673 = CARTESIAN_POINT ( 'NONE',  ( 755.8894580844503253, -15.82724539060794200, -332.3691319403863531 ) ) ;
#24674 = CARTESIAN_POINT ( 'NONE',  ( 804.7487373415286811, -91.54369356751116982, -364.7487373415288516 ) ) ;
#24675 = CARTESIAN_POINT ( 'NONE',  ( 756.7813123517142913, -283.9874144716867477, 329.9779781133712504 ) ) ;
#24676 = DIRECTION ( 'NONE',  ( -1.000000000000000000, -0.000000000000000000, -0.000000000000000000 ) ) ;
#24677 = VECTOR ( 'NONE', #16121, 1000.000000000000000 ) ;
#24678 = EDGE_CURVE ( 'NONE', #30282, #22122, #32954, .T. ) ;
#24679 = CARTESIAN_POINT ( 'NONE',  ( 755.8990559732751535, -35.46360902697151829, 365.9055244015606831 ) ) ;
#24680 = CARTESIAN_POINT ( 'NONE',  ( 751.6929314249748586, -222.9982390220561399, -318.8095938919659034 ) ) ;
#24681 = AXIS2_PLACEMENT_3D ( 'NONE', #10274, #38008, #30841 ) ;
#24682 = EDGE_CURVE ( 'NONE', #22852, #34024, #18189, .T. ) ;
#24683 = CARTESIAN_POINT ( 'NONE',  ( 804.9363028652555840, -88.27096629478390355, 338.2165204200192079 ) ) ;
#24684 = CARTESIAN_POINT ( 'NONE',  ( -208.8365100919714052, 256.5000000000001137, -193.8809999999926674 ) ) ;
#24685 = CARTESIAN_POINT ( 'NONE',  ( 749.8865473780648472, -260.5328690171413086, -322.1177392798429082 ) ) ;
#24686 = CARTESIAN_POINT ( 'NONE',  ( 797.8822607201568644, -462.5545181178792973, 370.1134526219340160 ) ) ;
#24687 = CARTESIAN_POINT ( 'NONE',  ( 814.9108240113580450, -304.2709662947832499, -337.5031285880265273 ) ) ;
#24688 = FACE_BOUND ( 'NONE', #1872, .T. ) ;
#24689 = CARTESIAN_POINT ( 'NONE',  ( 796.7845633553578182, -345.6237781080501463, 358.5707757039688204 ) ) ;
#24690 = CARTESIAN_POINT ( 'NONE',  ( 804.7487373415286811, -43.54369356751131903, 364.7487373415288516 ) ) ;
#24691 = ADVANCED_FACE ( 'NONE', ( #40427 ), #15927, .F. ) ;
#24692 = CARTESIAN_POINT ( 'NONE',  ( 804.4286716492782716, -377.3618753856920875, -345.3141322388244703 ) ) ;
#24693 = EDGE_CURVE ( 'NONE', #7627, #14468, #20293, .T. ) ;
#24694 = CARTESIAN_POINT ( 'NONE',  ( 755.0488828828309806, -41.80559628986934229, 344.1219089521771934 ) ) ;
#24695 = MECHANICAL_DESIGN_GEOMETRIC_PRESENTATION_REPRESENTATION (  '', ( #43147 ), #15831 ) ;
#24696 = CARTESIAN_POINT ( 'NONE',  ( 813.2346286133761168, -101.2601417444146250, -328.9521613784389160 ) ) ;
#24697 = CARTESIAN_POINT ( 'NONE',  ( 768.8385539511368734, -215.2601417444141987, 306.4236121716840557 ) ) ;
#24698 = CARTESIAN_POINT ( 'NONE',  ( 802.1676090361155502, -14.63460265842049779, 327.8955696845344505 ) ) ;
#24699 = VECTOR ( 'NONE', #23811, 1000.000000000000000 ) ;
#24700 = EDGE_LOOP ( 'NONE', ( #1825, #40416, #26073, #42437 ) ) ;
#24701 = CARTESIAN_POINT ( 'NONE',  ( 766.7756240680305382, -206.5328690171415360, -361.5560724626415663 ) ) ;
#24702 = CARTESIAN_POINT ( 'NONE',  ( 788.8264449731200330, -189.1800572038744122, 363.6646147819171233 ) ) ;
#24703 = CARTESIAN_POINT ( 'NONE',  ( 751.2241431872005251, -40.16923265350570915, -359.9636004259367610 ) ) ;
#24704 = CARTESIAN_POINT ( 'NONE',  ( 762.1405469898973024, -313.5436935675103882, 357.8594530101016176 ) ) ;
#24705 = AXIS2_PLACEMENT_3D ( 'NONE', #30943, #28096, #35257 ) ;
#24706 = LINE ( 'NONE', #7626, #27917 ) ;
#24707 = ORIENTED_EDGE ( 'NONE', *, *, #18664, .F. ) ;
#24708 = CARTESIAN_POINT ( 'NONE',  ( 760.5453621957607311, -45.07832356259660145, 323.8424801807151425 ) ) ;
#24709 = CARTESIAN_POINT ( 'NONE',  ( 811.3240766477731540, -316.3726999360615082, -355.6651683502462902 ) ) ;
#24710 = AXIS2_PLACEMENT_3D ( 'NONE', #24873, #14947, #29270 ) ;
#24711 = ADVANCED_FACE ( 'NONE', ( #5973 ), #9457, .T. ) ;
#24712 = VECTOR ( 'NONE', #2837, 1000.000000000000000 ) ;
#24713 = CARTESIAN_POINT ( 'NONE',  ( 782.5225473063383106, -262.2709662947832499, 375.2698199232970637 ) ) ;
#24714 = CIRCLE ( 'NONE', #7759, 2.749999999999919176 ) ;
#24715 = CARTESIAN_POINT ( 'NONE',  ( 776.2433038121456548, 11.10349461922141145, 374.8207195650711014 ) ) ;
#24716 = CARTESIAN_POINT ( 'NONE',  ( 759.0159684113467620, -160.9181544815165807, -325.8855110935213020 ) ) ;
#24717 = CARTESIAN_POINT ( 'NONE',  ( 805.1927285166397041, -160.8164208402382371, -341.8018195045277707 ) ) ;
#24718 = CARTESIAN_POINT ( 'NONE',  ( 774.6858677611749044, -345.7255117493285184, -315.5713283507209894 ) ) ;
#24719 = VERTEX_POINT ( 'NONE', #12462 ) ;
#24720 = CARTESIAN_POINT ( 'NONE',  ( 745.4481719005789273, -291.7255117493285752, 347.5162901302853129 ) ) ;
#24721 = DIRECTION ( 'NONE',  ( 1.000000000000000000, 0.000000000000000000, 0.000000000000000000 ) ) ;
#24722 = CARTESIAN_POINT ( 'NONE',  ( 760.5453621957607311, -333.0783235625956991, 323.8424801807151425 ) ) ;
#24723 = FACE_OUTER_BOUND ( 'NONE', #8882, .T. ) ;
#24724 = CARTESIAN_POINT ( 'NONE',  ( 776.9254006560222479, -140.1908817542438896, 314.8983024940802125 ) ) ;
#24725 = CARTESIAN_POINT ( 'NONE',  ( 781.8018195045266339, -22.27096629478410250, 365.1927285166406705 ) ) ;
#24726 = ORIENTED_EDGE ( 'NONE', *, *, #3181, .T. ) ;
#24727 = CARTESIAN_POINT ( 'NONE',  ( 805.6418435158337843, -389.4636090269704027, -363.8556311672236916 ) ) ;
#24728 = CIRCLE ( 'NONE', #26941, 2.749999999999835687 ) ;
#24729 = CARTESIAN_POINT ( 'NONE',  ( 811.0346526505617248, -14.63460265842049779, -323.0537975583478101 ) ) ;
#24730 = CARTESIAN_POINT ( 'NONE',  ( 793.0897708529556667, -222.5545181178800362, 361.3366627262616362 ) ) ;
#24731 = CARTESIAN_POINT ( 'NONE',  ( 760.0363995740630116, -250.9181544815163534, 368.7758568127991907 ) ) ;
#24732 = CARTESIAN_POINT ( 'NONE',  ( 765.8855110935204493, -190.1692326535052189, 319.0159684113471599 ) ) ;
#24733 = AXIS2_PLACEMENT_3D ( 'NONE', #1541, #26486, #33411 ) ;
#24734 = CARTESIAN_POINT ( 'NONE',  ( 797.6776695296629214, -379.5436935675102745, -357.6776695296636603 ) ) ;
#24735 = ADVANCED_FACE ( 'NONE', ( #30454 ), #19845, .F. ) ;
#24736 = CARTESIAN_POINT ( 'NONE',  ( 796.1575198192839480, -462.0090635724247932, 359.4546378042384163 ) ) ;
#24737 = DIRECTION ( 'NONE',  ( 1.000000000000000000, 0.000000000000000000, 0.000000000000000000 ) ) ;
#24738 = CARTESIAN_POINT ( 'NONE',  ( 766.9102291470427417, -210.5545181178800647, -318.6633372737382501 ) ) ;
#24739 = AXIS2_PLACEMENT_3D ( 'NONE', #4073, #29009, #35937 ) ;
#24740 = EDGE_CURVE ( 'NONE', #8326, #755, #7128, .T. ) ;
#24741 = CARTESIAN_POINT ( 'NONE',  ( 748.9653473494363425, -2.634602658420536869, 356.9462024416521331 ) ) ;
#24742 = CARTESIAN_POINT ( 'NONE',  ( 999.9999999999992042, 249.9999999999998863, -360.0000000000000000 ) ) ;
#24743 = CARTESIAN_POINT ( 'NONE',  ( 772.4837098697145166, -407.3618753856920307, -374.5518280994205611 ) ) ;
#24744 = DIRECTION ( 'NONE',  ( 1.000000000000000000, 0.000000000000000000, 0.000000000000000000 ) ) ;
#24745 = AXIS2_PLACEMENT_3D ( 'NONE', #42832, #39155, #11656 ) ;
#24746 = CARTESIAN_POINT ( 'NONE',  ( 811.3240766477731540, -364.3726999360614514, 355.6651683502462902 ) ) ;
#24747 = DIRECTION ( 'NONE',  ( 0.000000000000000000, 0.000000000000000000, -1.000000000000000000 ) ) ;
#24748 = CARTESIAN_POINT ( 'NONE',  ( 808.0189434323515343, -326.0891481129649492, 319.0252816721025511 ) ) ;
#24749 = CARTESIAN_POINT ( 'NONE',  ( 745.4481719005789273, -51.72551174932946338, -347.5162901302853129 ) ) ;
#24750 = CARTESIAN_POINT ( 'NONE',  ( 778.2165204200184689, -286.8164208402378677, -364.9363028652563230 ) ) ;
#24751 = VECTOR ( 'NONE', #16553, 1000.000000000000000 ) ;
#24752 = DIRECTION ( 'NONE',  ( -0.000000000000000000, 1.000000000000000000, -0.000000000000000000 ) ) ;
#24753 = CARTESIAN_POINT ( 'NONE',  ( 764.8639956371174549, -416.0891481129645513, 319.7806653035542013 ) ) ;
#24754 = CARTESIAN_POINT ( 'NONE',  ( 802.9823548866075953, -169.0999726633347393, 330.0799878456151077 ) ) ;
#24755 = CARTESIAN_POINT ( 'NONE',  ( 788.6739635108323228, -31.64542720878970883, -373.9316612368139090 ) ) ;
#24756 = CARTESIAN_POINT ( 'NONE',  ( 800.7704444035546203, -76.16923265350557415, -326.0291762391768771 ) ) ;
#24757 = CARTESIAN_POINT ( 'NONE',  ( 745.1769319972822814, -113.8055962898691149, 346.2694204179732083 ) ) ;
#24758 = CARTESIAN_POINT ( 'NONE',  ( 765.0180583372156207, -408.9982390220556567, 360.0135310231089534 ) ) ;
#24759 = DIRECTION ( 'NONE',  ( 8.326672684688676025E-16, 1.000000000000000000, 0.000000000000000000 ) ) ;
#24760 = CARTESIAN_POINT ( 'NONE',  ( 803.4237431249931660, 8.819942796124882634, -331.2633955100225194 ) ) ;
#24761 = ORIENTED_EDGE ( 'NONE', *, *, #15930, .T. ) ;
#24762 = CARTESIAN_POINT ( 'NONE',  ( 755.5713283507202505, -101.3618753856929544, -334.6858677611754729 ) ) ;
#24763 = CARTESIAN_POINT ( 'NONE',  ( 787.6308680596127942, -395.2601417444136587, -364.1105419155492768 ) ) ;
#24765 = CARTESIAN_POINT ( 'NONE',  ( 795.1360043628808398, -212.0891481129653187, 360.2193346964456282 ) ) ;
#24764 = CARTESIAN_POINT ( 'NONE',  ( 754.8072714833581358, -244.8164208402378961, 338.1981804954720587 ) ) ;
#24766 = AXIS2_PLACEMENT_3D ( 'NONE', #18561, #28947, #36780 ) ;
#24767 = CARTESIAN_POINT ( 'NONE',  ( 783.7566961878529810, -384.8965053807772847, -305.1792804349288417 ) ) ;
#24768 = CARTESIAN_POINT ( 'NONE',  ( 759.0252816721024374, -0.9982390220569063999, 368.0189434323527280 ) ) ;
#24769 = LINE ( 'NONE', #25688, #25648 ) ;
#24770 = ORIENTED_EDGE ( 'NONE', *, *, #35122, .F. ) ;
#24771 = CARTESIAN_POINT ( 'NONE',  ( 788.8264449731200330, -429.1800572038737869, 363.6646147819171233 ) ) ;
#24772 = VECTOR ( 'NONE', #9567, 1000.000000000000000 ) ;
#24773 = EDGE_LOOP ( 'NONE', ( #42516, #11216, #3726, #23722, #9788, #1259, #8720, #31880 ) ) ;
#24774 = VECTOR ( 'NONE', #11687, 1000.000000000000000 ) ;
#24775 = CARTESIAN_POINT ( 'NONE',  ( 751.9810565676468741, -242.0891481129652618, -360.9747183278973921 ) ) ;
#24776 = CARTESIAN_POINT ( 'NONE',  ( 814.2001403089898304, -137.3618753856928265, 347.4397851343538264 ) ) ;
#24777 = ORIENTED_EDGE ( 'NONE', *, *, #21050, .T. ) ;
#24778 = CARTESIAN_POINT ( 'NONE',  ( 778.1981804954715471, -250.2709662947833351, -314.8072714833591021 ) ) ;
#24779 = ORIENTED_EDGE ( 'NONE', *, *, #27519, .T. ) ;
#24780 = CARTESIAN_POINT ( 'NONE',  ( 774.6858677611749044, -369.7255117493284615, -315.5713283507209894 ) ) ;
#24781 = CARTESIAN_POINT ( 'NONE',  ( 757.8323909638827445, -26.63460265842045871, -352.1044303154654358 ) ) ;
#24782 = AXIS2_PLACEMENT_3D ( 'NONE', #32784, #11989, #7230 ) ;
#24783 = CARTESIAN_POINT ( 'NONE',  ( 787.6308680596127942, -227.2601417444141987, 364.1105419155492768 ) ) ;
#24784 = DIRECTION ( 'NONE',  ( -1.000000000000000000, 0.000000000000000000, 0.000000000000000000 ) ) ;
#24785 = PLANE ( 'NONE',  #27257 ) ;
#24786 = PRODUCT_DEFINITION_SHAPE ( 'NONE', 'NONE',  #45731 ) ;
#24787 = VERTEX_POINT ( 'NONE', #34139 ) ;
#24788 = CARTESIAN_POINT ( 'NONE',  ( 762.1405469898971887, -1.543693567511449150, -357.8594530101015607 ) ) ;
#24789 = CARTESIAN_POINT ( 'NONE',  ( 939.9999999999993179, -590.0000000000001137, 360.0000000000000000 ) ) ;
#24790 = CARTESIAN_POINT ( 'NONE',  ( 914.9999999999992042, 74.99999999999984368, 360.0000000000000000 ) ) ;
#24791 = VERTEX_POINT ( 'NONE', #23060 ) ;
#24792 = CARTESIAN_POINT ( 'NONE',  ( 791.0478386215596629, -261.8272453906071746, -306.7653713866226326 ) ) ;
#24793 = CARTESIAN_POINT ( 'NONE',  ( 788.6739635108323228, -151.6454272087892718, 373.9316612368139090 ) ) ;
#24795 = CARTESIAN_POINT ( 'NONE',  ( 781.7834795799800531, -250.8164208402379245, -315.0636971347436202 ) ) ;
#24794 = LINE ( 'NONE', #11172, #16515 ) ;
#24796 = CARTESIAN_POINT ( 'NONE',  ( 789.9200121543843807, -409.9874144716863498, -317.0176451133914384 ) ) ;
#24797 = CARTESIAN_POINT ( 'NONE',  ( 794.9999999999993179, -365.3551492539851893, 8.132432514707076621 ) ) ;
#24798 = CARTESIAN_POINT ( 'NONE',  ( 804.1105419155481968, -123.8272453906076009, -347.6308680596136469 ) ) ;
#24799 = CARTESIAN_POINT ( 'NONE',  ( 813.5763878283155464, -387.8272453906067767, 351.1614460488615350 ) ) ;
#24800 = CARTESIAN_POINT ( 'NONE',  ( 799.9999999999993179, -512.9681489794448908, -329.9999999999999432 ) ) ;
#24801 = CARTESIAN_POINT ( 'NONE',  ( 778.7502325331095108, -0.3510508353240099355, -304.6391490659818828 ) ) ;
#24802 = CARTESIAN_POINT ( 'NONE',  ( 814.5518280994195948, -327.7255117493285752, -332.4837098697145166 ) ) ;
#24803 = CARTESIAN_POINT ( 'NONE',  ( 755.5713283507202505, -5.361875385693257279, 334.6858677611754729 ) ) ;
#24804 = CARTESIAN_POINT ( 'NONE',  ( 791.9812246680005501, -68.63460265842033436, -361.9419747391813189 ) ) ;
#24805 = CARTESIAN_POINT ( 'NONE',  ( 802.2119215644370342, -246.0090635724253900, 367.5423716828165084 ) ) ;
#24806 = CARTESIAN_POINT ( 'NONE',  ( 812.6845335610512393, -199.9874144716870603, -353.5525998758768651 ) ) ;
#24807 = CARTESIAN_POINT ( 'NONE',  ( 745.0891759886404770, -220.2709662947834772, 342.4968714119734159 ) ) ;
#24808 = CARTESIAN_POINT ( 'NONE',  ( 810.7187646348534145, -450.4527844766009821, -356.7737145352016341 ) ) ;
#24809 = VECTOR ( 'NONE', #1702, 1000.000000000000000 ) ;
#24810 = DIRECTION ( 'NONE',  ( -0.000000000000000000, 1.000000000000000000, -0.000000000000000000 ) ) ;
#24811 = CARTESIAN_POINT ( 'NONE',  ( 771.2633955100217236, -287.9073299311468759, 363.4237431249939618 ) ) ;
#24812 = CARTESIAN_POINT ( 'NONE',  ( 787.5531968255692163, -93.82724539060770041, 316.1348686366205811 ) ) ;
#24813 = CARTESIAN_POINT ( 'NONE',  ( 759.2295555964440155, 7.830767346494148740, -353.9708237608231229 ) ) ;
#24814 = CARTESIAN_POINT ( 'NONE',  ( 1820.038553321469863, 47.45399382421944523, 201.9999999999999432 ) ) ;
#24815 = LINE ( 'NONE', #32670, #35066 ) ;
#24817 = CARTESIAN_POINT ( 'NONE',  ( 803.6646147819161570, -377.9073299311466485, 348.8264449731210561 ) ) ;
#24816 = CARTESIAN_POINT ( 'NONE',  ( 770.0799878456142551, -133.9874144716872024, 362.9823548866085616 ) ) ;
#24818 = ORIENTED_EDGE ( 'NONE', *, *, #21570, .F. ) ;
#24819 = AXIS2_PLACEMENT_3D ( 'NONE', #45024, #34835, #41548 ) ;
#24820 = CARTESIAN_POINT ( 'NONE',  ( 764.0069404352550464, -303.0783235625957559, -359.2566176426627180 ) ) ;
#24821 = CARTESIAN_POINT ( 'NONE',  ( 794.9819416627830151, -108.9982390220565804, 319.9864689768909898 ) ) ;
#24822 = CARTESIAN_POINT ( 'NONE',  ( 812.6845335610512393, -295.9874144716866908, -353.5525998758768651 ) ) ;
#24823 = DIRECTION ( 'NONE',  ( 0.000000000000000000, 0.000000000000000000, -1.000000000000000000 ) ) ;
#24824 = CARTESIAN_POINT ( 'NONE',  ( 764.3348316497523456, -406.7146871989590409, 308.6759233522265617 ) ) ;
#24825 = VERTEX_POINT ( 'NONE', #37402 ) ;
#24826 = CARTESIAN_POINT ( 'NONE',  ( 804.6798772138708955, -327.7255117493285184, 334.6312213355107019 ) ) ;
#24827 = CARTESIAN_POINT ( 'NONE',  ( 760.5453621957607311, -45.07832356259660145, -323.8424801807151425 ) ) ;
#24828 = CARTESIAN_POINT ( 'NONE',  ( 778.1981804954714335, -154.2709662947836478, -314.8072714833589885 ) ) ;
#24829 = CARTESIAN_POINT ( 'NONE',  ( 754.8072714833581358, -196.8164208402380950, -338.1981804954720587 ) ) ;
#24830 = CARTESIAN_POINT ( 'NONE',  ( 755.5713283507202505, -413.3618753856920307, 334.6858677611754729 ) ) ;
#24831 = CARTESIAN_POINT ( 'NONE',  ( 749.2812353651451076, -150.4527844766018916, -323.2262854647983090 ) ) ;
#24832 = ORIENTED_EDGE ( 'NONE', *, *, #40181, .F. ) ;
#24833 = CARTESIAN_POINT ( 'NONE',  ( 805.1927285166399315, -136.8164208402382656, -341.8018195045277707 ) ) ;
#24834 = ORIENTED_EDGE ( 'NONE', *, *, #13339, .T. ) ;
#24835 = AXIS2_PLACEMENT_3D ( 'NONE', #19676, #34202, #9736 ) ;
#24836 = CARTESIAN_POINT ( 'NONE',  ( 761.4292242960306112, -401.4636090269704027, -323.2154366446414429 ) ) ;
#24837 = CARTESIAN_POINT ( 'NONE',  ( 802.5472867521000353, -436.3726999360612240, 350.8726784830461156 ) ) ;
#24838 = CARTESIAN_POINT ( 'NONE',  ( 765.8855110935204493, -118.1692326535054463, 319.0159684113471599 ) ) ;
#24839 = VECTOR ( 'NONE', #19615, 1000.000000000000000 ) ;
#24842 = CARTESIAN_POINT ( 'NONE',  ( 768.8385539511368734, -383.2601417444137155, 306.4236121716840557 ) ) ;
#24841 = DIRECTION ( 'NONE',  ( -0.000000000000000000, -0.000000000000000000, 1.000000000000000000 ) ) ;
#24840 = DIRECTION ( 'NONE',  ( 0.000000000000000000, -1.000000000000000000, -1.110223024625155554E-15 ) ) ;
#24843 = ORIENTED_EDGE ( 'NONE', *, *, #6551, .F. ) ;
#24844 = CARTESIAN_POINT ( 'NONE',  ( 769.0155153010367712, -394.3726999360613377, -362.7791456095907279 ) ) ;
#24845 = CARTESIAN_POINT ( 'NONE',  ( 768.0187753319979720, -368.6346026584193964, -318.0580252608186242 ) ) ;
#24846 = CARTESIAN_POINT ( 'NONE',  ( 747.6481478633932056, -157.0999726633347962, -353.4146539503763620 ) ) ;
#24847 = CARTESIAN_POINT ( 'NONE',  ( 766.4474001241216001, -19.09997266333520116, 307.3154664389482491 ) ) ;
#24848 = CIRCLE ( 'NONE', #34183, 6.118999999999985562 ) ;
#24850 = LINE ( 'NONE', #45664, #22528 ) ;
#24849 = FACE_OUTER_BOUND ( 'NONE', #39629, .T. ) ;
#24851 = CARTESIAN_POINT ( 'NONE',  ( 796.7845633553578182, -297.6237781080502600, -358.5707757039688204 ) ) ;
#24852 = DIRECTION ( 'NONE',  ( -1.000000000000000000, -0.000000000000000000, 0.000000000000000000 ) ) ;
#24853 = CARTESIAN_POINT ( 'NONE',  ( 768.9521613784389729, -201.8272453906073451, -373.2346286133773106 ) ) ;
#24854 = DIRECTION ( 'NONE',  ( -1.000000000000000000, -0.000000000000000000, -0.000000000000000000 ) ) ;
#24855 = DIRECTION ( 'NONE',  ( -0.000000000000000000, 1.000000000000000000, -0.000000000000000000 ) ) ;
#24856 = AXIS2_PLACEMENT_3D ( 'NONE', #39712, #7832, #18450 ) ;
#24857 = CARTESIAN_POINT ( 'NONE',  ( 773.4516893846965786, -355.6454272087887603, 315.8398074228977066 ) ) ;
#24858 = CARTESIAN_POINT ( 'NONE',  ( 752.7379699480933368, -348.0090635724251342, 361.9858362298580232 ) ) ;
#24859 = CARTESIAN_POINT ( 'NONE',  ( 763.0537975583476964, -192.4527844766017211, -371.0346526505628617 ) ) ;
#24860 = CARTESIAN_POINT ( 'NONE',  ( -786.4999999999993179, -512.9681489794448908, -339.9999999999999432 ) ) ;
#24861 = CARTESIAN_POINT ( 'NONE',  ( 800.0135310231082713, 9.910851887033969021, -325.0180583372163028 ) ) ;
#24862 = CARTESIAN_POINT ( 'NONE',  ( 750.9282345327678740, -160.9181544815165807, 319.8311093483690115 ) ) ;
#24863 = CARTESIAN_POINT ( 'NONE',  ( 744.8212110874229666, -114.8965053807782226, -336.2046728542121627 ) ) ;
#24864 = CARTESIAN_POINT ( 'NONE',  ( 777.4774526936600978, -106.2709662947838467, 304.7301800767027657 ) ) ;
#24865 = CARTESIAN_POINT ( 'NONE',  ( 815.2698199232961542, -352.8164208402374129, -342.5225473063383106 ) ) ;
#24866 = DIRECTION ( 'NONE',  ( -0.000000000000000000, 1.000000000000000000, -0.000000000000000000 ) ) ;
#24867 = FACE_OUTER_BOUND ( 'NONE', #40369, .T. ) ;
#24868 = CARTESIAN_POINT ( 'NONE',  ( 771.2633955100217236, -167.9073299311473022, 363.4237431249939618 ) ) ;
#24869 = CARTESIAN_POINT ( 'NONE',  ( 787.5531968255692163, 2.172754609392001601, 316.1348686366205811 ) ) ;
#24870 = CARTESIAN_POINT ( 'NONE',  ( 746.0683387631852383, -403.4419599262317888, -331.3260364891676204 ) ) ;
#24871 = AXIS2_PLACEMENT_3D ( 'NONE', #18678, #44452, #37293 ) ;
#24872 = CARTESIAN_POINT ( 'NONE',  ( 745.4481719005789273, -411.7255117493282910, -347.5162901302853129 ) ) ;
#24873 = CARTESIAN_POINT ( 'NONE',  ( -338.8365100919713200, 260.0000000000001137, -199.9999999999917861 ) ) ;
#24874 = CARTESIAN_POINT ( 'NONE',  ( 800.1688906516307043, -10.16923265350579442, 369.0717654672308186 ) ) ;
#24875 = ORIENTED_EDGE ( 'NONE', *, *, #11726, .T. ) ;
#24876 = VECTOR ( 'NONE', #30650, 1000.000000000000000 ) ;
#24877 = CARTESIAN_POINT ( 'NONE',  ( 786.2056067578752163, -179.8055962898688733, -374.4686193811670023 ) ) ;
#24878 = DIRECTION ( 'NONE',  ( 1.000000000000000000, 0.000000000000000000, 0.000000000000000000 ) ) ;
#24879 = CARTESIAN_POINT ( 'NONE',  ( 771.2368401574024119, -325.4419599262320162, 374.2805881961240857 ) ) ;
#24880 = CARTESIAN_POINT ( 'NONE',  ( 804.9363028652555840, -136.2709662947837330, 338.2165204200192079 ) ) ;
#24881 = VERTEX_POINT ( 'NONE', #41326 ) ;
#24882 = AXIS2_PLACEMENT_3D ( 'NONE', #27603, #20668, #34759 ) ;
#24883 = CARTESIAN_POINT ( 'NONE',  ( 795.1360043628807261, -308.0891481129650629, 360.2193346964456282 ) ) ;
#24884 = CARTESIAN_POINT ( 'NONE',  ( 796.9462024416508257, -36.45278447660223975, -308.9653473494370246 ) ) ;
#24885 = CARTESIAN_POINT ( 'NONE',  ( 796.7737145352015204, -92.63460265842026331, 370.7187646348536987 ) ) ;
#24886 = EDGE_LOOP ( 'NONE', ( #43134, #45083, #43472, #37265 ) ) ;
#24887 = CARTESIAN_POINT ( 'NONE',  ( 773.7305795820266212, -441.2817908451521021, -374.8230680027170365 ) ) ;
#24888 = EDGE_LOOP ( 'NONE', ( #1640, #6553, #7564, #30756 ) ) ;
#24889 = PRODUCT_CONTEXT ( 'NONE', #34917, 'mechanical' ) ;
#24890 = CARTESIAN_POINT ( 'NONE',  ( 754.8072714833581358, -28.81642084023863148, 338.1981804954720587 ) ) ;
#24891 = CARTESIAN_POINT ( 'NONE',  ( 803.6646147819161570, -281.9073299311468759, -348.8264449731210561 ) ) ;
#24893 = CARTESIAN_POINT ( 'NONE',  ( 795.6651683502461765, -298.7146871989593251, 371.3240766477733814 ) ) ;
#24892 = CARTESIAN_POINT ( 'NONE',  ( 814.2001403089898304, -401.3618753856920307, 347.4397851343538264 ) ) ;
#24894 = CARTESIAN_POINT ( 'NONE',  ( 771.2368401574024119, -85.44195992623282621, 374.2805881961240857 ) ) ;
#24895 = CARTESIAN_POINT ( 'NONE',  ( 759.0159684113467620, -280.9181544815162965, -325.8855110935213020 ) ) ;
#24896 = CARTESIAN_POINT ( 'NONE',  ( 778.1981804954714335, -250.2709662947832783, -314.8072714833589885 ) ) ;
#24897 = CARTESIAN_POINT ( 'NONE',  ( 781.7834795799800531, -442.8164208402372992, -315.0636971347436202 ) ) ;
#24898 = CARTESIAN_POINT ( 'NONE',  ( 795.1360043628807261, -116.0891481129656029, -360.2193346964456282 ) ) ;
#24899 = CARTESIAN_POINT ( 'NONE',  ( -208.8365100919714052, 256.5000000000001137, -199.9999999999926956 ) ) ;
#24900 = CARTESIAN_POINT ( 'NONE',  ( 814.5518280994195948, -375.7255117493283478, 332.4837098697145734 ) ) ;
#24902 = PLANE ( 'NONE',  #42565 ) ;
#24901 = CARTESIAN_POINT ( 'NONE',  ( -786.4999999999993179, -512.9681489794448908, -339.9999999999999432 ) ) ;
#24903 = CARTESIAN_POINT ( 'NONE',  ( 764.1737431748507561, -58.37269993606236085, -371.6461892240376415 ) ) ;
#24904 = DIRECTION ( 'NONE',  ( 1.000000000000000000, 0.000000000000000000, -0.000000000000000000 ) ) ;
#24905 = CARTESIAN_POINT ( 'NONE',  ( 914.9999999999992042, 74.99999999999984368, 360.0000000000000000 ) ) ;
#24906 = EDGE_CURVE ( 'NONE', #23907, #56, #2509, .T. ) ;
#24907 = CARTESIAN_POINT ( 'NONE',  ( 802.9823548866075953, -265.0999726633344267, 330.0799878456151077 ) ) ;
#24908 = CARTESIAN_POINT ( 'NONE',  ( 759.7806653035534055, -126.9982390220565094, 324.8639956371180801 ) ) ;
#24909 = EDGE_LOOP ( 'NONE', ( #22927, #29885, #43919, #27343 ) ) ;
#24910 = CARTESIAN_POINT ( 'NONE',  ( 775.8780910478218402, -9.281790845153418346, -364.9511171171680530 ) ) ;
#24911 = CARTESIAN_POINT ( 'NONE',  ( 745.7998596910086917, -101.3618753856929544, -332.5602148656461168 ) ) ;
#24912 = CARTESIAN_POINT ( 'NONE',  ( 800.7704444035546203, -292.1692326535048210, 326.0291762391768771 ) ) ;
#24913 = AXIS2_PLACEMENT_3D ( 'NONE', #14852, #18325, #43239 ) ;
#24914 = FACE_OUTER_BOUND ( 'NONE', #28343, .T. ) ;
#24915 = CARTESIAN_POINT ( 'NONE',  ( 744.6391490659812007, -38.73633629969877035, 338.7502325331110455 ) ) ;
#24916 = CARTESIAN_POINT ( 'NONE',  ( 772.5602148656447525, -225.7255117493289163, -305.7998596910095443 ) ) ;
#24917 = CARTESIAN_POINT ( 'NONE',  ( 796.9462024416508257, -180.4527844766017211, 308.9653473494370246 ) ) ;
#24918 = CARTESIAN_POINT ( 'NONE',  ( 804.6798772138708955, -87.72551174932937101, 334.6312213355107019 ) ) ;
#24919 = CYLINDRICAL_SURFACE ( 'NONE', #26220, 7.999999999999896083 ) ;
#24920 = CARTESIAN_POINT ( 'NONE',  ( 759.8311093483677041, -310.1692326535048778, -310.9282345327691814 ) ) ;
#24921 = CARTESIAN_POINT ( 'NONE',  ( 797.8822607201568644, -438.5545181178793541, 370.1134526219340160 ) ) ;
#24922 = CARTESIAN_POINT ( 'NONE',  ( 748.9653473494363425, -314.6346026584194533, -356.9462024416521331 ) ) ;
#24923 = DIRECTION ( 'NONE',  ( 1.000000000000000000, -0.000000000000000000, -0.000000000000000000 ) ) ;
#24924 = CARTESIAN_POINT ( 'NONE',  ( 795.9930595647434757, -363.0783235625955854, 320.7433823573372820 ) ) ;
#24925 = CARTESIAN_POINT ( 'NONE',  ( 767.6429770376291799, -57.18005720387490243, 306.8695393053162093 ) ) ;
#24926 = CARTESIAN_POINT ( 'NONE',  ( 801.9419747391806368, -402.4527844766010389, -351.9812246680014027 ) ) ;
#24927 = CARTESIAN_POINT ( 'NONE',  ( 773.3843516231979720, -61.44195992623291147, 364.4086373105754433 ) ) ;
#24928 = CARTESIAN_POINT ( 'NONE',  ( 762.3223304703356007, -199.5436935675108430, -322.3223304703362828 ) ) ;
#24929 = CARTESIAN_POINT ( 'NONE',  ( 752.4576283171824116, -93.07832356259645223, -317.7880784355627952 ) ) ;
#24930 = CARTESIAN_POINT ( 'NONE',  ( 808.7758568127978833, -220.1692326535051052, 320.0363995740631822 ) ) ;
#24931 = CARTESIAN_POINT ( 'NONE',  ( 764.8639956371174549, -32.08914811296589420, 319.7806653035542581 ) ) ;
#24932 = ORIENTED_EDGE ( 'NONE', *, *, #11519, .F. ) ;
#24933 = CARTESIAN_POINT ( 'NONE',  ( 754.9735926884551418, -210.3510508353233490, -340.5236548041000333 ) ) ;
#24934 = CARTESIAN_POINT ( 'NONE',  ( 756.3353852180819104, -197.9073299311472169, 331.1735550268788302 ) ) ;
#24935 = CARTESIAN_POINT ( 'NONE',  ( 761.9338519418445230, -38.53286901714206891, -370.4231160770881957 ) ) ;
#24936 = CARTESIAN_POINT ( 'NONE',  ( 768.0187753319979720, -344.6346026584195101, 318.0580252608186242 ) ) ;
#24937 = DIRECTION ( 'NONE',  ( 1.000000000000000000, 1.644774851296528363E-16, -0.000000000000000000 ) ) ;
#24938 = LINE ( 'NONE', #11091, #41174 ) ;
#24939 = ORIENTED_EDGE ( 'NONE', *, *, #7143, .T. ) ;
#24940 = CARTESIAN_POINT ( 'NONE',  ( 770.0799878456142551, -61.98741447168745822, 362.9823548866085616 ) ) ;
#24941 = CARTESIAN_POINT ( 'NONE',  ( 807.2620300519052989, -360.0090635724250774, -318.0141637701419768 ) ) ;
#24942 = AXIS2_PLACEMENT_3D ( 'NONE', #30664, #17499, #31577 ) ;
#24943 = CARTESIAN_POINT ( 'NONE',  ( 749.2812353651451076, -246.4527844766016074, 323.2262854647983090 ) ) ;
#24944 = EDGE_CURVE ( 'NONE', #17118, #32232, #23299, .T. ) ;
#24945 = CARTESIAN_POINT ( 'NONE',  ( 791.1614460488616487, 12.73985825558503926, 373.5763878283158874 ) ) ;
#24946 = CARTESIAN_POINT ( 'NONE',  ( 755.5913626894240451, -133.6454272087893571, -346.6156483768012890 ) ) ;
#24947 = CARTESIAN_POINT ( 'NONE',  ( 792.1044303154645831, -132.4527844766018916, -317.8323909638837677 ) ) ;
#24948 = CARTESIAN_POINT ( 'NONE',  ( 756.5762568750052424, -339.1800572038740142, -348.7366044899774238 ) ) ;
#24949 = ORIENTED_EDGE ( 'NONE', *, *, #23560, .F. ) ;
#24950 = CARTESIAN_POINT ( 'NONE',  ( 804.9363028652555840, -448.2709662947827951, -338.2165204200192079 ) ) ;
#24951 = CARTESIAN_POINT ( 'NONE',  ( 763.2262854647970016, -272.6346026584196807, 309.2812353651462445 ) ) ;
#24952 = DIRECTION ( 'NONE',  ( 0.000000000000000000, 0.000000000000000000, 1.000000000000000000 ) ) ;
#24953 = CARTESIAN_POINT ( 'NONE',  ( 787.6308680596127942, -347.2601417444138860, 364.1105419155492768 ) ) ;
#24954 = CARTESIAN_POINT ( 'NONE',  ( 829.9999999999992042, 579.9999999999998863, -360.0000000000000000 ) ) ;
#24955 = EDGE_CURVE ( 'NONE', #1029, #37198, #21864, .T. ) ;
#24956 = CARTESIAN_POINT ( 'NONE',  ( 784.1219089521767955, -165.2817908451529547, 315.0488828828318333 ) ) ;
#24957 = CARTESIAN_POINT ( 'NONE',  ( 756.5762568750052424, -27.18005720387500901, 348.7366044899774238 ) ) ;
#24958 = ORIENTED_EDGE ( 'NONE', *, *, #8906, .T. ) ;
#24959 = CARTESIAN_POINT ( 'NONE',  ( 746.4236121716829757, -375.8272453906069472, -328.8385539511384650 ) ) ;
#24960 = CARTESIAN_POINT ( 'NONE',  ( 801.1904061080338124, 3.910851887033986785, -368.3070685750236066 ) ) ;
#24961 = CARTESIAN_POINT ( 'NONE',  ( 755.5913626894240451, -229.6454272087890729, 346.6156483768012890 ) ) ;
#24962 = CARTESIAN_POINT ( 'NONE',  ( 783.7953271457878373, -272.1908817542434917, 375.1787889125761239 ) ) ;
#24963 = CARTESIAN_POINT ( 'NONE',  ( 793.2243759319678702, -170.5328690171416781, 318.4439275373583200 ) ) ;
#24964 = CARTESIAN_POINT ( 'NONE',  ( 788.8264449731200330, -357.1800572038739006, -363.6646147819171233 ) ) ;
#24965 = CARTESIAN_POINT ( 'NONE',  ( 785.3141322388236176, 2.274488250670355871, 364.4286716492789537 ) ) ;
#24966 = DIRECTION ( 'NONE',  ( 1.000000000000000000, -0.000000000000000000, -0.000000000000000000 ) ) ;
#24967 = CARTESIAN_POINT ( 'NONE',  ( 763.8424801807145741, -210.0090635724255321, -320.5453621957614700 ) ) ;
#24968 = CARTESIAN_POINT ( 'NONE',  ( 796.7737145352015204, -20.63460265842048003, 370.7187646348536987 ) ) ;
#24969 = CARTESIAN_POINT ( 'NONE',  ( 804.7487373415286811, -67.54369356751125508, 364.7487373415288516 ) ) ;
#24970 = DIRECTION ( 'NONE',  ( 0.000000000000000000, 0.000000000000000000, -1.000000000000000000 ) ) ;
#24971 = CARTESIAN_POINT ( 'NONE',  ( 787.4397851343537695, -429.7255117493282910, -374.2001403089903988 ) ) ;
#24972 = EDGE_CURVE ( 'NONE', #35503, #41096, #813, .T. ) ;
#24973 = CIRCLE ( 'NONE', #9490, 10.00000000000000888 ) ;
#24974 = CARTESIAN_POINT ( 'NONE',  ( 768.9521613784389729, -369.8272453906068904, 373.2346286133773106 ) ) ;
#24975 = EDGE_CURVE ( 'NONE', #36456, #5823, #22847, .T. ) ;
#24976 = DIRECTION ( 'NONE',  ( -1.880165489482579047E-16, -1.000000000000000000, -0.000000000000000000 ) ) ;
#24977 = CARTESIAN_POINT ( 'NONE',  ( 745.4481719005789273, -339.7255117493285184, 347.5162901302853129 ) ) ;
#24978 = CARTESIAN_POINT ( 'NONE',  ( 815.2698199232961542, -64.81642084023852135, -342.5225473063383106 ) ) ;
#24979 = CARTESIAN_POINT ( 'NONE',  ( 803.4237431249931660, -279.1800572038741848, -331.2633955100225194 ) ) ;
#24980 = CARTESIAN_POINT ( 'NONE',  ( -728.8365100919714905, 256.5000000000001705, -199.9999999999890861 ) ) ;
#24981 = CARTESIAN_POINT ( 'NONE',  ( 755.5713283507202505, -437.3618753856919170, 334.6858677611754729 ) ) ;
#24982 = EDGE_CURVE ( 'NONE', #19525, #8509, #29268, .T. ) ;
#24983 = CARTESIAN_POINT ( 'NONE',  ( 763.0428371773158460, -179.4636090269710849, 358.7617431975195359 ) ) ;
#24984 = CARTESIAN_POINT ( 'NONE',  ( 793.5525998758768083, -55.09997266333508747, -372.6845335610516941 ) ) ;
#24985 = CARTESIAN_POINT ( 'NONE',  ( 803.2186876482843445, -79.98741447168740137, -350.0220218866286928 ) ) ;
#24986 = CARTESIAN_POINT ( 'NONE',  ( 805.9055244015594326, -99.62377810805098477, 315.8990559732753240 ) ) ;
#24987 = CARTESIAN_POINT ( 'NONE',  ( 762.3223304703356007, -391.5436935675101608, 322.3223304703362828 ) ) ;
#24988 = CARTESIAN_POINT ( 'NONE',  ( 814.8230680027162407, -149.8055962898689870, 333.7305795820267917 ) ) ;
#24989 = CARTESIAN_POINT ( 'NONE',  ( 797.8594530101008786, 10.45630643248850866, -322.1405469898980982 ) ) ;
#24990 = VERTEX_POINT ( 'NONE', #9676 ) ;
#24991 = CARTESIAN_POINT ( 'NONE',  ( 765.0180583372156207, -96.99823902205660886, -360.0135310231089534 ) ) ;
#24992 = CARTESIAN_POINT ( 'NONE',  ( 805.0264073115434940, -390.3510508353227237, -339.4763451958999099 ) ) ;
#24994 = CARTESIAN_POINT ( 'NONE',  ( 778.2165204200184689, -238.8164208402379813, 364.9363028652563230 ) ) ;
#24993 = CARTESIAN_POINT ( 'NONE',  ( 797.8594530101008786, -229.5436935675106440, 322.1405469898980982 ) ) ;
#24995 = ORIENTED_EDGE ( 'NONE', *, *, #35398, .T. ) ;
#24996 = CARTESIAN_POINT ( 'NONE',  ( 814.8230680027162407, -413.8055962898681059, -333.7305795820267917 ) ) ;
#24997 = DIRECTION ( 'NONE',  ( -0.000000000000000000, -0.000000000000000000, -1.000000000000000000 ) ) ;
#24998 = ORIENTED_EDGE ( 'NONE', *, *, #11465, .F. ) ;
#24999 = CARTESIAN_POINT ( 'NONE',  ( 785.3687786644884454, -419.3618753856918033, 315.3201227861279676 ) ) ;
#25000 = EDGE_CURVE ( 'NONE', #10586, #23226, #23741, .T. ) ;
#25001 = ORIENTED_EDGE ( 'NONE', *, *, #43293, .F. ) ;
#25002 = CARTESIAN_POINT ( 'NONE',  ( 777.5031285880264704, -262.8164208402379245, -374.9108240113588408 ) ) ;
#25003 = CARTESIAN_POINT ( 'NONE',  ( 777.4774526936600978, -154.2709662947836762, 304.7301800767028226 ) ) ;
#25004 = EDGE_CURVE ( 'NONE', #15202, #10227, #23519, .T. ) ;
#25005 = CARTESIAN_POINT ( 'NONE',  ( 763.8424801807145741, -282.0090635724253048, 320.5453621957614700 ) ) ;
#25006 = EDGE_LOOP ( 'NONE', ( #35962, #10457, #42737, #14816 ) ) ;
#25007 = CARTESIAN_POINT ( 'NONE',  ( 786.5483106153019435, -31.64542720878970883, -364.1601925771022366 ) ) ;
#25008 = CARTESIAN_POINT ( 'NONE',  ( 808.7758568127978833, -196.1692326535052473, 320.0363995740631822 ) ) ;
#25009 = CARTESIAN_POINT ( 'NONE',  ( 797.6776695296629214, -259.5436935675106156, -357.6776695296636603 ) ) ;
#25010 = ORIENTED_EDGE ( 'NONE', *, *, #2909, .F. ) ;
#25011 = VECTOR ( 'NONE', #20548, 1000.000000000000000 ) ;
#25012 = CARTESIAN_POINT ( 'NONE',  ( 764.8639956371174549, -368.0891481129647786, -319.7806653035542013 ) ) ;
#25013 = CARTESIAN_POINT ( 'NONE',  ( 759.9864689768902508, -2.089148112965993231, -354.9819416627836404 ) ) ;
#25014 = CARTESIAN_POINT ( 'NONE',  ( 760.5453621957607311, -237.0783235625960117, 323.8424801807151425 ) ) ;
#25015 = ADVANCED_FACE ( 'NONE', ( #34385 ), #40865, .F. ) ;
#25016 = FACE_OUTER_BOUND ( 'NONE', #4459, .T. ) ;
#25017 = CARTESIAN_POINT ( 'NONE',  ( -809.9999999999993179, -512.9681489794448908, -339.9999999999999432 ) ) ;
#25018 = VERTEX_POINT ( 'NONE', #42014 ) ;
#25019 = CARTESIAN_POINT ( 'NONE',  ( 774.6858677611749044, -33.72551174932952733, -315.5713283507209894 ) ) ;
#25020 = DIRECTION ( 'NONE',  ( -0.000000000000000000, -0.000000000000000000, 1.000000000000000000 ) ) ;
#25021 = CARTESIAN_POINT ( 'NONE',  ( -728.8365100919714905, 258.0940000000001646, -199.9999999999890861 ) ) ;
#25022 = ORIENTED_EDGE ( 'NONE', *, *, #6020, .T. ) ;
#25023 = CARTESIAN_POINT ( 'NONE',  ( 776.2046728542105711, -260.1908817542435486, -304.8212110874238761 ) ) ;
#25024 = CARTESIAN_POINT ( 'NONE',  ( 814.2805881961230625, -145.6454272087893287, 331.2368401574024119 ) ) ;
#25026 = CARTESIAN_POINT ( 'NONE',  ( 759.9864689768902508, -266.0891481129651197, -354.9819416627836404 ) ) ;
#25025 = LINE ( 'NONE', #21335, #35695 ) ;
#25027 = CARTESIAN_POINT ( 'NONE',  ( 802.5472867521000353, -124.3726999360621619, -350.8726784830461156 ) ) ;
#25028 = CARTESIAN_POINT ( 'NONE',  ( 754.3581564841646241, -377.4636090269704596, 316.1443688327762516 ) ) ;
#25029 = LINE ( 'NONE', #18117, #34252 ) ;
#25030 = CARTESIAN_POINT ( 'NONE',  ( 808.7758568127978833, 19.83076734649410966, -320.0363995740631822 ) ) ;
#25031 = CARTESIAN_POINT ( 'NONE',  ( 782.4968714119720516, -322.8164208402377540, -305.0891759886411023 ) ) ;
#25032 = DIRECTION ( 'NONE',  ( 1.000000000000000000, -0.000000000000000000, 0.000000000000000000 ) ) ;
#25033 = CARTESIAN_POINT ( 'NONE',  ( 778.1981804954714335, -10.27096629478414691, 314.8072714833589885 ) ) ;
#25034 = CARTESIAN_POINT ( 'NONE',  ( 791.0478386215596629, -237.8272453906072599, 306.7653713866226326 ) ) ;
#25035 = CARTESIAN_POINT ( 'NONE',  ( 744.9990715423526808, -186.3510508353234343, -341.2370466360926002 ) ) ;
#25036 = CARTESIAN_POINT ( 'NONE',  ( 812.7932403749906598, -231.1800572038743553, 327.7687537140311633 ) ) ;
#25037 = CARTESIAN_POINT ( 'NONE',  ( 772.4837098697144029, -431.3618753856918033, -374.5518280994205611 ) ) ;
#25038 = LINE ( 'NONE', #14194, #23185 ) ;
#25039 = CARTESIAN_POINT ( 'NONE',  ( 778.2165204200184689, -310.8164208402377540, 364.9363028652563230 ) ) ;
#25040 = CARTESIAN_POINT ( 'NONE',  ( 755.1538015810308480, -86.19088175424408860, 343.0433043558613804 ) ) ;
#25041 = CARTESIAN_POINT ( 'NONE',  ( 772.4468031744293057, -81.82724539060772884, 363.8651313633793620 ) ) ;
#25042 = CARTESIAN_POINT ( 'NONE',  ( 804.4286716492782716, -449.3618753856918602, -345.3141322388244703 ) ) ;
#25043 = CIRCLE ( 'NONE', #44969, 10.00000000000000888 ) ;
#25044 = CARTESIAN_POINT ( 'NONE',  ( 769.9999999999992042, 205.0000000000000568, -329.9999999999999432 ) ) ;
#25045 = DIRECTION ( 'NONE',  ( -0.000000000000000000, -0.000000000000000000, 1.000000000000000000 ) ) ;
#25047 = CARTESIAN_POINT ( 'NONE',  ( 774.6312213355099630, -359.3618753856920875, 364.6798772138717482 ) ) ;
#25046 = CARTESIAN_POINT ( 'NONE',  ( 798.7617431975189675, -147.6237781080508285, 323.0428371773161871 ) ) ;
#25048 = EDGE_LOOP ( 'NONE', ( #44978, #2797 ) ) ;
#25049 = CARTESIAN_POINT ( 'NONE',  ( 757.2208543904082489, -280.7146871989594956, -350.9844846989624330 ) ) ;
#25050 = CARTESIAN_POINT ( 'NONE',  ( 804.9363028652555840, -136.2709662947837330, 338.2165204200192079 ) ) ;
#25051 = CARTESIAN_POINT ( 'NONE',  ( 752.4576283171824116, -309.0783235625957559, -317.7880784355627952 ) ) ;
#25052 = CARTESIAN_POINT ( 'NONE',  ( -598.8365100919716042, 258.0940000000001646, -199.9999999999899671 ) ) ;
#25053 = CARTESIAN_POINT ( 'NONE',  ( 756.1443688327750579, -405.6237781080500326, 314.3581564841659315 ) ) ;
#25054 = ORIENTED_EDGE ( 'NONE', *, *, #4027, .T. ) ;
#25055 = CARTESIAN_POINT ( 'NONE',  ( 800.0135310231082713, -326.0891481129649492, 325.0180583372163028 ) ) ;
#25056 = CARTESIAN_POINT ( 'NONE',  ( 755.0488828828309806, -89.80559628986918597, -344.1219089521771934 ) ) ;
#25057 = CARTESIAN_POINT ( 'NONE',  ( 757.8323909638827445, -146.6346026584200217, -352.1044303154654358 ) ) ;
#25058 = CARTESIAN_POINT ( 'NONE',  ( 771.1735550268778070, -225.1800572038743269, -316.3353852180827630 ) ) ;
#25059 = CARTESIAN_POINT ( 'NONE',  ( 781.8018195045266339, -406.2709662947829088, 365.1927285166406705 ) ) ;
#25060 = CARTESIAN_POINT ( 'NONE',  ( 782.4968714119720516, -154.8164208402382371, -305.0891759886411023 ) ) ;
#25061 = ORIENTED_EDGE ( 'NONE', *, *, #16217, .T. ) ;
#25062 = CARTESIAN_POINT ( 'NONE',  ( 759.9864689768902508, -146.0891481129655176, -354.9819416627836404 ) ) ;
#25063 = ORIENTED_EDGE ( 'NONE', *, *, #39172, .T. ) ;
#25064 = CARTESIAN_POINT ( 'NONE',  ( 776.9254006560222479, -404.1908817542431507, -314.8983024940802125 ) ) ;
#25065 = CARTESIAN_POINT ( 'NONE',  ( 804.1601925771018387, -127.4419599262326983, 346.5483106153029098 ) ) ;
#25068 = CARTESIAN_POINT ( 'NONE',  ( 788.7631598425961101, -385.4419599262319593, 305.7194118038759143 ) ) ;
#25067 = CARTESIAN_POINT ( 'NONE',  ( 175.6195620086261613, 290.0000000000001137, -244.9999999999999716 ) ) ;
#25066 = CARTESIAN_POINT ( 'NONE',  ( -190.7583438952258916, 294.6698570112193920, -274.9999999999999432 ) ) ;
#25069 = ORIENTED_EDGE ( 'NONE', *, *, #20475, .T. ) ;
#25070 = CARTESIAN_POINT ( 'NONE',  ( 766.9102291470427417, -402.5545181178795247, -318.6633372737382501 ) ) ;
#25071 = CARTESIAN_POINT ( 'NONE',  ( 998.9999999999992042, 249.9999999999998863, 360.0000000000000000 ) ) ;
#25072 = CARTESIAN_POINT ( 'NONE',  ( 744.6391490659812007, -182.7363362996983369, -338.7502325331110455 ) ) ;
#25073 = CARTESIAN_POINT ( 'NONE',  ( 776.2046728542105711, -20.19088175424429110, 304.8212110874238761 ) ) ;
#25075 = DIRECTION ( 'NONE',  ( 0.000000000000000000, 0.000000000000000000, 1.000000000000000000 ) ) ;
#25074 = DIRECTION ( 'NONE',  ( -0.000000000000000000, 1.000000000000000000, -0.000000000000000000 ) ) ;
#25076 = CARTESIAN_POINT ( 'NONE',  ( 805.1016975059191054, -294.8965053807775689, -343.0745993439771837 ) ) ;
#25077 = PLANE ( 'NONE',  #25478 ) ;
#25078 = CARTESIAN_POINT ( 'NONE',  ( 811.3240766477731540, -172.3726999360619914, -355.6651683502462902 ) ) ;
#25079 = CARTESIAN_POINT ( 'NONE',  ( -829.9999999999992042, 430.0000000000002842, -319.9999999999996021 ) ) ;
#25080 = DIRECTION ( 'NONE',  ( 0.000000000000000000, 0.000000000000000000, 1.000000000000000000 ) ) ;
#25081 = CARTESIAN_POINT ( 'NONE',  ( 760.7433823573367135, -372.0090635724250205, 355.9930595647440441 ) ) ;
#25082 = CARTESIAN_POINT ( 'NONE',  ( 750.9282345327678740, -328.9181544815160692, 319.8311093483690115 ) ) ;
#25083 = CARTESIAN_POINT ( 'NONE',  ( 747.2067596250078623, -219.1800572038744122, -352.2312462859687230 ) ) ;
#25084 = DIRECTION ( 'NONE',  ( -0.000000000000000000, -6.938893903907222461E-16, 1.000000000000000000 ) ) ;
#25085 = CARTESIAN_POINT ( 'NONE',  ( 797.6776695296629214, 4.456306432488530866, -357.6776695296636603 ) ) ;
#25086 = CARTESIAN_POINT ( 'NONE',  ( 783.7953271457878373, -152.1908817542438612, 375.1787889125761239 ) ) ;
#25087 = CARTESIAN_POINT ( 'NONE',  ( 746.7653713866222915, -89.26014174441463922, -351.0478386215610271 ) ) ;
#25088 = CARTESIAN_POINT ( 'NONE',  ( 800.9747183278959710, -132.9982390220564810, 311.9810565676471583 ) ) ;
#25089 = CARTESIAN_POINT ( 'NONE',  ( 810.7187646348534145, -330.4527844766013231, -356.7737145352016341 ) ) ;
#25090 = DIRECTION ( 'NONE',  ( 1.000000000000000000, 0.000000000000000000, 0.000000000000000000 ) ) ;
#25091 = CARTESIAN_POINT ( 'NONE',  ( 939.9999999999993179, 56.78581973499407809, -212.6378164459127618 ) ) ;
#25092 = CARTESIAN_POINT ( 'NONE',  ( 800.2193346964447755, -210.9982390220561967, 355.1360043628815788 ) ) ;
#25093 = CARTESIAN_POINT ( 'NONE',  ( 814.2805881961230625, -457.6454272087884760, 331.2368401574024119 ) ) ;
#25094 = CARTESIAN_POINT ( 'NONE',  ( 814.8230680027162407, -413.8055962898681059, -333.7305795820267917 ) ) ;
#25095 = CARTESIAN_POINT ( 'NONE',  ( 772.5602148656447525, -417.7255117493283478, -305.7998596910095443 ) ) ;
#25096 = LINE ( 'NONE', #14732, #21751 ) ;
#25097 = CARTESIAN_POINT ( 'NONE',  ( 776.2433038121456548, 11.10349461922141145, 374.8207195650711014 ) ) ;
#25098 = ORIENTED_EDGE ( 'NONE', *, *, #35167, .F. ) ;
#25099 = CARTESIAN_POINT ( 'NONE',  ( 749.8865473780648472, -188.5328690171416497, -322.1177392798429082 ) ) ;
#25100 = CARTESIAN_POINT ( 'NONE',  ( 775.4999999999993179, -512.9681489794448908, -339.9999999999999432 ) ) ;
#25101 = CARTESIAN_POINT ( 'NONE',  ( 786.2056067578752163, -323.8055962898684470, 374.4686193811670023 ) ) ;
#25102 = CARTESIAN_POINT ( 'NONE',  ( 804.6798772138710092, -159.7255117493291436, 334.6312213355106451 ) ) ;
#25103 = ORIENTED_EDGE ( 'NONE', *, *, #39979, .T. ) ;
#25104 = CARTESIAN_POINT ( 'NONE',  ( 774.6312213355099630, -311.3618753856922581, 364.6798772138717482 ) ) ;
#25105 = CARTESIAN_POINT ( 'NONE',  ( 777.4774526936600978, -34.27096629478407408, -304.7301800767027657 ) ) ;
#25106 = EDGE_CURVE ( 'NONE', #12726, #23746, #6450, .T. ) ;
#25107 = CARTESIAN_POINT ( 'NONE',  ( 772.5602148656447525, -81.72551174932937101, 305.7998596910095443 ) ) ;
#25108 = ORIENTED_EDGE ( 'NONE', *, *, #30616, .T. ) ;
#25109 = CARTESIAN_POINT ( 'NONE',  ( 795.8262568251477660, -430.3726999360611671, -308.3538107759623585 ) ) ;
#25110 = ORIENTED_EDGE ( 'NONE', *, *, #35912, .T. ) ;
#25111 = APPLICATION_PROTOCOL_DEFINITION ( 'draft international standard', 'automotive_design', 1998, #32571 ) ;
#25112 = CARTESIAN_POINT ( 'NONE',  ( 781.8018195045266339, -22.27096629478410250, 365.1927285166406705 ) ) ;
#25113 = CARTESIAN_POINT ( 'NONE',  ( 804.9363028652555840, -280.2709662947833067, -338.2165204200192079 ) ) ;
#25115 = CARTESIAN_POINT ( 'NONE',  ( 793.4146539503750546, -289.9874144716866908, 307.6481478633938877 ) ) ;
#25114 = CARTESIAN_POINT ( 'NONE',  ( 801.1904061080338124, -380.0891481129647218, 368.3070685750236066 ) ) ;
#25116 = CARTESIAN_POINT ( 'NONE',  ( 810.1134526219336749, -80.53286901714194812, 357.8822607201570349 ) ) ;
#25117 = CARTESIAN_POINT ( 'NONE',  ( 760.7433823573367135, -276.0090635724253048, -355.9930595647440441 ) ) ;
#25118 = CARTESIAN_POINT ( 'NONE',  ( 803.4237431249931660, -279.1800572038741848, -331.2633955100225194 ) ) ;
#25119 = CARTESIAN_POINT ( 'NONE',  ( 800.0135310231082713, -446.0891481129646081, -325.0180583372163028 ) ) ;
#25120 = CARTESIAN_POINT ( 'NONE',  ( 788.7366044899766848, -131.9073299311473875, -316.5762568750059813 ) ) ;
#25121 = CARTESIAN_POINT ( 'NONE',  ( -789.9999999999992042, 240.0000000000000853, -360.0000000000000000 ) ) ;
#25122 = EDGE_LOOP ( 'NONE', ( #8469, #39272, #42586, #16156 ) ) ;
#25123 = CARTESIAN_POINT ( 'NONE',  ( 812.7932403749906598, -375.1800572038739574, 327.7687537140311633 ) ) ;
#25125 = DIRECTION ( 'NONE',  ( -1.000000000000000000, 0.000000000000000000, 0.000000000000000000 ) ) ;
#25124 = DIRECTION ( 'NONE',  ( 1.000000000000000000, 0.000000000000000000, 0.000000000000000000 ) ) ;
#25126 = CARTESIAN_POINT ( 'NONE',  ( 793.5525998758768083, -79.09997266333503774, -372.6845335610516941 ) ) ;
#25127 = DIRECTION ( 'NONE',  ( -1.000000000000000000, -0.000000000000000000, -0.000000000000000000 ) ) ;
#25128 = DIRECTION ( 'NONE',  ( 0.000000000000000000, 0.000000000000000000, -1.000000000000000000 ) ) ;
#25129 = CARTESIAN_POINT ( 'NONE',  ( 763.0428371773158460, -275.4636090269708575, 358.7617431975195359 ) ) ;
#25130 = CARTESIAN_POINT ( 'NONE',  ( 767.8955696845333705, -168.4527844766018347, 362.1676090361162323 ) ) ;
#25131 = EDGE_LOOP ( 'NONE', ( #17690, #31652, #23607, #31438 ) ) ;
#25132 = CARTESIAN_POINT ( 'NONE',  ( 793.9708237608222134, -46.91815448151694312, -319.2295555964448681 ) ) ;
#25133 = CARTESIAN_POINT ( 'NONE',  ( 804.7487373415286811, -115.5436935675110988, -364.7487373415288516 ) ) ;
#25134 = CARTESIAN_POINT ( 'NONE',  ( 779.4709603349208464, -336.3510508353228943, 314.7162404726379918 ) ) ;
#25135 = CARTESIAN_POINT ( 'NONE',  ( 999.9999999999992042, -600.0000000000001137, -360.0000000000000000 ) ) ;
#25136 = CARTESIAN_POINT ( 'NONE',  ( 745.7194118038753459, -37.64542720878968396, 348.7631598425976449 ) ) ;
#25137 = CARTESIAN_POINT ( 'NONE',  ( 782.4968714119720516, -226.8164208402380098, -305.0891759886411023 ) ) ;
#25138 = CARTESIAN_POINT ( 'NONE',  ( 751.9810565676468741, -194.0891481129654039, 360.9747183278973921 ) ) ;
#25139 = CARTESIAN_POINT ( 'NONE',  ( 802.1676090361156639, -110.6346026584201638, 327.8955696845344505 ) ) ;
#25140 = CARTESIAN_POINT ( 'NONE',  ( 701.1634899080286232, 258.0939999999999372, -199.9999999999990337 ) ) ;
#25141 = CARTESIAN_POINT ( 'NONE',  ( 751.2241431872005251, -304.1692326535048210, -359.9636004259367610 ) ) ;
#25142 = CARTESIAN_POINT ( 'NONE',  ( 804.1009440267234822, -455.4636090269701754, 314.0944755984392600 ) ) ;
#25143 = CARTESIAN_POINT ( 'NONE',  ( 746.8695393053150156, -317.9073299311468190, -327.6429770376306010 ) ) ;
#25144 = FACE_OUTER_BOUND ( 'NONE', #11146, .T. ) ;
#25145 = CARTESIAN_POINT ( 'NONE',  ( 794.1144889064781864, -370.1692326535045936, 360.9840315886528401 ) ) ;
#25146 = CARTESIAN_POINT ( 'NONE',  ( 808.0189434323515343, -62.08914811296580183, 319.0252816721025511 ) ) ;
#25147 = CARTESIAN_POINT ( 'NONE',  ( 805.1927285166397041, -400.8164208402373561, -341.8018195045277707 ) ) ;
#25148 = CARTESIAN_POINT ( 'NONE',  ( 758.6633372737375112, -68.53286901714197654, 326.9102291470432533 ) ) ;
#25149 = CARTESIAN_POINT ( 'NONE',  ( 767.8955696845333705, -192.4527844766016926, -362.1676090361162323 ) ) ;
#25151 = EDGE_CURVE ( 'NONE', #26480, #21150, #9901, .T. ) ;
#25150 = CARTESIAN_POINT ( 'NONE',  ( 756.1443688327750579, -69.62377810805107003, -314.3581564841659315 ) ) ;
#25152 = CARTESIAN_POINT ( 'NONE',  ( 815.1787889125755555, -222.8965053807778531, 343.7953271457877804 ) ) ;
#25153 = CARTESIAN_POINT ( 'NONE',  ( 759.9864689768902508, -2.089148112965993231, 354.9819416627836404 ) ) ;
#25154 = ORIENTED_EDGE ( 'NONE', *, *, #34453, .T. ) ;
#25155 = CARTESIAN_POINT ( 'NONE',  ( 793.2243759319678702, -218.5328690171414792, -318.4439275373583200 ) ) ;
#25156 = CARTESIAN_POINT ( 'NONE',  ( 757.8323909638827445, -194.6346026584198796, 352.1044303154654358 ) ) ;
#25157 = EDGE_CURVE ( 'NONE', #16297, #30803, #15250, .T. ) ;
#25158 = CARTESIAN_POINT ( 'NONE',  ( 810.1134526219336749, -32.53286901714208312, -357.8822607201570349 ) ) ;
#25159 = CARTESIAN_POINT ( 'NONE',  ( 781.7834795799800531, -322.8164208402377540, 315.0636971347436202 ) ) ;
#25160 = EDGE_CURVE ( 'NONE', #15183, #35055, #25557, .T. ) ;
#25161 = CARTESIAN_POINT ( 'NONE',  ( 939.9999999999993179, -600.0000000000001137, 360.0000000000000000 ) ) ;
#25162 = CARTESIAN_POINT ( 'NONE',  ( -775.4999999999993179, -513.1383975375929367, -350.0000000000000000 ) ) ;
#25163 = ORIENTED_EDGE ( 'NONE', *, *, #14227, .T. ) ;
#25164 = CARTESIAN_POINT ( 'NONE',  ( 802.7791456095903868, -52.71468719896020616, 329.0155153010375102 ) ) ;
#25165 = CARTESIAN_POINT ( 'NONE',  ( 799.9636004259356241, -358.9181544815160123, -311.2241431872006956 ) ) ;
#25166 = CARTESIAN_POINT ( 'NONE',  ( 758.8095938919644823, -296.0891481129650629, 311.6929314249762797 ) ) ;
#25167 = CARTESIAN_POINT ( 'NONE',  ( 807.5423716828161105, -9.078323562596708030, 362.2119215644372048 ) ) ;
#25168 = CARTESIAN_POINT ( 'NONE',  ( 804.6971507214547046, -195.2817908451528410, -344.0799538623459739 ) ) ;
#25169 = CARTESIAN_POINT ( 'NONE',  ( 804.6798772138708955, -159.7255117493291436, -334.6312213355107019 ) ) ;
#25170 = CARTESIAN_POINT ( 'NONE',  ( 756.3353852180820240, -365.9073299311466485, -331.1735550268787733 ) ) ;
#25171 = ORIENTED_EDGE ( 'NONE', *, *, #689, .F. ) ;
#25172 = CARTESIAN_POINT ( 'NONE',  ( 755.2512626584698410, -295.5436935675105588, 315.2512626584710915 ) ) ;
#25173 = LINE ( 'NONE', #14809, #9326 ) ;
#25174 = CARTESIAN_POINT ( 'NONE',  ( 755.8398074228967971, -355.4419599262319593, 333.4516893846970333 ) ) ;
#25175 = FACE_OUTER_BOUND ( 'NONE', #20347, .T. ) ;
#25176 = CARTESIAN_POINT ( 'NONE',  ( 784.1219089521767955, -141.2817908451530400, 315.0488828828318333 ) ) ;
#25177 = CARTESIAN_POINT ( 'NONE',  ( 797.6776695296629214, -43.54369356751131903, 357.6776695296636603 ) ) ;
#25178 = ORIENTED_EDGE ( 'NONE', *, *, #9772, .F. ) ;
#25179 = CARTESIAN_POINT ( 'NONE',  ( 745.5313806188320314, -423.2817908451521589, -333.7943932421247268 ) ) ;
#25180 = CARTESIAN_POINT ( 'NONE',  ( 747.2067596250078623, -3.180057203875080063, -352.2312462859687230 ) ) ;
#25181 = CARTESIAN_POINT ( 'NONE',  ( 771.3260364891663130, -259.6454272087890445, 306.0683387631859773 ) ) ;
#25182 = CARTESIAN_POINT ( 'NONE',  ( 766.7756240680305382, -230.5328690171415076, 361.5560724626415663 ) ) ;
#25183 = CARTESIAN_POINT ( 'NONE',  ( 785.3687786644884454, -371.3618753856919739, -315.3201227861279676 ) ) ;
#25184 = CARTESIAN_POINT ( 'NONE',  ( 755.3201227861273992, -3.725511749329622813, 345.3687786644892981 ) ) ;
#25185 = LINE ( 'NONE', #7207, #6781 ) ;
#25186 = CARTESIAN_POINT ( 'NONE',  ( 757.4527132478984868, -208.3726999360619061, -329.1273215169538844 ) ) ;
#25187 = CARTESIAN_POINT ( 'NONE',  ( 745.0891759886404770, -28.27096629478409540, 342.4968714119734159 ) ) ;
#25188 = CARTESIAN_POINT ( 'NONE',  ( 814.2001403089898304, -113.3618753856929260, 347.4397851343538264 ) ) ;
#25189 = DIRECTION ( 'NONE',  ( 0.000000000000000000, 0.000000000000000000, 1.000000000000000000 ) ) ;
#25190 = CARTESIAN_POINT ( 'NONE',  ( 745.7998596910086917, -437.3618753856919170, -332.5602148656461168 ) ) ;
#25191 = DIRECTION ( 'NONE',  ( 0.000000000000000000, 1.000000000000000000, 0.000000000000000000 ) ) ;
#25192 = CARTESIAN_POINT ( 'NONE',  ( 747.6481478633932056, -373.0999726633340856, 353.4146539503763620 ) ) ;
#25193 = CARTESIAN_POINT ( 'NONE',  ( 799.9999999999993179, -373.0259173205825505, -36.60293108048681887 ) ) ;
#25194 = CARTESIAN_POINT ( 'NONE',  ( 746.8695393053150156, -341.9073299311465917, 327.6429770376306010 ) ) ;
#25195 = CARTESIAN_POINT ( 'NONE',  ( 755.2512626584698410, -79.54369356751119824, -315.2512626584710915 ) ) ;
#25196 = CARTESIAN_POINT ( 'NONE',  ( 781.7834795799800531, -298.8164208402377540, -315.0636971347436202 ) ) ;
#25197 = EDGE_CURVE ( 'NONE', #29001, #14103, #13377, .T. ) ;
#25198 = CARTESIAN_POINT ( 'NONE',  ( 791.7608162188021197, 205.0000000000000568, -319.9999999999999432 ) ) ;
#25199 =( REPRESENTATION_RELATIONSHIP ('NONE','NONE', #39835, #18903 ) REPRESENTATION_RELATIONSHIP_WITH_TRANSFORMATION ( #34433 )SHAPE_REPRESENTATION_RELATIONSHIP( ) );
#25200 = CARTESIAN_POINT ( 'NONE',  ( 797.6776695296629214, -427.5436935675101040, 357.6776695296636603 ) ) ;
#25201=STYLED_ITEM('',(#45744),#17219);
#25202 = CARTESIAN_POINT ( 'NONE',  ( 786.5483106153019435, -175.6454272087892718, 364.1601925771022366 ) ) ;
#25203 = CARTESIAN_POINT ( 'NONE',  ( 745.1792804349281596, -62.19088175424416676, -343.7566961878542884 ) ) ;
#25204 = CARTESIAN_POINT ( 'NONE',  ( 765.8855110935204493, -94.16923265350555994, -319.0159684113471599 ) ) ;
#25205 = CARTESIAN_POINT ( 'NONE',  ( 795.6651683502461765, -106.7146871989600498, 371.3240766477733814 ) ) ;
#25206 = CARTESIAN_POINT ( 'NONE',  ( 781.7834795799800531, -418.8164208402374129, 315.0636971347436202 ) ) ;
#25207 = CARTESIAN_POINT ( 'NONE',  ( 757.8323909638827445, -2.634602658420536869, -352.1044303154654358 ) ) ;
#25208 = ORIENTED_EDGE ( 'NONE', *, *, #39964, .T. ) ;
#25209 = CARTESIAN_POINT ( 'NONE',  ( 755.0636971347428243, -100.2709662947838609, -341.7834795799807353 ) ) ;
#25210 = EDGE_CURVE ( 'NONE', #5848, #43744, #3198, .T. ) ;
#25211 = CARTESIAN_POINT ( 'NONE',  ( 804.9511171171677688, -413.8055962898681059, -335.8780910478229202 ) ) ;
#25213 = CARTESIAN_POINT ( 'NONE',  ( 781.8018195045267476, -238.2709662947833920, 365.1927285166407273 ) ) ;
#25212 = CARTESIAN_POINT ( 'NONE',  ( 755.5713283507202505, -221.3618753856925707, 334.6858677611754729 ) ) ;
#25214 = CARTESIAN_POINT ( 'NONE',  ( 771.2368401574024119, -397.4419599262317320, -374.2805881961240857 ) ) ;
#25215 = CARTESIAN_POINT ( 'NONE',  ( -200.7583438952258916, 294.6698570112193920, -244.9999999999999716 ) ) ;
#25216 = ORIENTED_EDGE ( 'NONE', *, *, #2708, .T. ) ;
#25217 = CARTESIAN_POINT ( 'NONE',  ( 757.8323909638827445, -434.6346026584190554, 352.1044303154654358 ) ) ;
#25218 = ORIENTED_EDGE ( 'NONE', *, *, #19956, .F. ) ;
#25219 = SHAPE_REPRESENTATION_RELATIONSHIP ( 'NONE' , 'NONE' ,  #28408, #10570 ) ;
#25220 = CARTESIAN_POINT ( 'NONE',  ( 814.9108240113580450, -256.2709662947834204, -337.5031285880265273 ) ) ;
#25221 = CARTESIAN_POINT ( 'NONE',  ( 782.4968714119720516, -178.8164208402381519, 305.0891759886411023 ) ) ;
#25222 = CARTESIAN_POINT ( 'NONE',  ( 758.4439275373578084, -252.5545181178799226, 353.2243759319684386 ) ) ;
#25223 = CARTESIAN_POINT ( 'NONE',  ( 754.9735926884551418, -378.3510508353227806, 340.5236548041000333 ) ) ;
#25224 = ORIENTED_EDGE ( 'NONE', *, *, #20487, .F. ) ;
#25225 = CARTESIAN_POINT ( 'NONE',  ( 780.5236548040995785, -92.73633629969860692, -314.9735926884559944 ) ) ;
#25226 = CARTESIAN_POINT ( 'NONE',  ( 749.8865473780648472, -188.5328690171416497, 322.1177392798429082 ) ) ;
#25227 = CARTESIAN_POINT ( 'NONE',  ( 804.6798772138710092, -255.7255117493287742, -334.6312213355106451 ) ) ;
#25228 = ORIENTED_EDGE ( 'NONE', *, *, #20988, .F. ) ;
#25229 = EDGE_CURVE ( 'NONE', #10285, #32281, #38781, .T. ) ;
#25230 = CARTESIAN_POINT ( 'NONE',  ( 757.8323909638827445, -410.6346026584191122, -352.1044303154654358 ) ) ;
#25231 = CARTESIAN_POINT ( 'NONE',  ( 758.0580252608178853, -54.45278447660219001, -328.0187753319985404 ) ) ;
#25232 = ADVANCED_FACE ( 'NONE', ( #7138 ), #31379, .F. ) ;
#25233 = CARTESIAN_POINT ( 'NONE',  ( 802.7791456095903868, -244.7146871989596093, 329.0155153010375102 ) ) ;
#25234 = DIRECTION ( 'NONE',  ( -0.000000000000000000, 1.000000000000000000, -0.000000000000000000 ) ) ;
#25235 = CARTESIAN_POINT ( 'NONE',  ( 989.9999999999992042, 56.73212367640085318, 362.5753187112032379 ) ) ;
#25236 = VERTEX_POINT ( 'NONE', #20742 ) ;
#25237 = CARTESIAN_POINT ( 'NONE',  ( 758.0580252608178853, -30.45278447660226817, -328.0187753319985404 ) ) ;
#25238 = DIRECTION ( 'NONE',  ( 1.000000000000000000, -0.000000000000000000, -0.000000000000000000 ) ) ;
#25239 = FACE_BOUND ( 'NONE', #18273, .T. ) ;
#25240 = ORIENTED_EDGE ( 'NONE', *, *, #28330, .F. ) ;
#25241 = CARTESIAN_POINT ( 'NONE',  ( 799.9636004259356241, -286.9181544815161828, -311.2241431872006956 ) ) ;
#25242 = VECTOR ( 'NONE', #20640, 1000.000000000000000 ) ;
#25243 = CARTESIAN_POINT ( 'NONE',  ( 762.1177392798416577, -186.5545181178801215, 309.8865473780659272 ) ) ;
#25245 = CARTESIAN_POINT ( 'NONE',  ( 755.5713283507202505, -245.3618753856925139, -334.6858677611754729 ) ) ;
#25244 = CARTESIAN_POINT ( 'NONE',  ( 999.9999999999992042, -590.0000000000001137, -360.0000000000000000 ) ) ;
#25246 = CARTESIAN_POINT ( 'NONE',  ( 757.4527132478984868, -112.3726999360621761, -329.1273215169538844 ) ) ;
#25247 = CARTESIAN_POINT ( 'NONE',  ( 814.5518280994195948, -15.72551174932958951, 332.4837098697145734 ) ) ;
#25248 = DIRECTION ( 'NONE',  ( 0.000000000000000000, 0.000000000000000000, -1.000000000000000000 ) ) ;
#25249 = CARTESIAN_POINT ( 'NONE',  ( 815.1787889125755555, -6.896505380778533478, -343.7953271457877804 ) ) ;
#25250 = CARTESIAN_POINT ( 'NONE',  ( 777.5031285880264704, -310.8164208402377540, -374.9108240113588408 ) ) ;
#25251 = PLANE ( 'NONE',  #40859 ) ;
#25252 = CARTESIAN_POINT ( 'NONE',  ( 801.9419747391806368, 5.547215523397618142, 351.9812246680014027 ) ) ;
#25253 = ADVANCED_FACE ( 'NONE', ( #24435 ), #42463, .F. ) ;
#25254 = CARTESIAN_POINT ( 'NONE',  ( 810.4231160770870019, -264.5545181178798657, 321.9338519418446936 ) ) ;
#25255 = CARTESIAN_POINT ( 'NONE',  ( 747.3154664389472828, -211.9874144716869750, -326.4474001241230781 ) ) ;
#25256 = CARTESIAN_POINT ( 'NONE',  ( 787.4397851343537695, -237.7255117493289163, 374.2001403089903988 ) ) ;
#25257 = CARTESIAN_POINT ( 'NONE',  ( 757.7880784355613741, 5.990936427573807954, -312.4576283171834916 ) ) ;
#25258 = PLANE ( 'NONE',  #35040 ) ;
#25259 = EDGE_CURVE ( 'NONE', #11032, #41260, #7366, .T. ) ;
#25260 = CARTESIAN_POINT ( 'NONE',  ( 768.0187753319979720, -320.6346026584195670, 318.0580252608186242 ) ) ;
#25261 = AXIS2_PLACEMENT_3D ( 'NONE', #16568, #17020, #27631 ) ;
#25262 = CARTESIAN_POINT ( 'NONE',  ( 804.6971507214547046, -99.28179084515313946, 344.0799538623459739 ) ) ;
#25263 = CARTESIAN_POINT ( 'NONE',  ( 775.8780910478218402, -81.28179084515319630, 364.9511171171680530 ) ) ;
#25264 = CARTESIAN_POINT ( 'NONE',  ( 801.3366627262608972, 15.46713098285775878, -353.0897708529566899 ) ) ;
#25265 = CARTESIAN_POINT ( 'NONE',  ( 701.1634899080286232, 229.9999999999999147, -199.9999999999990337 ) ) ;
#25266 = CARTESIAN_POINT ( 'NONE',  ( 919.9999999999993179, 154.9999999999998863, 359.9749999999999659 ) ) ;
#25268 = CARTESIAN_POINT ( 'NONE',  ( 800.2193346964447755, -354.9982390220557704, 355.1360043628815788 ) ) ;
#25267 = CARTESIAN_POINT ( 'NONE',  ( 799.4546378042377910, -153.0783235625962675, 356.1575198192848006 ) ) ;
#25269 = EDGE_LOOP ( 'NONE', ( #33034, #15970 ) ) ;
#25270 = EDGE_CURVE ( 'NONE', #20663, #4785, #31611, .T. ) ;
#25271 = EDGE_CURVE ( 'NONE', #31800, #45067, #10139, .T. ) ;
#25272 = CARTESIAN_POINT ( 'NONE',  ( 769.1273215169530886, -286.7146871989594388, -317.4527132478988847 ) ) ;
#25273 = CARTESIAN_POINT ( 'NONE',  ( 768.0187753319979720, -128.6346026584201354, 318.0580252608186242 ) ) ;
#25274 = CARTESIAN_POINT ( 'NONE',  ( 759.8311093483677041, -310.1692326535048778, -310.9282345327691814 ) ) ;
#25275 = FACE_OUTER_BOUND ( 'NONE', #39470, .T. ) ;
#25276 = CARTESIAN_POINT ( 'NONE',  ( 792.2312462859673587, 12.09267006885214180, 307.2067596250082602 ) ) ;
#25277 = EDGE_LOOP ( 'NONE', ( #27427, #33103 ) ) ;
#25278 = CARTESIAN_POINT ( 'NONE',  ( 781.8018195045266339, -334.2709662947829656, 365.1927285166406705 ) ) ;
#25279 = CARTESIAN_POINT ( 'NONE',  ( 756.7813123517142913, -67.98741447168742980, -329.9779781133712504 ) ) ;
#25280 = CARTESIAN_POINT ( 'NONE',  ( 795.1360043628807261, -164.0891481129655176, -360.2193346964456282 ) ) ;
#25281 = CARTESIAN_POINT ( 'NONE',  ( 794.9819416627830151, -444.9982390220554862, 319.9864689768909898 ) ) ;
#25282 = CARTESIAN_POINT ( 'NONE',  ( 746.8695393053150156, -149.9073299311473875, -327.6429770376306010 ) ) ;
#25283 = ORIENTED_EDGE ( 'NONE', *, *, #4027, .F. ) ;
#25284 = CARTESIAN_POINT ( 'NONE',  ( 758.0580252608178853, -126.4527844766019626, -328.0187753319985404 ) ) ;
#25285 = EDGE_LOOP ( 'NONE', ( #37353, #8069, #42269, #10292 ) ) ;
#25286 = CARTESIAN_POINT ( 'NONE',  ( 769.0155153010367712, -418.3726999360612808, -362.7791456095907279 ) ) ;
#25287 = EDGE_CURVE ( 'NONE', #19382, #34117, #4946, .T. ) ;
#25288 = CARTESIAN_POINT ( 'NONE',  ( 791.9460785601769430, -462.7578698805381237, 362.0383033825738721 ) ) ;
#25289 = CARTESIAN_POINT ( 'NONE',  ( 749.2812353651451076, -222.4527844766016642, 323.2262854647983090 ) ) ;
#25290 = CARTESIAN_POINT ( 'NONE',  ( 756.1348686366196716, -113.2601417444145682, 347.5531968255698416 ) ) ;
#25293 = CARTESIAN_POINT ( 'NONE',  ( 768.8385539511368734, -407.2601417444137155, 306.4236121716840557 ) ) ;
#25292 = DIRECTION ( 'NONE',  ( 0.000000000000000000, 0.7071067811865578978, 0.7071067811865372477 ) ) ;
#25291 = DIRECTION ( 'NONE',  ( 0.000000000000000000, 0.000000000000000000, 1.000000000000000000 ) ) ;
#25294 = ORIENTED_EDGE ( 'NONE', *, *, #11400, .T. ) ;
#25295 = CARTESIAN_POINT ( 'NONE',  ( 776.9254006560222479, -380.1908817542431507, -314.8983024940802125 ) ) ;
#25296 = DIRECTION ( 'NONE',  ( 0.000000000000000000, 0.000000000000000000, -1.000000000000000000 ) ) ;
#25297 = VECTOR ( 'NONE', #9581, 1000.000000000000000 ) ;
#25298 = CARTESIAN_POINT ( 'NONE',  ( 809.0717654672305343, -172.9181544815165239, -360.1688906516309885 ) ) ;
#25299 = PRODUCT_DEFINITION_FORMATION_WITH_SPECIFIED_SOURCE ( 'ANY', '', #79, .NOT_KNOWN. ) ;
#25300 = CARTESIAN_POINT ( 'NONE',  ( 791.0478386215596629, -69.82724539060775726, 306.7653713866226326 ) ) ;
#25302 = LINE ( 'NONE', #32703, #39547 ) ;
#25301 = CARTESIAN_POINT ( 'NONE',  ( -28.63011601220122415, -365.3551492539851893, -18.13243251470705886 ) ) ;
#25303 = CARTESIAN_POINT ( 'NONE',  ( 787.6308680596127942, -323.2601417444138860, -364.1105419155492768 ) ) ;
#25304 = FACE_OUTER_BOUND ( 'NONE', #37029, .T. ) ;
#25305 = CARTESIAN_POINT ( 'NONE',  ( 764.1737431748507561, -178.3726999360619629, -371.6461892240376415 ) ) ;
#25306 = DIRECTION ( 'NONE',  ( 1.880165489482579047E-16, 1.000000000000000000, 0.000000000000000000 ) ) ;
#25307 = CARTESIAN_POINT ( 'NONE',  ( -786.4999999999993179, -110.5936016518799221, 750.6326042729449455 ) ) ;
#25308 = CARTESIAN_POINT ( 'NONE',  ( 800.9840315886518738, -364.9181544815158986, 354.1144889064786412 ) ) ;
#25309 = CARTESIAN_POINT ( 'NONE',  ( 748.6759233522253680, -352.3726999360614514, 324.3348316497537098 ) ) ;
#25310 = CARTESIAN_POINT ( 'NONE',  ( 759.0252816721024374, -216.9982390220562252, -368.0189434323527280 ) ) ;
#25311 = CARTESIAN_POINT ( 'NONE',  ( 919.9999999999993179, 219.9999999999998863, -360.0000000000000000 ) ) ;
#25312 = CARTESIAN_POINT ( 'NONE',  ( 762.1405469898971887, -25.54369356751136877, -357.8594530101015607 ) ) ;
#25313 = EDGE_CURVE ( 'NONE', #38247, #12844, #28138, .T. ) ;
#25314 = CARTESIAN_POINT ( 'NONE',  ( 804.1009440267234822, -143.4636090269711701, 314.0944755984392600 ) ) ;
#25315 = CARTESIAN_POINT ( 'NONE',  ( 810.1134526219336749, -104.5328690171418913, -357.8822607201570349 ) ) ;
#25316 = CARTESIAN_POINT ( 'NONE',  ( 810.7187646348534145, -114.4527844766020053, 356.7737145352016341 ) ) ;
#25317 = CARTESIAN_POINT ( 'NONE',  ( 805.0032342141412300, -349.5436935675102745, -314.9967657858571783 ) ) ;
#25318 = DIRECTION ( 'NONE',  ( -0.000000000000000000, -0.000000000000000000, -1.000000000000000000 ) ) ;
#25320 = EDGE_CURVE ( 'NONE', #17032, #34365, #38322, .T. ) ;
#25319 = CYLINDRICAL_SURFACE ( 'NONE', #15404, 2.749999999999835687 ) ;
#25321 = CARTESIAN_POINT ( 'NONE',  ( 785.3687786644884454, -203.3618753856925991, 315.3201227861279676 ) ) ;
#25322 = CARTESIAN_POINT ( 'NONE',  ( 798.5707757039680246, -5.463609026971610660, 356.7845633553585003 ) ) ;
#25323 = CARTESIAN_POINT ( 'NONE',  ( 768.8385539511368734, -407.2601417444137155, -306.4236121716840557 ) ) ;
#25324 = CARTESIAN_POINT ( 'NONE',  ( 782.4968714119720516, -418.8164208402374129, -305.0891759886411023 ) ) ;
#25325 = DIRECTION ( 'NONE',  ( -1.000000000000000000, -0.000000000000000000, -0.000000000000000000 ) ) ;
#25326 = CARTESIAN_POINT ( 'NONE',  ( 791.1614460488616487, -35.26014174441480264, 373.5763878283158874 ) ) ;
#25327 = ORIENTED_EDGE ( 'NONE', *, *, #640, .T. ) ;
#25328 = CARTESIAN_POINT ( 'NONE',  ( 765.8855110935204493, -190.1692326535052189, -319.0159684113471599 ) ) ;
#25329 = VECTOR ( 'NONE', #4423, 999.9999999999998863 ) ;
#25330 = CARTESIAN_POINT ( 'NONE',  ( 805.1927285166397041, -40.81642084023859951, 341.8018195045277707 ) ) ;
#25331 = CARTESIAN_POINT ( 'NONE',  ( 771.2368401574024119, -205.4419599262324425, -374.2805881961240857 ) ) ;
#25332 =( LENGTH_UNIT ( ) NAMED_UNIT ( * ) SI_UNIT ( .MILLI., .METRE. ) );
#25333 = CARTESIAN_POINT ( 'NONE',  ( 814.8230680027162407, -293.8055962898685607, 333.7305795820267917 ) ) ;
#25334 = CARTESIAN_POINT ( 'NONE',  ( 781.8018195045267476, -166.2709662947836478, 365.1927285166407273 ) ) ;
#25335 = ORIENTED_EDGE ( 'NONE', *, *, #17898, .F. ) ;
#25336 = CARTESIAN_POINT ( 'NONE',  ( 797.8594530101008786, -325.5436935675105019, 322.1405469898980982 ) ) ;
#25337 = CARTESIAN_POINT ( 'NONE',  ( 810.7187646348534145, -42.45278447660223264, -356.7737145352016341 ) ) ;
#25338 = CARTESIAN_POINT ( 'NONE',  ( 804.7487373415286811, -91.54369356751116982, 364.7487373415288516 ) ) ;
#25339 = ORIENTED_EDGE ( 'NONE', *, *, #19836, .T. ) ;
#25340 = CARTESIAN_POINT ( 'NONE',  ( 812.3518521366052028, -433.0999726633339151, -326.5853460496235243 ) ) ;
#25341 = ORIENTED_EDGE ( 'NONE', *, *, #1019, .T. ) ;
#25342 = SHAPE_DEFINITION_REPRESENTATION ( #41751, #28315 ) ;
#25343 = AXIS2_PLACEMENT_3D ( 'NONE', #2902, #28276, #38697 ) ;
#25345 = CARTESIAN_POINT ( 'NONE',  ( 779.4763451958990572, -368.7363362996977685, 365.0264073115438919 ) ) ;
#25344 = CARTESIAN_POINT ( 'NONE',  ( 774.6312213355099630, -47.36187538569312494, 364.6798772138717482 ) ) ;
#25346 = CARTESIAN_POINT ( 'NONE',  ( 758.0580252608178853, -294.4527844766013800, -328.0187753319985404 ) ) ;
#25348 = CARTESIAN_POINT ( 'NONE',  ( 810.1134526219336749, -296.5328690171411949, 357.8822607201570349 ) ) ;
#25347 = CARTESIAN_POINT ( 'NONE',  ( 805.0032342141413437, -397.5436935675101040, 314.9967657858572352 ) ) ;
#25349 = CARTESIAN_POINT ( 'NONE',  ( 748.3538107759620743, -64.71468719896019195, 355.8262568251490165 ) ) ;
#25350 = CARTESIAN_POINT ( 'NONE',  ( 784.1219089521767955, -285.2817908451526137, -315.0488828828318333 ) ) ;
#25351 = CARTESIAN_POINT ( 'NONE',  ( 804.4286716492782716, -305.3618753856922581, -345.3141322388244703 ) ) ;
#25352 = FACE_OUTER_BOUND ( 'NONE', #16116, .T. ) ;
#25353 = CARTESIAN_POINT ( 'NONE',  ( 802.1676090361156639, -110.6346026584201638, -327.8955696845344505 ) ) ;
#25354 = PLANE ( 'NONE',  #5538 ) ;
#25355 = ORIENTED_EDGE ( 'NONE', *, *, #16680, .F. ) ;
#25356 = CARTESIAN_POINT ( 'NONE',  ( 777.4774526936600978, -394.2709662947827951, 304.7301800767027657 ) ) ;
#25358 = CARTESIAN_POINT ( 'NONE',  ( 759.9999999999992042, 205.0000000000000568, -360.0000000000000000 ) ) ;
#25357 = DIRECTION ( 'NONE',  ( -0.000000000000000000, -0.000000000000000000, 1.000000000000000000 ) ) ;
#25359 = CARTESIAN_POINT ( 'NONE',  ( 750.9282345327678740, -88.91815448151682233, -319.8311093483690115 ) ) ;
#25360 = LINE ( 'NONE', #43595, #12325 ) ;
#25361 = CARTESIAN_POINT ( 'NONE',  ( 879.9999999999992042, 529.9999999999997726, -360.0000000000000000 ) ) ;
#25362 = CARTESIAN_POINT ( 'NONE',  ( 754.7162404726377645, -278.7363362996980527, 339.4709603349214717 ) ) ;
#25363 = CARTESIAN_POINT ( 'NONE',  ( 774.6312213355099630, -167.3618753856927412, 364.6798772138717482 ) ) ;
#25364 = ORIENTED_EDGE ( 'NONE', *, *, #12787, .T. ) ;
#25365 = CARTESIAN_POINT ( 'NONE',  ( 804.4086373105744769, -49.64542720878965554, -333.3843516231986541 ) ) ;
#25366 = VECTOR ( 'NONE', #35203, 1000.000000000000114 ) ;
#25367 = CIRCLE ( 'NONE', #21676, 2.749999999999919176 ) ;
#25368 = CARTESIAN_POINT ( 'NONE',  ( 772.4837098697145166, -119.3618753856928834, -374.5518280994205611 ) ) ;
#25369 = CARTESIAN_POINT ( 'NONE',  ( 802.7791456095903868, -316.7146871989593819, 329.0155153010375102 ) ) ;
#25370 = CARTESIAN_POINT ( 'NONE',  ( 791.9812246680005501, -452.6346026584191691, -361.9419747391813189 ) ) ;
#25371 = CARTESIAN_POINT ( 'NONE',  ( 768.9521613784389729, -57.82724539060780700, 373.2346286133773106 ) ) ;
#25372 = CARTESIAN_POINT ( 'NONE',  ( 751.6929314249748586, -246.9982390220560546, -318.8095938919659034 ) ) ;
#25373 = CARTESIAN_POINT ( 'NONE',  ( 792.2312462859673587, -203.9073299311471885, 307.2067596250082602 ) ) ;
#25374 = CARTESIAN_POINT ( 'NONE',  ( 765.0180583372156207, -120.9982390220565378, 360.0135310231089534 ) ) ;
#25375 = LINE ( 'NONE', #4376, #29911 ) ;
#25376 = CARTESIAN_POINT ( 'NONE',  ( 813.9316612368132837, -295.4419599262320730, -348.6739635108323228 ) ) ;
#25377 = AXIS2_PLACEMENT_3D ( 'NONE', #34731, #3570, #3330 ) ;
#25378 = CARTESIAN_POINT ( 'NONE',  ( 814.2805881961230625, -457.6454272087884760, 331.2368401574024119 ) ) ;
#25379 = CARTESIAN_POINT ( 'NONE',  ( 810.7187646348534145, -306.4527844766013800, -356.7737145352016341 ) ) ;
#25380 = CARTESIAN_POINT ( 'NONE',  ( -28.63011601220122415, -365.3551492539851893, -28.13243251470704109 ) ) ;
#25381 = CARTESIAN_POINT ( 'NONE',  ( 766.7756240680305382, -350.5328690171411381, 361.5560724626415663 ) ) ;
#25382 = CARTESIAN_POINT ( 'NONE',  ( -338.8365100919713200, 256.5000000000001137, -197.2499999999918714 ) ) ;
#25383 = CARTESIAN_POINT ( 'NONE',  ( 781.7834795799800531, -418.8164208402374129, -315.0636971347436202 ) ) ;
#25384 = CARTESIAN_POINT ( 'NONE',  ( 759.2295555964440155, -64.16923265350563099, 353.9708237608231229 ) ) ;
#25385 = CARTESIAN_POINT ( 'NONE',  ( 803.4237431249931660, -207.1800572038744406, -331.2633955100225194 ) ) ;
#25386 = CARTESIAN_POINT ( 'NONE',  ( 744.9990715423526808, -90.35105083532373271, -341.2370466360926002 ) ) ;
#25387 = CARTESIAN_POINT ( 'NONE',  ( 813.9316612368132837, -199.4419599262324709, 348.6739635108323228 ) ) ;
#25388 = CARTESIAN_POINT ( 'NONE',  ( 788.8264449731201466, -69.18005720387488111, 363.6646147819170665 ) ) ;
#25389 = VERTEX_POINT ( 'NONE', #21442 ) ;
#25390 = CARTESIAN_POINT ( 'NONE',  ( 796.7845633553578182, -225.6237781080506011, -358.5707757039688204 ) ) ;
#25391 = CARTESIAN_POINT ( 'NONE',  ( 778.2165204200184689, -190.8164208402381234, 364.9363028652563230 ) ) ;
#25392 = CARTESIAN_POINT ( 'NONE',  ( 746.7653713866222915, -41.26014174441479554, -351.0478386215610271 ) ) ;
#25393 = CARTESIAN_POINT ( 'NONE',  ( 797.8594530101009923, -349.5436935675103314, 322.1405469898982119 ) ) ;
#25394 = DIRECTION ( 'NONE',  ( 1.000000000000000000, -0.000000000000000000, -0.000000000000000000 ) ) ;
#25395 = DIRECTION ( 'NONE',  ( 1.000000000000000000, 0.000000000000000000, -0.000000000000000000 ) ) ;
#25396 = AXIS2_PLACEMENT_3D ( 'NONE', #38166, #2824, #38862 ) ;
#25397 = ORIENTED_EDGE ( 'NONE', *, *, #1807, .T. ) ;
#25398 = CARTESIAN_POINT ( 'NONE',  ( 755.8398074228967971, -43.44195992623296831, 333.4516893846970333 ) ) ;
#25399 = CARTESIAN_POINT ( 'NONE',  ( 760.0363995740630116, -346.9181544815160123, -368.7758568127991907 ) ) ;
#25400 = CARTESIAN_POINT ( 'NONE',  ( 763.0537975583476964, -288.4527844766014937, 371.0346526505628617 ) ) ;
#25401 = CARTESIAN_POINT ( 'NONE',  ( 759.8311093483677041, 1.830767346494167391, 310.9282345327691814 ) ) ;
#25402 = CARTESIAN_POINT ( 'NONE',  ( 769.0155153010367712, -202.3726999360618777, -362.7791456095907279 ) ) ;
#25403 = CARTESIAN_POINT ( 'NONE',  ( 756.5762568750052424, -171.1800572038745543, -348.7366044899774238 ) ) ;
#25404 = CARTESIAN_POINT ( 'NONE',  ( 762.1405469898973024, -337.5436935675102745, -357.8594530101016176 ) ) ;
#25405 = ORIENTED_EDGE ( 'NONE', *, *, #31393, .T. ) ;
#25406 = CARTESIAN_POINT ( 'NONE',  ( 804.1601925771018387, 16.55804007376685050, -346.5483106153029098 ) ) ;
#25407 = CARTESIAN_POINT ( 'NONE',  ( 782.5225473063381969, -286.2709662947833635, 375.2698199232970637 ) ) ;
#25408 = AXIS2_PLACEMENT_3D ( 'NONE', #29555, #8976, #8764 ) ;
#25409 = DIRECTION ( 'NONE',  ( -1.000000000000000000, -0.000000000000000000, 0.000000000000000000 ) ) ;
#25410 = CARTESIAN_POINT ( 'NONE',  ( 802.9823548866075953, -217.0999726633345972, 330.0799878456151077 ) ) ;
#25411 = CARTESIAN_POINT ( 'NONE',  ( -338.8365100919713200, 258.0940000000001078, -199.9999999999917861 ) ) ;
#25412 = AXIS2_PLACEMENT_3D ( 'NONE', #37069, #29479, #36398 ) ;
#25413 = CARTESIAN_POINT ( 'NONE',  ( 798.5707757039680246, -149.4636090269711417, 356.7845633553585003 ) ) ;
#25414 = CARTESIAN_POINT ( 'NONE',  ( 800.2193346964447755, -42.99823902205675807, 355.1360043628815788 ) ) ;
#25415 = ORIENTED_EDGE ( 'NONE', *, *, #33439, .T. ) ;
#25416 = CARTESIAN_POINT ( 'NONE',  ( 786.2694204179717872, -429.2817908451521021, -305.1769319972829067 ) ) ;
#25417 = CARTESIAN_POINT ( 'NONE',  ( 763.2262854647970016, 15.36539734157940629, -309.2812353651462445 ) ) ;
#25418 = CARTESIAN_POINT ( 'NONE',  ( 757.7880784355613741, -258.0090635724253616, 312.4576283171834916 ) ) ;
#25419 = CARTESIAN_POINT ( 'NONE',  ( 770.0799878456142551, -229.9874144716869466, 362.9823548866085616 ) ) ;
#25420 = CARTESIAN_POINT ( 'NONE',  ( 762.3223304703356007, -367.5436935675102745, -322.3223304703362828 ) ) ;
#25421 = CARTESIAN_POINT ( 'NONE',  ( 779.9999999999992042, -462.9681489794448339, 339.9999999999999432 ) ) ;
#25422 = CARTESIAN_POINT ( 'NONE',  ( 800.0135310231082713, 9.910851887033969021, 325.0180583372163028 ) ) ;
#25423 = DIRECTION ( 'NONE',  ( -1.000000000000000000, 0.000000000000000000, 0.000000000000000000 ) ) ;
#25424 = CARTESIAN_POINT ( 'NONE',  ( 755.8894580844503253, -255.8272453906072315, -332.3691319403863531 ) ) ;
#25425 = CARTESIAN_POINT ( 'NONE',  ( 777.4774526936600978, -58.27096629478398171, 304.7301800767027657 ) ) ;
#25426 = CARTESIAN_POINT ( 'NONE',  ( 808.3070685750230950, -114.9982390220565236, 361.1904061080339261 ) ) ;
#25427 = PLANE ( 'NONE',  #42415 ) ;
#25428 = DIRECTION ( 'NONE',  ( 0.000000000000000000, 0.000000000000000000, 1.000000000000000000 ) ) ;
#25429 = AXIS2_PLACEMENT_3D ( 'NONE', #29805, #30251, #19407 ) ;
#25430 = LINE ( 'NONE', #4641, #26152 ) ;
#25431 = VECTOR ( 'NONE', #6343, 1000.000000000000000 ) ;
#25432 = CARTESIAN_POINT ( 'NONE',  ( 762.1177392798416577, -378.5545181178795247, 309.8865473780659272 ) ) ;
#25433 = DIRECTION ( 'NONE',  ( -1.058954862565134068E-16, 0.6438296778008191223, 0.7651688349527137056 ) ) ;
#25434 = CARTESIAN_POINT ( 'NONE',  ( 763.0537975583475827, -312.4527844766012663, 371.0346526505627480 ) ) ;
#25435 = CARTESIAN_POINT ( 'NONE',  ( 785.3141322388236176, -333.7255117493286320, -364.4286716492789537 ) ) ;
#25436 = CARTESIAN_POINT ( 'NONE',  ( -332.7175100919712918, 256.5000000000001137, -199.9999999999917861 ) ) ;
#25437 = CARTESIAN_POINT ( 'NONE',  ( 800.0135310231082713, -446.0891481129646081, 325.0180583372163028 ) ) ;
#25438 = CIRCLE ( 'NONE', #355, 6.119000000000013095 ) ;
#25439 = CARTESIAN_POINT ( 'NONE',  ( 802.9823548866075953, -193.0999726633346256, 330.0799878456151077 ) ) ;
#25440 = CARTESIAN_POINT ( 'NONE',  ( 749.5768839229115201, -60.55451811788051941, -358.0661480581553064 ) ) ;
#25441 = CARTESIAN_POINT ( 'NONE',  ( 789.9200121543843807, -97.98741447168734453, -317.0176451133914384 ) ) ;
#25442 = CARTESIAN_POINT ( 'NONE',  ( 761.9338519418445230, -110.5328690171418629, 370.4231160770881957 ) ) ;
#25443 = CARTESIAN_POINT ( 'NONE',  ( 797.6776695296629214, -427.5436935675101040, 357.6776695296636603 ) ) ;
#25444 = AXIS2_PLACEMENT_3D ( 'NONE', #28108, #20504, #34593 ) ;
#25445 = CARTESIAN_POINT ( 'NONE',  ( 762.3223304703356007, 16.45630643248849267, -322.3223304703362828 ) ) ;
#25447 = VERTEX_POINT ( 'NONE', #20971 ) ;
#25446 = CARTESIAN_POINT ( 'NONE',  ( 804.9511171171677688, -101.8055962898691718, -335.8780910478229202 ) ) ;
#25448 = CARTESIAN_POINT ( 'NONE',  ( 756.5762568750052424, -99.18005720387478164, -348.7366044899774238 ) ) ;
#25449 = VECTOR ( 'NONE', #26237, 1000.000000000000227 ) ;
#25450 = CIRCLE ( 'NONE', #30629, 10.00000000000000888 ) ;
#25451 = CARTESIAN_POINT ( 'NONE',  ( 775.9200461376533440, -383.8055962898682765, -315.3028492785443291 ) ) ;
#25453 = CARTESIAN_POINT ( 'NONE',  ( 774.6312213355098493, -215.3618753856925707, 364.6798772138717482 ) ) ;
#25452 = CARTESIAN_POINT ( 'NONE',  ( 803.4237431249931660, -279.1800572038741848, 331.2633955100225194 ) ) ;
#25454 = CARTESIAN_POINT ( 'NONE',  ( 441.1634899080286232, 259.9999999999999432, -199.9999999999972431 ) ) ;
#25455 = ORIENTED_EDGE ( 'NONE', *, *, #22148, .F. ) ;
#25456 = CARTESIAN_POINT ( 'NONE',  ( 804.6798772138708955, -423.7255117493281205, 334.6312213355107019 ) ) ;
#25457 = ORIENTED_EDGE ( 'NONE', *, *, #16508, .T. ) ;
#25458 = CARTESIAN_POINT ( 'NONE',  ( 745.4481719005789273, -171.7255117493290868, 347.5162901302853697 ) ) ;
#25459 = AXIS2_PLACEMENT_3D ( 'NONE', #27359, #23648, #44924 ) ;
#25460 = CARTESIAN_POINT ( 'NONE',  ( 790.0220218866281812, -271.0999726633344267, 363.2186876482849129 ) ) ;
#25461 = VERTEX_POINT ( 'NONE', #3441 ) ;
#25462 = CARTESIAN_POINT ( 'NONE',  ( 763.8424801807145741, -90.00906357242590161, -320.5453621957614700 ) ) ;
#25463 = CARTESIAN_POINT ( 'NONE',  ( 746.0683387631852383, -235.4419599262323857, 331.3260364891676204 ) ) ;
#25464 = CARTESIAN_POINT ( 'NONE',  ( 778.2165204200184689, -238.8164208402379813, -364.9363028652563230 ) ) ;
#25465 = VECTOR ( 'NONE', #35756, 1000.000000000000000 ) ;
#25466 = ORIENTED_EDGE ( 'NONE', *, *, #39960, .F. ) ;
#25467 = CARTESIAN_POINT ( 'NONE',  ( 785.3687786644884454, -395.3618753856918602, -315.3201227861279676 ) ) ;
#25468 = CARTESIAN_POINT ( 'NONE',  ( 756.3353852180819104, -53.90732993114765037, -331.1735550268788302 ) ) ;
#25469 = AXIS2_PLACEMENT_3D ( 'NONE', #31893, #10904, #24970 ) ;
#25470 = CARTESIAN_POINT ( 'NONE',  ( 754.9735926884551418, -282.3510508353230080, 340.5236548041000333 ) ) ;
#25471 = DIRECTION ( 'NONE',  ( -1.000000000000000000, 4.147566128926363633E-16, 0.000000000000000000 ) ) ;
#25472 = CARTESIAN_POINT ( 'NONE',  ( 200.7583438952259485, 394.6698570112193920, -274.9999999999999432 ) ) ;
#25473 = EDGE_CURVE ( 'NONE', #40963, #25447, #45714, .T. ) ;
#25474 = CARTESIAN_POINT ( 'NONE',  ( 804.9363028652555840, -16.27096629478413092, -338.2165204200192079 ) ) ;
#25475 = CARTESIAN_POINT ( 'NONE',  ( 786.4999999999993179, -513.1383975375929367, -349.9999999999999432 ) ) ;
#25476 = ORIENTED_EDGE ( 'NONE', *, *, #28401, .F. ) ;
#25477 = CARTESIAN_POINT ( 'NONE',  ( 752.7379699480933368, -300.0090635724252479, -361.9858362298580232 ) ) ;
#25478 = AXIS2_PLACEMENT_3D ( 'NONE', #7541, #21617, #35699 ) ;
#25479 = CARTESIAN_POINT ( 'NONE',  ( 754.3581564841646241, -161.4636090269711133, 316.1443688327762516 ) ) ;
#25480 = VECTOR ( 'NONE', #44013, 1000.000000000000000 ) ;
#25482 = CARTESIAN_POINT ( 'NONE',  ( 756.3353852180819104, -269.9073299311468190, -331.1735550268788302 ) ) ;
#25481 = CARTESIAN_POINT ( 'NONE',  ( 939.9999999999992042, 46.15097736693707020, 350.0000000000000000 ) ) ;
#25483 = DIRECTION ( 'NONE',  ( 1.000000000000000000, 0.000000000000000000, 0.000000000000000000 ) ) ;
#25484 = CARTESIAN_POINT ( 'NONE',  ( 790.9844846989617508, -142.3726999360620766, -317.2208543904092721 ) ) ;
#25485 = EDGE_CURVE ( 'NONE', #37198, #1029, #9367, .T. ) ;
#25486 = AXIS2_PLACEMENT_3D ( 'NONE', #25265, #4493, #18585 ) ;
#25487 =( REPRESENTATION_RELATIONSHIP ('NONE','NONE', #39835, #10941 ) REPRESENTATION_RELATIONSHIP_WITH_TRANSFORMATION ( #23786 )SHAPE_REPRESENTATION_RELATIONSHIP( ) );
#25488 = CARTESIAN_POINT ( 'NONE',  ( 748.9653473494363425, -26.63460265842045871, 356.9462024416521331 ) ) ;
#25489 = FACE_OUTER_BOUND ( 'NONE', #7466, .T. ) ;
#25490 = CARTESIAN_POINT ( 'NONE',  ( 776.2433038121456548, -12.89650538077851216, -374.8207195650711014 ) ) ;
#25491 = CARTESIAN_POINT ( 'NONE',  ( 787.5162901302840055, -347.3618753856922012, -305.4481719005793252 ) ) ;
#25492 = DIRECTION ( 'NONE',  ( -0.000000000000000000, 0.000000000000000000, -1.000000000000000000 ) ) ;
#25493 = CARTESIAN_POINT ( 'NONE',  ( 801.9419747391806368, -18.45278447660230725, 351.9812246680014027 ) ) ;
#25494 = CARTESIAN_POINT ( 'NONE',  ( 752.7379699480933368, -276.0090635724253048, 361.9858362298580232 ) ) ;
#25495 = CARTESIAN_POINT ( 'NONE',  ( 773.7943932421234194, -215.8055962898687881, -305.5313806188329409 ) ) ;
#25496 = CARTESIAN_POINT ( 'NONE',  ( 767.7687537140311633, -239.9073299311470748, 372.7932403749916830 ) ) ;
#25497 = CARTESIAN_POINT ( 'NONE',  ( 808.3070685750230950, 5.001760977943074948, -361.1904061080339261 ) ) ;
#25498 = CYLINDRICAL_SURFACE ( 'NONE', #18075, 9.999999999999982236 ) ;
#25499 = ORIENTED_EDGE ( 'NONE', *, *, #25793, .T. ) ;
#25500 = CARTESIAN_POINT ( 'NONE',  ( 803.4237431249931660, -327.1800572038741279, 331.2633955100225194 ) ) ;
#25501 = AXIS2_PLACEMENT_3D ( 'NONE', #43028, #29621, #19010 ) ;
#25502 = CARTESIAN_POINT ( 'NONE',  ( 796.9571628226829034, -95.46360902697132644, 321.2382568024804641 ) ) ;
#25503 = CARTESIAN_POINT ( 'NONE',  ( 779.4709603349208464, 23.64894916467591912, -314.7162404726379918 ) ) ;
#25504 = VECTOR ( 'NONE', #28776, 1000.000000000000000 ) ;
#25505 = CARTESIAN_POINT ( 'NONE',  ( -37.63011601220122770, 22.32581219114657856, 895.6886905569881492 ) ) ;
#25506 = CARTESIAN_POINT ( 'NONE',  ( -728.8365100919714905, 240.0000000000001990, -199.9999999999890861 ) ) ;
#25508 = CARTESIAN_POINT ( 'NONE',  ( 804.6798772138708955, -375.7255117493283478, 334.6312213355107019 ) ) ;
#25507 = CARTESIAN_POINT ( 'NONE',  ( 755.8398074228967971, -163.4419599262325846, 333.4516893846970333 ) ) ;
#25509 = VERTEX_POINT ( 'NONE', #24665 ) ;
#25510 = CARTESIAN_POINT ( 'NONE',  ( 761.2382568024794409, -303.6237781080503169, -356.9571628226838129 ) ) ;
#25511 = CARTESIAN_POINT ( 'NONE',  ( 758.0580252608178853, -174.4527844766018063, 328.0187753319985404 ) ) ;
#25512 = CARTESIAN_POINT ( 'NONE',  ( 793.4146539503750546, -337.9874144716865771, -307.6481478633938877 ) ) ;
#25513 = DIRECTION ( 'NONE',  ( 1.892425610156518354E-16, 1.000000000000000000, -0.000000000000000000 ) ) ;
#25514 = CARTESIAN_POINT ( 'NONE',  ( 811.6461892240364477, -436.7146871989589272, 324.1737431748509835 ) ) ;
#25515 = VERTEX_POINT ( 'NONE', #17762 ) ;
#25516 = CARTESIAN_POINT ( 'NONE',  ( 767.8955696845333705, -312.4527844766012663, 362.1676090361162323 ) ) ;
#25517 = AXIS2_PLACEMENT_3D ( 'NONE', #1678, #15782, #40507 ) ;
#25518 = CARTESIAN_POINT ( 'NONE',  ( 800.7704444035546203, -76.16923265350557415, -326.0291762391768771 ) ) ;
#25519 = CARTESIAN_POINT ( 'NONE',  ( 797.6776695296629214, -427.5436935675101040, 357.6776695296636603 ) ) ;
#25520 = CIRCLE ( 'NONE', #10023, 18.00000000000001421 ) ;
#25521 = CARTESIAN_POINT ( 'NONE',  ( 792.3570229623688874, -165.1800572038745258, -373.1304606946836202 ) ) ;
#25522 = ORIENTED_EDGE ( 'NONE', *, *, #28735, .T. ) ;
#25523 = CARTESIAN_POINT ( 'NONE',  ( 802.1676090361155502, -134.6346026584201070, -327.8955696845344505 ) ) ;
#25524 = ORIENTED_EDGE ( 'NONE', *, *, #11876, .F. ) ;
#25525 = CARTESIAN_POINT ( 'NONE',  ( 804.8461984189677878, -410.1908817542430370, -336.9566956441385628 ) ) ;
#25526 = EDGE_CURVE ( 'NONE', #25236, #19734, #17491, .T. ) ;
#25527 = CARTESIAN_POINT ( 'NONE',  ( 790.7339360641449275, -462.9631818684622999, 362.6136660859752965 ) ) ;
#25528 = CARTESIAN_POINT ( 'NONE',  ( 814.2001403089898304, -233.3618753856925423, 347.4397851343538264 ) ) ;
#25529 = CARTESIAN_POINT ( 'NONE',  ( 804.1601925771018387, -151.4419599262326415, 346.5483106153029098 ) ) ;
#25532 = CARTESIAN_POINT ( 'NONE',  ( 764.3348316497523456, -382.7146871989591546, 308.6759233522265617 ) ) ;
#25531 = CARTESIAN_POINT ( 'NONE',  ( 779.9999999999992042, -462.9681489794448339, -370.0000000000000568 ) ) ;
#25530 = LINE ( 'NONE', #21833, #1893 ) ;
#25533 = EDGE_CURVE ( 'NONE', #12108, #45635, #18904, .T. ) ;
#25534 = ORIENTED_EDGE ( 'NONE', *, *, #41383, .T. ) ;
#25535 = CARTESIAN_POINT ( 'NONE',  ( 776.9254006560222479, -404.1908817542431507, -314.8983024940802125 ) ) ;
#25536 = DIRECTION ( 'NONE',  ( 1.000000000000000000, -0.000000000000000000, -0.000000000000000000 ) ) ;
#25537 = CARTESIAN_POINT ( 'NONE',  ( 807.2620300519052989, -192.0090635724255606, -318.0141637701419768 ) ) ;
#25538 = CARTESIAN_POINT ( 'NONE',  ( 810.4231160770870019, -72.55451811788049099, 321.9338519418446936 ) ) ;
#25539 = AXIS2_PLACEMENT_3D ( 'NONE', #43743, #19489, #8672 ) ;
#25541 = CARTESIAN_POINT ( 'NONE',  ( 311.1634899080286232, 240.0000000000000000, -199.9999999999963336 ) ) ;
#25540 = CYLINDRICAL_SURFACE ( 'NONE', #36664, 2.749999999999835687 ) ;
#25542 = CARTESIAN_POINT ( 'NONE',  ( 784.0799538623451781, -323.8055962898684470, -364.6971507214555572 ) ) ;
#25543 = FACE_OUTER_BOUND ( 'NONE', #1521, .T. ) ;
#25544 = CARTESIAN_POINT ( 'NONE',  ( 748.6759233522253680, -184.3726999360619629, -324.3348316497537098 ) ) ;
#25545 = CARTESIAN_POINT ( 'NONE',  ( -454.7528517110260964, 200.0000000000001137, -122.7905160835438068 ) ) ;
#25546 = CARTESIAN_POINT ( 'NONE',  ( 758.7867965644027208, 16.45630643248849267, -318.7867965644036872 ) ) ;
#25547 = EDGE_CURVE ( 'NONE', #42263, #19442, #39926, .T. ) ;
#25548 = CARTESIAN_POINT ( 'NONE',  ( 754.7162404726377645, -398.7363362996976548, 339.4709603349214717 ) ) ;
#25549 = CARTESIAN_POINT ( 'NONE',  ( 813.1304606946831655, -233.9073299311470464, -352.3570229623691716 ) ) ;
#25550 = DIRECTION ( 'NONE',  ( 0.000000000000000000, 1.000000000000000000, 0.000000000000000000 ) ) ;
#25551 = CARTESIAN_POINT ( 'NONE',  ( 762.3223304703356007, -7.543693567511430942, -322.3223304703362828 ) ) ;
#25552 = COLOUR_RGB ( '',0.7921568627450980005, 0.8196078431372548767, 0.9333333333333333481 ) ;
#25553 = CARTESIAN_POINT ( 'NONE',  ( 795.8262568251477660, -166.3726999360620198, 308.3538107759623585 ) ) ;
#25554 = CARTESIAN_POINT ( 'NONE',  ( 749.8865473780648472, -92.53286901714190549, -322.1177392798429082 ) ) ;
#25555 = CARTESIAN_POINT ( 'NONE',  ( 767.6429770376289525, -105.1800572038747248, 306.8695393053162093 ) ) ;
#25556 = CARTESIAN_POINT ( 'NONE',  ( 777.5031285880264704, -382.8164208402374697, -374.9108240113588408 ) ) ;
#25557 = CIRCLE ( 'NONE', #27033, 10.00000000000000888 ) ;
#25558 = CARTESIAN_POINT ( 'NONE',  ( 311.1634899080286232, 260.0000000000000000, -199.9999999999963336 ) ) ;
#25559 = PLANE ( 'NONE',  #13152 ) ;
#25560 = CARTESIAN_POINT ( 'NONE',  ( 804.6798772138708955, -207.7255117493289447, 334.6312213355107019 ) ) ;
#25561 = CARTESIAN_POINT ( 'NONE',  ( 766.4474001241216001, -451.0999726633339151, 307.3154664389482491 ) ) ;
#25562 = ADVANCED_FACE ( 'NONE', ( #18668 ), #8269, .T. ) ;
#25563 = CARTESIAN_POINT ( 'NONE',  ( 754.0944755984390895, -399.6237781080500326, -364.1009440267246760 ) ) ;
#25564 = CARTESIAN_POINT ( 'NONE',  ( 801.1904061080336987, -452.0891481129646650, -368.3070685750235498 ) ) ;
#25566 = EDGE_CURVE ( 'NONE', #14504, #5020, #17986, .T. ) ;
#25565 = CARTESIAN_POINT ( 'NONE',  ( -858.8365100919713768, 256.5000000000002274, -197.2499999999882334 ) ) ;
#25567 = CARTESIAN_POINT ( 'NONE',  ( 744.8212110874229666, -18.89650538077849617, 336.2046728542121627 ) ) ;
#25568 = EDGE_LOOP ( 'NONE', ( #26316, #43174, #37220, #19597 ) ) ;
#25569 = CARTESIAN_POINT ( 'NONE',  ( 779.4709603349208464, -192.3510508353233774, -314.7162404726379918 ) ) ;
#25570 = CARTESIAN_POINT ( 'NONE',  ( 762.3223304703356007, -7.543693567511430942, 322.3223304703362828 ) ) ;
#25571 = CARTESIAN_POINT ( 'NONE',  ( 811.6461892240364477, -172.7146871989598083, -324.1737431748509835 ) ) ;
#25572 = FILL_AREA_STYLE_COLOUR ( '', #7650 ) ;
#25573 = CARTESIAN_POINT ( 'NONE',  ( 798.0661480581538854, -338.5328690171411381, 309.5768839229118043 ) ) ;
#25574 = CARTESIAN_POINT ( 'NONE',  ( 795.1360043628808398, -140.0891481129655176, 360.2193346964456282 ) ) ;
#25575 = ORIENTED_EDGE ( 'NONE', *, *, #3488, .T. ) ;
#25576 = CARTESIAN_POINT ( 'NONE',  ( 758.0580252608178853, -150.4527844766018916, -328.0187753319985404 ) ) ;
#25577 = CARTESIAN_POINT ( 'NONE',  ( 771.1735550268778070, -345.1800572038739006, 316.3353852180827630 ) ) ;
#25578 = AXIS2_PLACEMENT_3D ( 'NONE', #41104, #6452, #37161 ) ;
#25579 = CARTESIAN_POINT ( 'NONE',  ( 796.7737145352015204, -44.63460265842040542, -370.7187646348536987 ) ) ;
#25580 = EDGE_CURVE ( 'NONE', #20167, #26190, #4576, .T. ) ;
#25581 = ORIENTED_EDGE ( 'NONE', *, *, #19642, .F. ) ;
#25582 = CARTESIAN_POINT ( 'NONE',  ( 793.5525998758768083, -439.0999726633339719, -372.6845335610516941 ) ) ;
#25583 = AXIS2_PLACEMENT_3D ( 'NONE', #25916, #9288, #33768 ) ;
#25584 = EDGE_LOOP ( 'NONE', ( #5564, #41302, #23040, #33348, #2041, #38945, #6260, #23699, #3293, #44366, #2247 ) ) ;
#25585 = CARTESIAN_POINT ( 'NONE',  ( 790.9844846989617508, -310.3726999360616219, -317.2208543904092721 ) ) ;
#25586 = ITEM_DEFINED_TRANSFORMATION ( 'NONE', 'NONE', #20873,  #26858 ) ;
#25587 = EDGE_CURVE ( 'NONE', #34011, #23619, #11280, .T. ) ;
#25589 = CARTESIAN_POINT ( 'NONE',  ( 787.5531968255692163, -381.8272453906068336, 316.1348686366205811 ) ) ;
#25588 = CARTESIAN_POINT ( 'NONE',  ( 762.3223304703356007, -55.54369356751127640, 322.3223304703362828 ) ) ;
#25590 = CARTESIAN_POINT ( 'NONE',  ( 803.4237431249931660, -303.1800572038740711, -331.2633955100225194 ) ) ;
#25591 = AXIS2_PLACEMENT_3D ( 'NONE', #17237, #31323, #27870 ) ;
#25593 = CARTESIAN_POINT ( 'NONE',  ( 751.2241431872005251, -304.1692326535048210, 359.9636004259367610 ) ) ;
#25592 = CARTESIAN_POINT ( 'NONE',  ( 801.1904061080338124, -404.0891481129646650, 368.3070685750236066 ) ) ;
#25594 = EDGE_CURVE ( 'NONE', #16782, #25236, #43591, .T. ) ;
#25595 = CARTESIAN_POINT ( 'NONE',  ( 755.5913626894240451, -277.6454272087889308, -346.6156483768012890 ) ) ;
#25596 = CARTESIAN_POINT ( 'NONE',  ( 764.8639956371174549, -272.0891481129651197, -319.7806653035542013 ) ) ;
#25597 = CARTESIAN_POINT ( 'NONE',  ( 989.9999999999992042, 56.78581973499402835, -212.6378164459127049 ) ) ;
#25598 = CARTESIAN_POINT ( 'NONE',  ( 801.9419747391806368, -114.4527844766020053, -351.9812246680014027 ) ) ;
#25599 = LINE ( 'NONE', #36209, #17355 ) ;
#25600 = ORIENTED_EDGE ( 'NONE', *, *, #431, .F. ) ;
#25601 = CARTESIAN_POINT ( 'NONE',  ( 745.7998596910086917, -437.3618753856919170, 332.5602148656461168 ) ) ;
#25603 = CARTESIAN_POINT ( 'NONE',  ( 919.9999999999993179, 154.9999999999998863, 350.0000000000000000 ) ) ;
#25602 = CARTESIAN_POINT ( 'NONE',  ( -784.4999999999993179, -513.1383975375929367, -369.9999999999999432 ) ) ;
#25604 = CARTESIAN_POINT ( 'NONE',  ( 760.0363995740630116, -82.91815448151682233, -368.7758568127991907 ) ) ;
#25605 = DIRECTION ( 'NONE',  ( -0.000000000000000000, -0.000000000000000000, -1.000000000000000000 ) ) ;
#25606 = LINE ( 'NONE', #29310, #37058 ) ;
#25607 = CARTESIAN_POINT ( 'NONE',  ( 799.2566176426618085, -288.0090635724252479, 324.0069404352559559 ) ) ;
#25608 = CARTESIAN_POINT ( 'NONE',  ( 774.6858677611749044, -153.7255117493291721, 315.5713283507209894 ) ) ;
#25609 = ORIENTED_EDGE ( 'NONE', *, *, #28130, .T. ) ;
#25610 = CARTESIAN_POINT ( 'NONE',  ( 777.4774526936600978, -106.2709662947838467, -304.7301800767028226 ) ) ;
#25611 = CARTESIAN_POINT ( 'NONE',  ( 800.7704444035546203, -316.1692326535048210, 326.0291762391768771 ) ) ;
#25612 = LINE ( 'NONE', #23645, #8666 ) ;
#25613 = CARTESIAN_POINT ( 'NONE',  ( 812.3518521366052028, -25.09997266333519050, 326.5853460496235243 ) ) ;
#25615 = VECTOR ( 'NONE', #39929, 1000.000000000000000 ) ;
#25614 = CARTESIAN_POINT ( 'NONE',  ( 748.9653473494363425, -242.6346026584197659, -356.9462024416521331 ) ) ;
#25616 = CARTESIAN_POINT ( 'NONE',  ( 756.5762568750052424, -123.1800572038747106, 348.7366044899774238 ) ) ;
#25617 = FACE_OUTER_BOUND ( 'NONE', #23717, .T. ) ;
#25618 = CARTESIAN_POINT ( 'NONE',  ( 810.1134526219336749, -296.5328690171411949, -357.8822607201570349 ) ) ;
#25619 = AXIS2_PLACEMENT_3D ( 'NONE', #13249, #6306, #23836 ) ;
#25620 = CARTESIAN_POINT ( 'NONE',  ( 780.5236548040995785, -20.73633629969883430, 314.9735926884559944 ) ) ;
#25621 = CARTESIAN_POINT ( 'NONE',  ( 754.9967657858570647, -313.5436935675102745, -365.0032342141425374 ) ) ;
#25622 = CARTESIAN_POINT ( 'NONE',  ( 441.1634899080286232, 259.9999999999999432, -199.9999999999972431 ) ) ;
#25623 = CARTESIAN_POINT ( 'NONE',  ( 803.8651313633788504, -413.2601417444136018, 332.4468031744301015 ) ) ;
#25624 = VERTEX_POINT ( 'NONE', #39473 ) ;
#25625 = CARTESIAN_POINT ( 'NONE',  ( 788.8264449731200330, -405.1800572038737300, -363.6646147819171233 ) ) ;
#25626 = AXIS2_PLACEMENT_3D ( 'NONE', #36161, #32702, #11690 ) ;
#25627 = CARTESIAN_POINT ( 'NONE',  ( 785.3687786644884454, -227.3618753856925707, -315.3201227861279676 ) ) ;
#25628 = CARTESIAN_POINT ( 'NONE',  ( 778.7502325331095108, -96.35105083532370429, -304.6391490659818828 ) ) ;
#25629 = DIRECTION ( 'NONE',  ( 1.000000000000000000, -0.000000000000000000, -0.000000000000000000 ) ) ;
#25630 = CARTESIAN_POINT ( 'NONE',  ( 746.7653713866222915, -233.2601417444141987, 351.0478386215610271 ) ) ;
#25631 = CARTESIAN_POINT ( 'NONE',  ( 774.6858677611749044, -57.72551174932945628, 315.5713283507209894 ) ) ;
#25632 = VERTEX_POINT ( 'NONE', #22334 ) ;
#25633 = CARTESIAN_POINT ( 'NONE',  ( 802.7791456095903868, -220.7146871989596661, -329.0155153010375102 ) ) ;
#25634 = CARTESIAN_POINT ( 'NONE',  ( 774.6858677611749044, -225.7255117493289163, 315.5713283507209894 ) ) ;
#25635 = CARTESIAN_POINT ( 'NONE',  ( 756.1443688327750579, -69.62377810805107003, -314.3581564841659315 ) ) ;
#25636 = CARTESIAN_POINT ( 'NONE',  ( 808.7373736539768743, -452.9681489794446065, -336.0792598452978268 ) ) ;
#25637 = ORIENTED_EDGE ( 'NONE', *, *, #39667, .F. ) ;
#25638 = CARTESIAN_POINT ( 'NONE',  ( 781.2370466360911223, -356.7363362996978253, -304.9990715423533629 ) ) ;
#25639 =( BOUNDED_CURVE ( )  B_SPLINE_CURVE ( 3, ( #34819, #16602, #3424, #30685 ),
 .UNSPECIFIED., .F., .T. ) 
 B_SPLINE_CURVE_WITH_KNOTS ( ( 4, 4 ),
 ( 3.141592653589793116, 4.712388980384689674 ),
 .UNSPECIFIED. ) 
 CURVE ( )  GEOMETRIC_REPRESENTATION_ITEM ( )  RATIONAL_B_SPLINE_CURVE ( ( 1.000000000000000000, 0.8047378541243649375, 0.8047378541243649375, 1.000000000000000000 ) ) 
 REPRESENTATION_ITEM ( '' )  );
#25640 = CARTESIAN_POINT ( 'NONE',  ( 792.3570229623691148, -285.1800572038741279, 373.1304606946836770 ) ) ;
#25641 = CARTESIAN_POINT ( 'NONE',  ( 798.0661480581538854, -2.532869017142183932, 309.5768839229118043 ) ) ;
#25642 = CARTESIAN_POINT ( 'NONE',  ( 804.8461984189677878, -170.1908817542438328, -336.9566956441385628 ) ) ;
#25643 = CARTESIAN_POINT ( 'NONE',  ( 755.0636971347428243, -196.2709662947835909, -341.7834795799807353 ) ) ;
#25644 = CARTESIAN_POINT ( 'NONE',  ( 757.8323909638828582, -386.6346026584192828, -352.1044303154654358 ) ) ;
#25645 = ORIENTED_EDGE ( 'NONE', *, *, #9984, .F. ) ;
#25646 = CARTESIAN_POINT ( 'NONE',  ( 772.3691319403857278, 24.73985825558500551, -315.8894580844506663 ) ) ;
#25647 = VERTEX_POINT ( 'NONE', #21666 ) ;
#25648 = VECTOR ( 'NONE', #15069, 1000.000000000000000 ) ;
#25649 = CARTESIAN_POINT ( 'NONE',  ( 805.0032342141412300, -325.5436935675105019, 314.9967657858571783 ) ) ;
#25650 = DIRECTION ( 'NONE',  ( 0.000000000000000000, -1.000000000000000000, 0.000000000000000000 ) ) ;
#25651 = CARTESIAN_POINT ( 'NONE',  ( 756.7813123517142913, -355.9874144716865203, 329.9779781133712504 ) ) ;
#25652 = CARTESIAN_POINT ( 'NONE',  ( 772.4999999999993179, -462.9681489794447202, -270.0000000000000568 ) ) ;
#25653 = CARTESIAN_POINT ( 'NONE',  ( 763.0428371773158460, -155.4636090269711417, 358.7617431975195359 ) ) ;
#25654 = CARTESIAN_POINT ( 'NONE',  ( 768.0187753319979720, -56.63460265842036279, 318.0580252608186242 ) ) ;
#25655 = EDGE_LOOP ( 'NONE', ( #7798, #33639, #1734, #37379, #32566, #22727 ) ) ;
#25656 = CARTESIAN_POINT ( 'NONE',  ( 814.4686193811664907, -411.2817908451521589, -346.2056067578752732 ) ) ;
#25657 = CARTESIAN_POINT ( 'NONE',  ( 812.7932403749906598, -15.18005720387504631, -327.7687537140311633 ) ) ;
#25658 = CARTESIAN_POINT ( 'NONE',  ( 791.0478386215596629, -261.8272453906071746, 306.7653713866226326 ) ) ;
#25659 = CARTESIAN_POINT ( 'NONE',  ( 758.6633372737375112, -236.5328690171414792, 326.9102291470432533 ) ) ;
#25660 = CARTESIAN_POINT ( 'NONE',  ( 778.1981804954714335, -370.2709662947831362, -314.8072714833589885 ) ) ;
#25661 = FACE_OUTER_BOUND ( 'NONE', #42443, .T. ) ;
#25662 = CARTESIAN_POINT ( 'NONE',  ( 794.9819416627830151, 11.00176097794305541, 319.9864689768909898 ) ) ;
#25663 = LINE ( 'NONE', #7428, #32574 ) ;
#25664 = CARTESIAN_POINT ( 'NONE',  ( 804.1105419155481968, -243.8272453906072030, -347.6308680596136469 ) ) ;
#25665 = CARTESIAN_POINT ( 'NONE',  ( 814.2001403089898304, -41.36187538569314626, 347.4397851343538264 ) ) ;
#25666 = CARTESIAN_POINT ( 'NONE',  ( 767.7687537140311633, -119.9073299311474443, 372.7932403749916830 ) ) ;
#25667 = DIRECTION ( 'NONE',  ( 0.000000000000000000, -0.7651688349527138167, -0.6438296778008192334 ) ) ;
#25668 = FILL_AREA_STYLE_COLOUR ( '', #2575 ) ;
#25669 = CARTESIAN_POINT ( 'NONE',  ( 773.7305795820266212, -393.2817908451522726, 374.8230680027170365 ) ) ;
#25670 = LINE ( 'NONE', #39994, #27223 ) ;
#25671 = CARTESIAN_POINT ( 'NONE',  ( 767.6429770376289525, -369.1800572038739574, 306.8695393053162093 ) ) ;
#25672 = CARTESIAN_POINT ( 'NONE',  ( 757.8323909638827445, -314.6346026584194533, -352.1044303154654358 ) ) ;
#25673 = DIRECTION ( 'NONE',  ( -0.000000000000000000, 1.000000000000000000, -0.000000000000000000 ) ) ;
#25674 = CARTESIAN_POINT ( 'NONE',  ( 794.9819416627830151, -420.9982390220555999, 319.9864689768909898 ) ) ;
#25675 = CARTESIAN_POINT ( 'NONE',  ( 804.6971507214547046, -195.2817908451528410, 344.0799538623459739 ) ) ;
#25676 = CARTESIAN_POINT ( 'NONE',  ( 802.2119215644370342, -78.00906357242591582, -367.5423716828165084 ) ) ;
#25677 = CARTESIAN_POINT ( 'NONE',  ( 758.6633372737375112, -116.5328690171418202, -326.9102291470432533 ) ) ;
#25678 = CARTESIAN_POINT ( 'NONE',  ( 773.7943932421234194, -95.80559628986917176, 305.5313806188329409 ) ) ;
#25679 = CARTESIAN_POINT ( 'NONE',  ( 804.6798772138710092, -423.7255117493282341, 334.6312213355106451 ) ) ;
#25680 = VECTOR ( 'NONE', #16888, 1000.000000000000000 ) ;
#25681 = CARTESIAN_POINT ( 'NONE',  ( 805.9055244015594326, -171.6237781080507432, 315.8990559732753240 ) ) ;
#25682 = CARTESIAN_POINT ( 'NONE',  ( 791.9812246680005501, -20.63460265842048003, -361.9419747391813189 ) ) ;
#25683 = CARTESIAN_POINT ( 'NONE',  ( 783.0433043558608688, -120.8965053807781800, -315.1538015810313027 ) ) ;
#25684 = CARTESIAN_POINT ( 'NONE',  ( 774.6858677611749044, -105.7255117493293000, -315.5713283507209894 ) ) ;
#25685 = CARTESIAN_POINT ( 'NONE',  ( 795.9930595647434757, -435.0783235625953580, -320.7433823573372820 ) ) ;
#25687 = CARTESIAN_POINT ( 'NONE',  ( 800.0135310231082713, -278.0891481129651197, 325.0180583372163028 ) ) ;
#25686 = CARTESIAN_POINT ( 'NONE',  ( 791.9812246680005501, -260.6346026584197375, 361.9419747391813189 ) ) ;
#25688 = CARTESIAN_POINT ( 'NONE',  ( -928.0249999999991815, 154.9999999999998863, -360.0000000000000000 ) ) ;
#25689 = ORIENTED_EDGE ( 'NONE', *, *, #22659, .T. ) ;
#25690 = CARTESIAN_POINT ( 'NONE',  ( 775.9200461376533440, 24.19440371013046231, 315.3028492785443291 ) ) ;
#25691 = VERTEX_POINT ( 'NONE', #4800 ) ;
#25692 =( NAMED_UNIT ( * ) PLANE_ANGLE_UNIT ( ) SI_UNIT ( $, .RADIAN. ) );
#25693 = CARTESIAN_POINT ( 'NONE',  ( 772.4837098697145166, -191.3618753856926276, 374.5518280994205611 ) ) ;
#25694 = CARTESIAN_POINT ( 'NONE',  ( 804.1105419155481968, -267.8272453906071746, 347.6308680596136469 ) ) ;
#25695 = CARTESIAN_POINT ( 'NONE',  ( 756.1348686366196716, -377.2601417444137724, 347.5531968255698416 ) ) ;
#25696 = ORIENTED_EDGE ( 'NONE', *, *, #4683, .T. ) ;
#25697 = CARTESIAN_POINT ( 'NONE',  ( 796.1575198192839480, -78.00906357242591582, -359.4546378042384163 ) ) ;
#25698 = CARTESIAN_POINT ( 'NONE',  ( 791.1614460488616487, -203.2601417444143124, 373.5763878283158874 ) ) ;
#25699 = CARTESIAN_POINT ( 'NONE',  ( 755.5713283507202505, -269.3618753856924286, -334.6858677611754729 ) ) ;
#25700 = ORIENTED_EDGE ( 'NONE', *, *, #26355, .T. ) ;
#25701 = CARTESIAN_POINT ( 'NONE',  ( 774.6858677611749044, -393.7255117493283478, -315.5713283507209894 ) ) ;
#25702 = CARTESIAN_POINT ( 'NONE',  ( 771.1735550268778070, -33.18005720387498769, -316.3353852180827630 ) ) ;
#25703 = CARTESIAN_POINT ( 'NONE',  ( 784.0799538623451781, -251.8055962898686744, 364.6971507214555572 ) ) ;
#25704 = FACE_OUTER_BOUND ( 'NONE', #9822, .T. ) ;
#25705 = DIRECTION ( 'NONE',  ( 0.000000000000000000, 0.000000000000000000, -1.000000000000000000 ) ) ;
#25706 = CARTESIAN_POINT ( 'NONE',  ( 745.1792804349281596, -14.19088175424431242, -343.7566961878542884 ) ) ;
#25707 = DIRECTION ( 'NONE',  ( 0.000000000000000000, 0.000000000000000000, -1.000000000000000000 ) ) ;
#25708 = ORIENTED_EDGE ( 'NONE', *, *, #36696, .T. ) ;
#25709 = CARTESIAN_POINT ( 'NONE',  ( 746.4236121716829757, -303.8272453906071178, -328.8385539511384650 ) ) ;
#25710 = CARTESIAN_POINT ( 'NONE',  ( 745.1792804349281596, -158.1908817542438612, 343.7566961878542884 ) ) ;
#25711 = AXIS2_PLACEMENT_3D ( 'NONE', #21183, #32492, #1065 ) ;
#25713 = CARTESIAN_POINT ( 'NONE',  ( 767.8955696845333705, -240.4527844766015221, -362.1676090361162323 ) ) ;
#25712 = CARTESIAN_POINT ( 'NONE',  ( -879.9999999999992042, 430.0000000000002842, -244.9999999999999716 ) ) ;
#25714 = PRESENTATION_STYLE_ASSIGNMENT (( #20420 ) ) ;
#25715 = CARTESIAN_POINT ( 'NONE',  ( 755.3028492785439312, -159.2817908451529547, -335.9200461376539693 ) ) ;
#25716 = CARTESIAN_POINT ( 'NONE',  ( 759.0252816721024374, -24.99823902205683268, 368.0189434323527280 ) ) ;
#25717 = FACE_OUTER_BOUND ( 'NONE', #25837, .T. ) ;
#25718 = CARTESIAN_POINT ( 'NONE',  ( 773.7943932421234194, -23.80559628986938847, -305.5313806188329409 ) ) ;
#25719 = CARTESIAN_POINT ( 'NONE',  ( 792.3570229623691148, -357.1800572038739574, -373.1304606946836770 ) ) ;
#25720 = CARTESIAN_POINT ( 'NONE',  ( 265.7583438952258916, 430.0000000000002842, -320.0000000000000000 ) ) ;
#25721 = CARTESIAN_POINT ( 'NONE',  ( 755.3201227861273992, -27.72551174932954510, 345.3687786644892981 ) ) ;
#25722 = CARTESIAN_POINT ( 'NONE',  ( 762.1177392798416577, -282.5545181178798657, 309.8865473780659272 ) ) ;
#25723 = CARTESIAN_POINT ( 'NONE',  ( 811.6461892240364477, -220.7146871989596661, -324.1737431748509835 ) ) ;
#25724 = CARTESIAN_POINT ( 'NONE',  ( 745.4481719005789273, -219.7255117493289447, 347.5162901302853129 ) ) ;
#25725 = CARTESIAN_POINT ( 'NONE',  ( 777.4774526936600978, 13.72903370521577138, -304.7301800767027657 ) ) ;
#25726 = DIRECTION ( 'NONE',  ( -0.000000000000000000, 1.000000000000000000, -0.000000000000000000 ) ) ;
#25727 = ORIENTED_EDGE ( 'NONE', *, *, #4581, .F. ) ;
#25728 = CARTESIAN_POINT ( 'NONE',  ( 762.1405469898971887, -337.5436935675102177, 357.8594530101015607 ) ) ;
#25729 = CARTESIAN_POINT ( 'NONE',  ( 793.9708237608222134, -70.91815448151683654, 319.2295555964448681 ) ) ;
#25730 = CARTESIAN_POINT ( 'NONE',  ( 804.9511171171677688, -29.80559628986937781, -335.8780910478229202 ) ) ;
#25731 = DIRECTION ( 'NONE',  ( -1.000000000000000000, -0.000000000000000000, -0.000000000000000000 ) ) ;
#25732 = CARTESIAN_POINT ( 'NONE',  ( -2.174186756557595869E-13, 469.9999999999994884, 0.000000000000000000 ) ) ;
#25734 = CARTESIAN_POINT ( 'NONE',  ( 804.9363028652555840, -352.2709662947830225, 338.2165204200192079 ) ) ;
#25733 = CARTESIAN_POINT ( 'NONE',  ( 775.9200461376533440, -167.8055962898689586, 315.3028492785443291 ) ) ;
#25735 = ORIENTED_EDGE ( 'NONE', *, *, #43262, .T. ) ;
#25736 = CARTESIAN_POINT ( 'NONE',  ( 795.9930595647434757, -291.0783235625957559, -320.7433823573372820 ) ) ;
#25737 = CARTESIAN_POINT ( 'NONE',  ( 774.6858677611749044, -153.7255117493291721, 315.5713283507209894 ) ) ;
#25738 = CARTESIAN_POINT ( 'NONE',  ( 815.1787889125755555, -318.8965053807775121, -343.7953271457877804 ) ) ;
#25739 = FACE_BOUND ( 'NONE', #31660, .T. ) ;
#25740 = CARTESIAN_POINT ( 'NONE',  ( 777.4774526936600978, 13.72903370521577138, 304.7301800767027657 ) ) ;
#25741 = ORIENTED_EDGE ( 'NONE', *, *, #13502, .T. ) ;
#25742 = CARTESIAN_POINT ( 'NONE',  ( 774.6858677611749044, -321.7255117493286320, 315.5713283507209894 ) ) ;
#25743 = CIRCLE ( 'NONE', #11019, 8.024999999999948841 ) ;
#25744 = CARTESIAN_POINT ( 'NONE',  ( 760.5453621957607311, -93.07832356259645223, -323.8424801807151425 ) ) ;
#25745 = ORIENTED_EDGE ( 'NONE', *, *, #29246, .F. ) ;
#25746 = CARTESIAN_POINT ( 'NONE',  ( 754.8072714833581358, -436.8164208402372992, 338.1981804954720587 ) ) ;
#25747 = EDGE_CURVE ( 'NONE', #17477, #928, #21909, .T. ) ;
#25748 = CARTESIAN_POINT ( 'NONE',  ( 758.8095938919642549, -200.0891481129653187, -311.6929314249763365 ) ) ;
#25749 = EDGE_LOOP ( 'NONE', ( #41901, #44417, #7289, #1458 ) ) ;
#25750 = CARTESIAN_POINT ( 'NONE',  ( 795.1360043628808398, -140.0891481129655176, -360.2193346964456282 ) ) ;
#25751 = ORIENTED_EDGE ( 'NONE', *, *, #12005, .T. ) ;
#25752 = CARTESIAN_POINT ( 'NONE',  ( 804.4086373105744769, -409.6454272087884760, -333.3843516231986541 ) ) ;
#25753 = CARTESIAN_POINT ( 'NONE',  ( 759.9864689768902508, -2.089148112965993231, 354.9819416627836404 ) ) ;
#25754 = CARTESIAN_POINT ( 'NONE',  ( 796.7737145352015204, -236.6346026584198228, 370.7187646348536987 ) ) ;
#25755 = CARTESIAN_POINT ( 'NONE',  ( 770.0799878456142551, -157.9874144716871456, 362.9823548866085616 ) ) ;
#25757 = DIRECTION ( 'NONE',  ( 0.000000000000000000, -6.938893903907241197E-16, 1.000000000000000000 ) ) ;
#25756 = CARTESIAN_POINT ( 'NONE',  ( 775.4999999999993179, -513.1383975375929367, -349.9999999999999432 ) ) ;
#25758 = VERTEX_POINT ( 'NONE', #25602 ) ;
#25759 = CARTESIAN_POINT ( 'NONE',  ( 802.5472867521000353, -388.3726999360613945, -350.8726784830461156 ) ) ;
#25760 = CARTESIAN_POINT ( 'NONE',  ( 786.4999999999993179, -513.1383975375929367, -369.9999999999999432 ) ) ;
#25761 = CARTESIAN_POINT ( 'NONE',  ( 766.4474001241216001, -211.0999726633346540, -307.3154664389482491 ) ) ;
#25762 = CARTESIAN_POINT ( 'NONE',  ( 788.6739635108323228, -55.64542720878963422, 373.9316612368139090 ) ) ;
#25764 = DIRECTION ( 'NONE',  ( 1.000000000000000000, 0.000000000000000000, 0.000000000000000000 ) ) ;
#25763 = DIRECTION ( 'NONE',  ( -0.000000000000000000, 1.000000000000000000, -0.000000000000000000 ) ) ;
#25765 = CARTESIAN_POINT ( 'NONE',  ( 769.1273215169530886, -310.7146871989593251, -317.4527132478988847 ) ) ;
#25766 = CARTESIAN_POINT ( 'NONE',  ( 831.1634899080286232, 256.4999999999998863, -199.9999999999999432 ) ) ;
#25767 = CARTESIAN_POINT ( 'NONE',  ( 754.3581564841646241, -185.4636090269710280, -316.1443688327762516 ) ) ;
#25768 = DIRECTION ( 'NONE',  ( 0.000000000000000000, 0.000000000000000000, -1.000000000000000000 ) ) ;
#25769 = FACE_BOUND ( 'NONE', #45695, .T. ) ;
#25770 = CARTESIAN_POINT ( 'NONE',  ( 804.8461984189677878, -386.1908817542432075, 336.9566956441385628 ) ) ;
#25771 = CARTESIAN_POINT ( 'NONE',  ( 772.5602148656447525, -249.7255117493288594, -305.7998596910095443 ) ) ;
#25772 = DIRECTION ( 'NONE',  ( 1.000000000000000000, 0.000000000000000000, 0.000000000000000000 ) ) ;
#25773 = CARTESIAN_POINT ( 'NONE',  ( 755.5713283507202505, -5.361875385693257279, -334.6858677611754729 ) ) ;
#25774 = CIRCLE ( 'NONE', #19122, 10.00000000000000888 ) ;
#25775 = CARTESIAN_POINT ( 'NONE',  ( 776.2046728542105711, -164.1908817542438612, 304.8212110874238761 ) ) ;
#25776 = CARTESIAN_POINT ( 'NONE',  ( 773.7943932421234194, -143.8055962898690154, -305.5313806188329409 ) ) ;
#25777 = CARTESIAN_POINT ( 'NONE',  ( 777.4774526936600978, -130.2709662947837899, 304.7301800767027657 ) ) ;
#25778 = CARTESIAN_POINT ( 'NONE',  ( 759.0252816721024374, -360.9982390220557704, -368.0189434323527280 ) ) ;
#25779 = DIRECTION ( 'NONE',  ( 0.000000000000000000, 0.000000000000000000, -1.000000000000000000 ) ) ;
#25780 = PLANE ( 'NONE',  #4326 ) ;
#25781 = CARTESIAN_POINT ( 'NONE',  ( 756.3353852180819104, -221.9073299311470464, 331.1735550268788302 ) ) ;
#25782 = CARTESIAN_POINT ( 'NONE',  ( 802.5472867521000353, -28.37269993606244967, 350.8726784830461156 ) ) ;
#25783 = CARTESIAN_POINT ( 'NONE',  ( 773.7305795820266212, -9.281790845153418346, -374.8230680027170365 ) ) ;
#25784 = FACE_OUTER_BOUND ( 'NONE', #44600, .T. ) ;
#25785 = CARTESIAN_POINT ( 'NONE',  ( 771.2368401574024119, -37.44195992623299674, 374.2805881961240857 ) ) ;
#25786 = ORIENTED_EDGE ( 'NONE', *, *, #4581, .T. ) ;
#25787 = EDGE_CURVE ( 'NONE', #4037, #12675, #29295, .T. ) ;
#25788 = CARTESIAN_POINT ( 'NONE',  ( 796.7845633553578182, -201.6237781080506863, -358.5707757039688204 ) ) ;
#25789 = CARTESIAN_POINT ( 'NONE',  ( 800.0135310231082713, -14.08914811296595460, 325.0180583372163028 ) ) ;
#25790 = CARTESIAN_POINT ( 'NONE',  ( 783.7566961878529810, -240.8965053807777963, -305.1792804349288417 ) ) ;
#25791 = CARTESIAN_POINT ( 'NONE',  ( 749.8865473780648472, -332.5328690171411381, 322.1177392798429082 ) ) ;
#25792 = ORIENTED_EDGE ( 'NONE', *, *, #19317, .T. ) ;
#25793 = EDGE_CURVE ( 'NONE', #11392, #37728, #35995, .T. ) ;
#25794 = CARTESIAN_POINT ( 'NONE',  ( 797.6776695296629214, -331.5436935675104451, 357.6776695296636603 ) ) ;
#25795 = EDGE_CURVE ( 'NONE', #69, #27963, #27070, .T. ) ;
#25796 = CARTESIAN_POINT ( 'NONE',  ( 777.4774526936600978, -58.27096629478398171, -304.7301800767027657 ) ) ;
#25797 = CARTESIAN_POINT ( 'NONE',  ( 764.0069404352550464, -87.07832356259646645, 359.2566176426627180 ) ) ;
#25798 = EDGE_LOOP ( 'NONE', ( #18713, #43964 ) ) ;
#25799 = CARTESIAN_POINT ( 'NONE',  ( 776.2046728542105711, -452.1908817542428665, -304.8212110874238761 ) ) ;
#25800 = ORIENTED_EDGE ( 'NONE', *, *, #11114, .T. ) ;
#25801 = CARTESIAN_POINT ( 'NONE',  ( 780.5236548040995785, -308.7363362996979390, -314.9735926884559944 ) ) ;
#25803 = CARTESIAN_POINT ( 'NONE',  ( 793.9708237608222134, -382.9181544815159555, 319.2295555964448681 ) ) ;
#25802 = CARTESIAN_POINT ( 'NONE',  ( 765.0180583372156207, -72.99823902205667991, 360.0135310231089534 ) ) ;
#25804 = CARTESIAN_POINT ( 'NONE',  ( 755.3201227861273992, -291.7255117493285752, -345.3687786644892981 ) ) ;
#25806 = CARTESIAN_POINT ( 'NONE',  ( 758.0141637701419768, -327.0783235625956991, 367.2620300519063790 ) ) ;
#25805 = CARTESIAN_POINT ( 'NONE',  ( 751.9810565676468741, -410.0891481129647218, 360.9747183278973921 ) ) ;
#25807 = CARTESIAN_POINT ( 'NONE',  ( 787.5531968255692163, -285.8272453906071178, -316.1348686366205811 ) ) ;
#25808 = CARTESIAN_POINT ( 'NONE',  ( 768.0187753319979720, -296.6346026584195670, -318.0580252608186242 ) ) ;
#25809 = FACE_BOUND ( 'NONE', #16881, .T. ) ;
#25810 = CARTESIAN_POINT ( 'NONE',  ( 792.1044303154645831, -156.4527844766018916, -317.8323909638837677 ) ) ;
#25811 = EDGE_CURVE ( 'NONE', #28460, #13538, #42692, .T. ) ;
#25812 = CARTESIAN_POINT ( 'NONE',  ( 759.0252816721024374, -408.9982390220556567, 368.0189434323527280 ) ) ;
#25814 = CARTESIAN_POINT ( 'NONE',  ( -26.63011601220122060, 22.32581219114657856, 895.6886905569881492 ) ) ;
#25813 = CARTESIAN_POINT ( 'NONE',  ( 911.9749999999993406, 219.9999999999998863, -360.0000000000000000 ) ) ;
#25815 = EDGE_CURVE ( 'NONE', #28192, #20456, #8502, .T. ) ;
#25816 = CARTESIAN_POINT ( 'NONE',  ( 749.5768839229115201, -84.55451811788046257, -358.0661480581553064 ) ) ;
#25817 = CARTESIAN_POINT ( 'NONE',  ( 989.9999999999992042, 249.9999999999998863, 360.0000000000000000 ) ) ;
#25818 = DIRECTION ( 'NONE',  ( 1.000000000000000000, 0.000000000000000000, 0.000000000000000000 ) ) ;
#25819 = CARTESIAN_POINT ( 'NONE',  ( 790.9844846989617508, -286.3726999360617356, 317.2208543904092721 ) ) ;
#25820 = CARTESIAN_POINT ( 'NONE',  ( 754.8072714833581358, -148.8164208402382656, 338.1981804954720587 ) ) ;
#25821 = ORIENTED_EDGE ( 'NONE', *, *, #43619, .F. ) ;
#25822 = CARTESIAN_POINT ( 'NONE',  ( 751.6929314249750860, -126.9982390220565094, -318.8095938919659034 ) ) ;
#25823 = CARTESIAN_POINT ( 'NONE',  ( 758.6633372737375112, -332.5328690171411381, 326.9102291470432533 ) ) ;
#25824 = PLANE ( 'NONE',  #14578 ) ;
#25825 = CARTESIAN_POINT ( 'NONE',  ( 766.7756240680305382, -422.5328690171408539, -361.5560724626415663 ) ) ;
#25826 = CARTESIAN_POINT ( 'NONE',  ( 744.6391490659812007, -62.73633629969871350, 338.7502325331110455 ) ) ;
#25827 = CARTESIAN_POINT ( 'NONE',  ( 746.8695393053150156, -269.9073299311468190, -327.6429770376306010 ) ) ;
#25828 = CARTESIAN_POINT ( 'NONE',  ( 814.9108240113580450, -208.2709662947835341, 337.5031285880265273 ) ) ;
#25829 = CARTESIAN_POINT ( 'NONE',  ( 768.0187753319979720, -104.6346026584202207, 318.0580252608186242 ) ) ;
#25830 = ORIENTED_EDGE ( 'NONE', *, *, #12787, .F. ) ;
#25831 = CARTESIAN_POINT ( 'NONE',  ( 801.9858362298568863, -315.0783235625957559, -312.7379699480935642 ) ) ;
#25832 = EDGE_CURVE ( 'NONE', #36800, #14626, #24139, .T. ) ;
#25833 = CARTESIAN_POINT ( 'NONE',  ( 804.4086373105744769, -1.645427208789804308, 333.3843516231986541 ) ) ;
#25834 = CARTESIAN_POINT ( 'NONE',  ( 745.4481719005789273, -339.7255117493285184, -347.5162901302853129 ) ) ;
#25835 = DIRECTION ( 'NONE',  ( 0.000000000000000000, 0.000000000000000000, -1.000000000000000000 ) ) ;
#25836 = CARTESIAN_POINT ( 'NONE',  ( 756.1348686366196716, -401.2601417444137155, 347.5531968255698416 ) ) ;
#25837 = EDGE_LOOP ( 'NONE', ( #2029, #9501, #29733, #5439 ) ) ;
#25838 = CARTESIAN_POINT ( 'NONE',  ( 755.0636971347428243, -412.2709662947829088, -341.7834795799807353 ) ) ;
#25839 = EDGE_CURVE ( 'NONE', #19255, #8608, #15218, .T. ) ;
#25840 = CARTESIAN_POINT ( 'NONE',  ( 759.9864689768902508, -218.0891481129653187, -354.9819416627836404 ) ) ;
#25841 = CARTESIAN_POINT ( 'NONE',  ( 749.8865473780648472, -116.5328690171418202, -322.1177392798429082 ) ) ;
#25842 = LINE ( 'NONE', #24517, #37345 ) ;
#25843 = CARTESIAN_POINT ( 'NONE',  ( 795.6651683502461765, -250.7146871989595809, 371.3240766477733814 ) ) ;
#25844 = CARTESIAN_POINT ( 'NONE',  ( 800.0135310231082713, -62.08914811296580183, 325.0180583372163028 ) ) ;
#25845 = ORIENTED_EDGE ( 'NONE', *, *, #4114, .F. ) ;
#25846 = CARTESIAN_POINT ( 'NONE',  ( 754.8983024940795303, -234.8965053807777963, -336.9254006560228163 ) ) ;
#25847 = EDGE_CURVE ( 'NONE', #11392, #42107, #1729, .T. ) ;
#25848 = CARTESIAN_POINT ( 'NONE',  ( 795.1360043628807261, -236.0891481129651766, 360.2193346964456282 ) ) ;
#25849 = EDGE_CURVE ( 'NONE', #23261, #35455, #7590, .T. ) ;
#25850 = CARTESIAN_POINT ( 'NONE',  ( 813.2346286133761168, -53.26014174441475291, -328.9521613784389160 ) ) ;
#25851 = LINE ( 'NONE', #35554, #19496 ) ;
#25852 = ORIENTED_EDGE ( 'NONE', *, *, #27824, .F. ) ;
#25853 = ORIENTED_EDGE ( 'NONE', *, *, #3316, .F. ) ;
#25854 = CARTESIAN_POINT ( 'NONE',  ( 799.9636004259356241, -334.9181544815160692, -311.2241431872006956 ) ) ;
#25855 = CARTESIAN_POINT ( 'NONE',  ( 772.5602148656447525, -273.7255117493288026, 305.7998596910095443 ) ) ;
#25856 = CARTESIAN_POINT ( 'NONE',  ( 808.7758568127978833, -28.16923265350574468, 320.0363995740631822 ) ) ;
#25857 = CARTESIAN_POINT ( 'NONE',  ( 754.7162404726377645, -182.7363362996983369, -339.4709603349214717 ) ) ;
#25858 = CARTESIAN_POINT ( 'NONE',  ( 767.8955696845333705, -192.4527844766016926, -362.1676090361162323 ) ) ;
#25859 = CARTESIAN_POINT ( 'NONE',  ( 781.7834795799800531, -370.8164208402375834, -315.0636971347436202 ) ) ;
#25860 = ORIENTED_EDGE ( 'NONE', *, *, #2744, .F. ) ;
#25861 = CARTESIAN_POINT ( 'NONE',  ( 790.8050863131179540, -452.8379544210779954, -362.5841948692291226 ) ) ;
#25862 = VERTEX_POINT ( 'NONE', #5707 ) ;
#25863 = CARTESIAN_POINT ( 'NONE',  ( 779.9999999999992042, -452.9681489794448339, -339.9999999999999432 ) ) ;
#25864 = CARTESIAN_POINT ( 'NONE',  ( 939.9999999999993179, -600.0000000000001137, 360.0000000000000000 ) ) ;
#25865 = CARTESIAN_POINT ( 'NONE',  ( 779.4763451958990572, -200.7363362996982801, 365.0264073115438919 ) ) ;
#25866 = CARTESIAN_POINT ( 'NONE',  ( 768.0187753319979720, -32.63460265842044095, 318.0580252608186242 ) ) ;
#25867 = ORIENTED_EDGE ( 'NONE', *, *, #16989, .T. ) ;
#25868 = CARTESIAN_POINT ( 'NONE',  ( 748.6759233522253680, -424.3726999360612808, -324.3348316497537098 ) ) ;
#25869 = CARTESIAN_POINT ( 'NONE',  ( 748.9653473494365699, -26.63460265842046226, -356.9462024416520762 ) ) ;
#25870 = CARTESIAN_POINT ( 'NONE',  ( 801.3366627262608972, -224.5328690171415076, 353.0897708529566899 ) ) ;
#25871 = CARTESIAN_POINT ( 'NONE',  ( 759.9864689768902508, -386.0891481129647786, -354.9819416627836404 ) ) ;
#25872 = CARTESIAN_POINT ( 'NONE',  ( 804.9363028652555840, 7.729033705215793582, -338.2165204200192079 ) ) ;
#25873 = CARTESIAN_POINT ( 'NONE',  ( 814.5518280994195948, -423.7255117493281205, 332.4837098697145734 ) ) ;
#25874 = CARTESIAN_POINT ( 'NONE',  ( 441.1634899080286232, 240.0000000000000000, -199.9999999999972431 ) ) ;
#25875 = CARTESIAN_POINT ( 'NONE',  ( 784.1219089521767955, -261.2817908451526705, -315.0488828828318333 ) ) ;
#25876 = CARTESIAN_POINT ( 'NONE',  ( 792.2312462859673587, -179.9073299311472454, -307.2067596250082602 ) ) ;
#25877 = CARTESIAN_POINT ( 'NONE',  ( 796.9462024416508257, -60.45278447660215448, 308.9653473494370246 ) ) ;
#25878 = CARTESIAN_POINT ( 'NONE',  ( 772.4837098697144029, -95.36187538569294020, 374.5518280994205611 ) ) ;
#25879 = CARTESIAN_POINT ( 'NONE',  ( -28.63011601220122415, -355.4967352946684969, -16.45562775363623587 ) ) ;
#25880 = CARTESIAN_POINT ( 'NONE',  ( 791.0478386215596629, -381.8272453906068336, 306.7653713866226326 ) ) ;
#25881 = ADVANCED_FACE ( 'NONE', ( #41275 ), #5926, .F. ) ;
#25882 = DIRECTION ( 'NONE',  ( -1.000000000000000000, -0.000000000000000000, -0.000000000000000000 ) ) ;
#25883 = CARTESIAN_POINT ( 'NONE',  ( 811.0346526505616112, -350.6346026584192828, 323.0537975583477532 ) ) ;
#25884 = CARTESIAN_POINT ( 'NONE',  ( 792.1044303154645831, -300.4527844766012663, -317.8323909638837677 ) ) ;
#25885 = CARTESIAN_POINT ( 'NONE',  ( 783.0433043558608688, 23.10349461922137237, 315.1538015810313027 ) ) ;
#25886 = CARTESIAN_POINT ( 'NONE',  ( 745.5313806188320314, -63.28179084515324604, -333.7943932421247268 ) ) ;
#25887 = CARTESIAN_POINT ( 'NONE',  ( 798.7617431975189675, -123.6237781080508569, -323.0428371773161871 ) ) ;
#25888 = CARTESIAN_POINT ( 'NONE',  ( 795.6651683502461765, -130.7146871989599504, 371.3240766477733814 ) ) ;
#25889 = CARTESIAN_POINT ( 'NONE',  ( 803.6646147819162707, -449.9073299311464211, 348.8264449731211130 ) ) ;
#25890 =( BOUNDED_SURFACE ( )  B_SPLINE_SURFACE ( 3, 2, ( 
 ( #26594, #6034, #19441, #19908, #20354, #33984, #2336, #16436, #9516, #8834, #9047, #23116, #23582, #22902, #37687, #2572, #34450, #13217, #27294, #2813, #16904, #30985, #12308, #36993, #33535, #13661, #3034, #34677, #41846, #42284, #27743, #17122, #21270, #38596, #14118, #41606, #28425, #35570, #10646, #6722, #31207, #38846, #6502, #42064, #42524, #21037, #10413, #27968, #31437, #27508, #10190, #24266, #26, #13438, #20797, #35349, #10890, #38374, #3725, #7199, #31659, #45543, #17813, #28191, #34894, #3260, #17352, #13894, #20581, #24489, #6953, #24725, #35124, #31879, #38153, #3502, #21493, #17588, #251, #14348, #24957, #39071, #7419, #3947, #18042, #45082, #9963, #24033, #8325, #11797, #25866, #5084, #4194, #1389, #36052, #32585, #32361, #4856, #18287, #32122, #487, #28667, #927, #39976, #40200, #22625, #22389, #35815, #15493, #25414, #25177, #14594, #39534, #21966, #8561, #15031, #21722, #7891, #42745, #1163, #11107, #4414, #18506, #29119, #36493, #39288, #43202, #717, #11573, #14815, #43429, #18956, #12018, #15271, #25654, #39767, #29357, #28888, #4626, #8115, #42968, #22175, #33052, #32810, #36726, #36270, #11335, #29573, #18723, #43649, #26086, #7643, #37164, #5523, #16155, #19618, #33260, #33714, #1606, #40869, #40643, #15703, #33931, #19391, #12684, #26326, #2063, #44102, #30237, #36944, #23745, #12466, #44803, #9681, #44329, #2514, #43868, #26763, #9233, #37857, #23524, #30707, #23304, #33478, #16620, #26545, #8996, #22851, #13160, #5297, #41108, #37406, #27239, #5763, #19851, #2282, #41332, #16381, #1824, #29788, #37626, #23064, #19175, #12247, #40431, #30458, #44562, #12924, #15932, #27009, #9461, #5977, #30016, #20068, #34143, #8783, #3446, #17768, #31150, #45247, #27456, #30935, #24440, #17543, #35304, #20977, #17072, #21223, #24671, #45489, #20534, #42239, #7145, #38790, #2985, #17295, #28368, #9906, #31833, #10144, #2761, #3681, #38545, #31616, #28145, #204, #14296, #6897, #13383, #45719, #41794, #41553, #24219, #35074, #34390, #27924, #13607, #42470, #13846, #42019, #10836, #27690, #20749, #24908, #14072, #6206, #10365, #38327, #10595, #20299, #38100, #16855, #6673, #23979, #45029, #6455, #34840, #31385, #34628, #3204, #4366, #437, #11964, #43386, #7840, #36442, #36219, #4806, #18236, #32311, #14539, #17993, #11525, #4583, #22341, #8068, #4143, #8276, #11753, #32536, #7596, #29312, #39932, #25820, #35764, #18457, #15448, #42699, #18911, #42920, #35524, #33004, #25608, #18674, #15225, #1344, #29524, #39718, #28617, #32763, #28840, #11063, #11286, #22130, #21448, #14985, #667, #43598, #882, #29070, #39022, #14768, #21915, #7372, #1110, #3900, #43158, #25363, #32065, #25130, #39243, #21672, #39480, #36002, #44282, #12196, #33426, #5470, #40388, #8508, #33662, #1555, #26033, #44510, #40144, #44051, #22577, #2011, #1768, #36679, #40819, #26276, #16108, #15653, #8950, #15879, #30192, #8739, #22805, #9173, #5932, #36898, #23249, #9409, #37352, #5713, #19800, #33884, #12870, #37577, #2237, #16332, #34099, #26952, #41052, #43393, #28625, #8283, #19841, #37156, #9452, #40635, #44093, #26537, #23515, #12458, #43855, #12010, #2274, #36936, #27001, #20059, #5969, #5290, #19383, #8988, #15695, #5514, #23056, #19610, #26317, #33703, #37616, #12676, #30006, #2053, #40861, #8775, #16147, #33469, #12238, #1814, #16373, #44321, #34136, #30230, #22843, #37398, #26756, #5752, #15922, #1597, #9222, #33923, #30450, #44554, #41097, #2506, #16611, #29780, #43641, #26074, #40188, #8553, #36716, #5076, #19167, #33251, #34382, #24432, #37849, #27681, #28136, #6666, #41786, #13599, #17064, #13150, #13374, #27447, #31375, #44795, #38092, #6889, #42231, #2751, #35065, #38537, #17286, #31141, #20968, #45482, #30926, #45021, #16846, #20289, #6198, #6447, #41545, #13838, #38319, #27915, #23739, #9898, #7136, #23970, #20526, #3438, #20740, #34620, #45238, #10585, #2976, #17535, #10136, #24209, #31608, #10356, #45712, #3673, #34833, #14063, #3196, #42012, #24663, #38778, #21214, #30699, #27231, #41323, #35295, #9673, #28112, #41303, #45690, #20269, #14043, #6425, #9653, #34360, #31119, #2729, #39899, #36866, #37314, #30164, #19103, #16304, #30387, #6376, #41478, #20458, #6816, #2437, #45172, #20222, #13532, #6131, #27847, #24360, #34545, #27606, #2905, #44950, #45406, #16774, #34306, #38464, #41713, #17213, #44719, #31542, #38700, #41942, #9830, #2678, #10286, #9609, #10069, #45643, #24138, #38248, #31072, #16996, #30622, #30854, #13306, #3124, #16539, #23900, #20894, #13992, #27382, #34992, #3367, #34762, #6593, #17459, #31300, #38020, #20671, #28063, #37783, #23670, #42156, #10507, #24583, #7059, #21143, #41253, #13081, #27165, #38946, #31976, #11431, #11206, #39167, #4046, #15130, #28530, #7985, #347, #7296, #25516, #14905, #28987, #8197, #21371, #4504, #7517, #35671, #35447, #22051, #3817, #35226, #3604, #31751, #18145, #43068, #43299, #25742, #39630, #17908, #18596, #42625, #28280, #17691, #10986, #25055, #11666, #32224, #24826, #21590, #121, #4286, #14211, #584, #14685, #28762, #36142, #42380, #42842, #14450, #25278, #39389, #805, #32680, #29220, #18377, #7742, #21820, #32457, #35914, #1028, #39856, #10748, #12109, #26630, #22934, #30325, #26416, #33135, #1922, #22720, #30108, #15572, #25952, #40302, #36597, #40059, #44194, #15791, #37028, #18824, #5620, #12771, #19476, #29654, #8419, #16028, #29440, #19254, #19716, #43965, #33342, #5170, #8656, #4720, #4953, #19045, #5382, #36361, #43731, #12555, #33802, #22487, #40727, #9084, #8869, #36815, #23151, #33571, #1472, #26188, #1686, #11881, #43515, #29880, #12342, #37259, #40517, #2154, #15362, #16246, #44418, #26852, #40961, #22264, #32916, #1260, #23838, #34937, #2613, #27785, #20162, #27107, #31247, #34712, #3070, #28008, #41198, #24306, #13251, #37953, #9553, #41884, #23615, #9324, #23394, #5855, #6308, #17161, #17398, #45585, #45344, #13017, #38413, #16713, #2375, #37495, #30798, #44891, #31481, #20392, #44656, #27329, #19943, #24075, #34019, #41422, #34489, #2848, #13706, #16473, #16941, #37722, #31021, #6073, #20617, #10228, #3303, #38192, #45119, #13476, #6537, #34238, #27546, #41650, #10006, #6764, #20838, #13933, #30555, #528, #7242, #21764, #42570, #4235, #35389, #14158, #14390, #28469, #39110, #10931, #38887, #39329, #35613, #7930, #7460, #24999, #21533, #22000, #3986, #42323, #10453, #756, #3762, #25456, #18544, #4455, #17852, #31919, #18083, #28229, #32163, #14634, #28706, #24771, #42785, #11147, #39575, #7684, #36089, #21313, #290, #17633, #21085, #25217, #35858, #32623, #18327, #32407, #11373, #14854, #28931, #10688, #43010, #967, #15071, #42103, #24530, #38641, #7000, #35169, #3547, #31698, #12501, #1638, #26361, #5330, #23099, #26577, #15738, #36306, #22886, #18994, #18762, #1424, #12285, #11612, #5118, #8362, #19657 ),
 ( #2100, #33516, #43241, #15526, #25690, #19206, #4894, #39802, #43908, #29391, #22665, #4664, #29606, #22427, #43684, #1200, #33750, #36536, #9029, #29158, #26127, #40675, #8150, #12055, #33293, #22213, #1865, #37199, #40242, #43463, #5565, #33087, #8599, #32852, #15308, #11830, #19425, #25901, #36762, #29826, #40465, #8817, #40011, #36977, #15971, #30053, #44136, #9719, #30971, #12719, #45287, #6708, #13423, #23563, #19889, #9947, #23340, #13201, #13645, #37898, #27279, #44838, #2553, #44364, #44601, #12963, #16890, #30271, #37666, #38138, #27729, #33967, #20568, #24020, #2798, #16660, #6489, #45068, #16417, #30498, #2319, #5803, #37443, #6016, #27049, #27492, #23784, #41592, #9273, #41147, #38362, #9499, #20107, #34663, #6248, #34182, #30744, #41831, #41372, #3023, #20338, #34431, #17109, #31191, #10177, #34879, #24254, #20785, #16190, #26799, #40903, #21706, #21018, #21951, #17332, #45527, #17799, #28651, #11320, #39518, #42729, #6937, #18274, #42270, #42051, #3244, #10631, #38830, #25398, #3712, #38582, #24708, #31421, #18027, #27955, #7180, #21255, #35335, #7628, #13879, #236, #35108, #14332, #3484, #14576, #25164, #28872, #32105, #31865, #42508, #473, #31645, #21479, #28410, #17574, #10874, #35801, #3932, #7874, #7405, #14104, #11093, #24940, #39273, #39056, #4179, #32347, #42953, #702, #35557, #14798, #10399, #13, #24475, #28178, #18703, #4839, #1146, #16124, #9429, #5488, #40405, #12655, #40616, #37371, #36913, #19146, #5267, #19359, #44300, #19819, #33902, #16351, #1573, #30431, #44531, #12889, #23496, #29542, #37596, #5950, #33023, #1361, #15464, #43617, #40162, #11983, #26051, #25797, #34321, #44961, #9621, #5698, #2450, #16552, #20471, #19785, #30637, #45181, #17227, #41034, #27617, #31084, #34558, #23683, #13544, #2917, #23462, #37561, #26931, #12850, #44492, #44732, #9393, #41726, #13318, #24152, #27177, #41265, #45420, #37794, #38261, #6606, #31313, #27861, #41956, #23230, #3615, #28774, #21153, #28073, #32236, #35685, #4060, #28997, #42168, #25290, #14223, #10762, #10519, #42852, #24594, #10298, #24371, #6827, #24838, #18161, #18387, #816, #597, #14004, #39402, #17703, #3380, #38476, #31764, #134, #32467, #38958, #45654, #28292, #20907, #25065, #35003, #42392, #7308, #21385, #14698, #17472, #35458, #38712, #3831, #7073, #35237, #7753, #17920, #31990, #362, #11219, #14464, #31554, #28542, #42637, #10998, #21832, #14916, #39179, #35925, #7529, #4296, #21603, #36152, #43081, #4734, #32929, #19487, #43526, #32692, #18836, #11445, #12120, #22061, #1273, #36372, #15373, #1696, #25529, #40070, #15144, #8432, #1039, #8670, #19265, #22943, #26202, #29452, #36611, #40316, #25755, #15583, #11891, #11679, #25964, #15801, #43741, #5392, #1484, #8208, #22734, #22500, #5179, #4967, #29234, #19058, #33147, #29665, #36828, #39867, #33354, #22276, #43310, #29891, #43977, #12352, #39642, #26429, #33584, #40530, #8879, #37040, #1934, #4514, #16037, #7996, #18607, #41209, #13028, #16486, #12567, #12783, #26865, #30808, #44207, #37507, #6321, #27558, #2167, #34499, #23850, #16724, #30567, #20403, #44902, #30337, #44429, #33814, #19726, #5632, #5866, #16258, #13261, #37734, #27339, #23164, #40974, #6549, #9335, #23404, #2859, #6086, #34030, #44668, #10020, #19955, #16951, #2387, #27118, #31029, #9783, #37966, #3080, #9565, #41432, #23625, #20174, #45128, #34253, #13486, #26642, #41664, #20628, #24087, #2625, #38201, #34721, #37272, #30120, #40738, #9094, #28238, #75, #3559, #45359, #45597, #13944, #17863, #31258, #24539, #39123, #14646, #34947, #21544, #10943, #3773, #17647, #7474, #31931, #17413, #31493, #20849, #6773, #38422, #38652, #3317, #302, #24783, #14404, #10239, #28018, #39343, #42112, #10463, #35626, #38901, #21099, #31708, #42801, #7010, #3998, #35183, #14167, #18099, #42583, #25014, #35872, #42333, #32180, #10701, #7254, #21325, #542, #35402, #17171, #13720, #27799, #28483, #28722, #25233, #7696, #11161, #21778, #41894, #24318, #43024, #4248, #11625, #39815, #26376, #4680, #39588, #25703, #18338, #19006, #28944, #8161, #43254, #22224, #8614, #32419, #1213, #22011, #15321, #7944, #15537, #26144, #29840, #33098, #36319, #43475, #1436, #32637, #22444, #18777, #18556, #32867, #22680, #4908, #12301, #8377, #15085, #29618, #29403, #12069, #11843, #36102, #25914, #40024, #36551, #43696, #4466, #40259, #36776, #5132, #11386, #29172, #40479, #981, #19219, #33306, #1651, #15753, #43924, #8831, #22898, #768, #14868, #25470, #13213, #16673, #30759, #9959, #9044, #6262, #40919, #37457, #37215, #9731, #23113, #36990, #5344, #33531, #5818, #44851, #45078, #27504, #27290, #40689, #20349, #30285, #30070, #19438, #44378, #26814, #13434, #19904, #26591, #12734, #1879, #6030, #15990, #9286, #23355, #33981, #41384, #44151, #2332, #5581, #16432, #19672, #2567, #23797, #16900, #20122, #30513, #44615, #34198, #33766, #9512, #12979, #2116, #27067, #37909, #37681, #41603, #41161, #16205, #34445, #23577, #2809, #30981, #12517, #42061, #10410, #21032, #24486, #20794, #21267, #38371, #41842, #248, #17585, #38842, #20578, #7416, #14591, #35346, #31433, #27739, #17810, #31203, #35120, #21490, #23, #3498, #6949, #38593, #6499, #6719, #34891, #24722, #38149, #45540, #14344, #35567, #10187, #28422, #31876, #10642, #31656, #42520, #7194, #24263, #3256, #17346, #13657, #45299, #13891, #27965, #14115, #10886, #28188, #3722, #34674, #3944, #28663, #24953, #42281, #39068, #18038, #32119, #483, #42740, #24029, #3031, #17119, #43199, #39285, #39531, #32581, #11794, #25174, #25651, #29569, #22620, #28885, #26081, #40194, #8321, #39764, #36722, #5080, #11332, #8112, #14810, #713, #32358, #22172, #42965, #33256, #18720, #1602, #36266, #4621, #1160, #15267, #29354, #10651, #28431, #493, #3704, #24466, #10622, #6927, #7172, #21246, #28398, #32095, #32629, #10693, #28476, #25695, #14639, #25223, #39116, #39806, #7465, #38893, #28712, #42793, #12293, #23105, #5809, #33974, #37207, #1428, #12725, #36768, #36541, #43467, #5124, #33299, #19897, #43914, #33091, #19212, #11835, #12507, #22436, #1644, #15745, #29833, #2108, #25906, #40471, #15530, #8823, #29611, #9035, #19663, #23347, #26583, #26369, #36983, #40681, #26135, #15978, #22891, #12061, #5336, #16197, #44143, #2325, #1871, #8607, #5571, #19431, #33756, #33523, #43688, #30062, #30277, #44370, #26805, #40250, #40911, #9278, #37450, #16423, #40015, #22672, #8367, #4900, #18999, #6023, #37902, #20114, #45293, #38143, #13652, #23569, #41377, #6942, #34189, #27284, #6712, #6494, #34437, #45073, #10403, #23790, #3248, #9726, #2560, #20789, #10182, #24258, #3490, #16665, #45532, #2803, #30975, #30750, #17340, #44844, #30505, #44608, #27058, #13428, #38366, #38586, #21025, #34884, #13206, #13884, #6256, #37674, #12969, #20343, #16894, #35113, #27498, #41597, #9954 ),
 ( #31426, #31195, #41154, #34668, #24024, #27959, #20572, #42055, #3027, #17114, #27733, #41836, #24480, #9505, #14336, #14802, #31869, #35339, #39523, #11097, #32351, #14107, #915, #8102, #28876, #24945, #21260, #11323, #24715, #14581, #15017, #39276, #28655, #476, #3935, #16, #239, #28414, #18277, #31648, #39060, #7878, #29106, #3715, #21954, #25401, #21482, #28181, #43190, #35806, #42956, #36040, #11559, #25641, #4182, #38833, #4403, #7408, #7186, #35560, #705, #42273, #7631, #42512, #22164, #25167, #21709, #36253, #18030, #32111, #39754, #18493, #17578, #32570, #42733, #10634, #17802, #10877, #1810, #15481, #39966, #22837, #36480, #43635, #29772, #18944, #32797, #15690, #11785, #23292, #8982, #18707, #22611, #1151, #26312, #26068, #15256, #19378, #4844, #43850, #25856, #36711, #29561, #5071, #22375, #9217, #12004, #30225, #40854, #1591, #33698, #29345, #33246, #40418, #4611, #23051, #16142, #19162, #33040, #2048, #40182, #8547, #8311, #44316, #1378, #26532, #12233, #12671, #8770, #36931, #5285, #26751, #33462, #15917, #43418, #37149, #30001, #44087, #12453, #40630, #5509, #19605, #30921, #30695, #45017, #13370, #27676, #10131, #20734, #26996, #21902, #21660, #35986, #3668, #17755, #45708, #3433, #42684, #35750, #7823, #39230, #35290, #39463, #42906, #17980, #38773, #28826, #25349, #11273, #21209, #35511, #868, #28131, #4351, #14059, #17530, #11051, #4129, #18442, #7583, #31819, #32520, #14971, #32050, #7131, #29056, #43142, #24427, #190, #3886, #38530, #10579, #6884, #28351, #20961, #35059, #25116, #18221, #651, #31603, #24656, #32296, #14282, #42454, #10822, #24894, #39008, #7359, #21435, #421, #14526, #28602, #19118, #33207, #16095, #32991, #26019, #5456, #12182, #30179, #1544, #29511, #1757, #15865, #43373, #8728, #4792, #1096, #29722, #11739, #1329, #36668, #8262, #22116, #22564, #32749, #15210, #44038, #29298, #43583, #11951, #15639, #5028, #43800, #40377, #22793, #36888, #5240, #19330, #33413, #12408, #26488, #40589, #8935, #19551, #33647, #44739, #38036, #37340, #23687, #37798, #45185, #27397, #20476, #6147, #12856, #34563, #9398, #16792, #19789, #2921, #16320, #41492, #44270, #5702, #19246, #40291, #22708, #19705, #33333, #8409, #22253, #44182, #29644, #16236, #36351, #32903, #12100, #37018, #5373, #11871, #1910, #16018, #26620, #22477, #15351, #43504, #24296, #17150, #38402, #44880, #41412, #37940, #30546, #6297, #16931, #27535, #41637, #37712, #6752, #41188, #27097, #3291, #17386, #26842, #19934, #40951, #2363, #16463, #9542, #17618, #21752, #21072, #24988, #39565, #32153, #7448, #21523, #14378, #24518, #42312, #38875, #39317, #38628, #17841, #32396, #18533, #53, #14845, #28920, #3534, #7231, #31908, #29816, #1191, #25891, #8352, #36523, #33076, #26117, #40231, #12275, #22654, #36967, #39793, #36752, #5555, #5321, #33506, #15962, #30044, #19648, #43231, #25681, #8141, #20559, #27039, #5794, #3013, #13413, #45276, #2091, #16408, #13635, #6004, #34172, #20097, #27718, #13189, #41361, #37886, #6237, #34420, #38353, #2788, #16880, #30560, #3309, #32174, #3554, #10233, #3075, #17639, #31703, #25226, #70, #17405, #38895, #17167, #31925, #27792, #7249, #297, #14397, #537, #31252, #42578, #45590, #25008, #13938, #28715, #42796, #11156, #39338, #45353, #13714, #28013, #18550, #8370, #43249, #4461, #25698, #40853, #36544, #44547, #40019, #975, #16141, #36313, #44315, #18772, #25909, #26995, #9216, #2269, #22219, #32632, #33918, #29165, #11620, #39582, #16366, #22006, #12670, #29398, #30445, #32858, #4674, #1208, #12908, #15316, #36096, #4243, #23291, #39809, #19835, #41092, #9447, #8156, #43470, #11838, #7939, #22439, #5508, #19604, #15078, #33697, #2046, #35866, #30224, #18333, #26750, #37392, #11381, #14863, #5747, #32413, #762, #28939, #43016, #25463, #42007, #17058, #37845, #13833, #24425, #10350, #20285, #34614, #45707, #27227, #3432, #27441, #20054, #6883, #41781, #20733, #45477, #17529, #20959, #10130, #30694, #17278, #13369, #13146, #41540, #6660, #5965, #45232, #2747, #14058, #31135, #13593, #28129, #30920, #38087, #31602, #24204, #42225, #27675, #9891, #27910, #38529, #9668, #34827, #34378, #41319, #38313, #23734, #16842, #2970, #6193, #34132, #3191, #44791, #23511, #35058, #37611, #23965, #2500, #31369, #45016, #16607, #6442, #20521, #4127, #17754, #42683, #35510, #11050, #28350, #15209, #3885, #36204, #1095, #7582, #39703, #35289, #7130, #8051, #28825, #7821, #32519, #4568, #22115, #42905, #31818, #4350, #420, #188, #28601, #21900, #38772, #32295, #17978, #29297, #18220, #650, #10578, #32048, #25115, #18659, #11272, #24655, #14752, #39229, #867, #14970, #42453, #35985, #21434, #14280, #25348, #10821, #14525, #35747, #24893, #21208, #21659, #39007, #3667, #29055, #7358, #18441, #43141, #11508, #25593, #32748, #12407, #43582, #36887, #4791, #29721, #22563, #43799, #15432, #2225, #36667, #23233, #33872, #40376, #26705, #22327, #26263, #33412, #16319, #1999, #9160, #12180, #11950, #40803, #5027, #19117, #1328, #37339, #29509, #19549, #5238, #5701, #8727, #22792, #19328, #19788, #1756, #26018, #11737, #16094, #33205, #25806, #39919, #8261, #1542, #15638, #15863, #40129, #29954, #44037, #26487, #8492, #40588, #8934, #36428, #23005, #18895, #37099, #5455, #32990, #33646, #30178, #44269, #12627, #45184, #41268, #45423, #3139, #23914, #44737, #20686, #31316, #17230, #27180, #41491, #6830, #34087, #10301, #34324, #34776, #13785, #16555, #27620, #9624, #20011, #2920, #30640, #23686, #9845, #13097, #12853, #38035, #37564, #3383, #27864, #44495, #2694, #26935, #6392, #6146, #41037, #13547, #37797, #20474, #5921, #16790, #20236, #30869, #2453, #35006, #44964, #24374, #20910, #27396, #41959, #9397, #13321, #34561, #30401, #38479, #23465, #17009, #31087, #41729, #10083, #24155, #38264, #6610, #3618, #39405, #11001, #29000, #14467, #17923, #365, #43084, #31993, #17706, #31557, #21835, #10765, #819, #39645, #25532, #24842, #38961, #28546, #35240, #25068, #42640, #39182, #137, #7532, #21606, #14919, #14701, #11448, #42395, #7311, #38715, #42172, #35688, #28777, #7999, #32240, #28296, #32470, #35929, #4063, #31767, #7756, #18390, #4299, #14226, #18164, #22064, #21157, #36155, #21388, #14007, #17476, #600, #42855, #45657, #28076, #10522, #11222, #24597, #25293, #35461, #7076, #3834, #1699, #29237, #40319, #19061, #4517, #22737, #15804, #43314, #26432, #44210, #11682, #22279, #18839, #5013, #18881, #32736, #8248, #26003, #15195, #29042, #11936, #8037, #19534, #5224, #43127, #32973, #22103, #22548, #36416, #4556, #8713, #1081, #40114, #18646, #1316, #4778, #15418, #29279, #5440, #29495, #26474, #857, #43567, #12395, #43358, #8478, #19104, #11723, #19313, #40575, #22779, #36873, #8921, #15848, #22991, #37324, #63, #19774, #38638, #27166, #14155, #30624, #2438, #16540 ),
 ( #19998, #26917, #44720, #6997, #1983, #13082, #5683, #41254, #33859, #44951, #21082, #28226, #2679, #9610, #23671, #27383, #16305, #6132, #9383, #30388, #23450, #3544, #34308, #42320, #37784, #44479, #17630, #20223, #31695, #16775, #12836, #10685, #24768, #38884, #7239, #16081, #30165, #44255, #12614, #26691, #40788, #9145, #23214, #8629, #15765, #22460, #32653, #28959, #1447, #32432, #18792, #5146, #1227, #32882, #43488, #11855, #40035, #35886, #19231, #25247, #36567, #29188, #43037, #29628, #781, #25926, #33317, #8390, #4921, #12082, #11639, #18352, #7956, #22024, #40274, #39357, #25716, #1663, #14881, #25488, #36113, #4478, #18569, #39828, #2583, #27078, #12529, #26603, #16001, #1894, #33544, #19685, #30083, #41171, #19915, #9525, #5356, #23123, #34459, #44166, #9057, #34209, #33992, #16218, #26824, #37920, #5594, #30771, #37228, #40702, #16686, #37694, #6044, #30992, #33778, #27302, #30295, #12745, #2129, #44862, #44389, #26390, #40491, #8843, #40931, #20133, #20365, #2821, #13225, #9297, #41396, #23366, #19449, #22911, #37468, #5830, #16913, #2343, #16444, #30526, #37002, #9743, #44626, #12991, #23589, #23810, #6277, #45090, #42074, #17133, #10423, #3043, #38859, #21283, #24969, #14129, #31451, #38608, #42295, #27754, #17598, #6733, #13673, #34907, #3736, #28201, #7431, #7210, #10200, #35361, #13905, #17824, #20807, #31217, #17364, #27979, #24500, #6967, #41856, #31891, #24278, #45311, #263, #28440, #21052, #42539, #3272, #35135, #10903, #21504, #35582, #3960, #18053, #13447, #27515, #41616, #20590, #34685, #1176, #28679, #15505, #22641, #29370, #39549, #35830, #25878, #39300, #29130, #29585, #8127, #43214, #15044, #18518, #14607, #14827, #28902, #32824, #500, #7906, #8339, #43661, #4207, #36507, #39991, #18737, #32597, #22402, #15285, #32377, #730, #18299, #21733, #7655, #21977, #42982, #43441, #39779, #11809, #25188, #11348, #8576, #25426, #36063, #4869, #22190, #4430, #940, #12033, #11588, #18971, #25666, #36283, #33064, #1401, #26101, #5096, #4639, #40213, #36738, #32135, #42756, #11119, #36956, #37871, #33272, #15717, #33728, #44576, #27253, #9693, #12935, #22863, #34156, #12478, #12259, #19186, #26557, #9008, #41344, #19633, #8795, #5309, #1618, #2528, #23758, #23078, #40655, #37177, #23537, #29803, #16167, #19405, #30249, #33491, #30472, #41122, #44815, #33944, #5536, #12696, #16393, #1839, #37420, #2075, #15948, #44341, #37638, #19863, #43882, #23316, #30030, #27023, #26340, #26776, #16632, #40882, #9246, #5777, #2295, #40443, #44114, #9475, #5990, #20081, #30720, #13172, #3689, #23989, #38799, #32700, #38553, #38336, #42247, #20990, #6466, #34637, #9918, #41565, #27466, #13618, #38111, #35082, #13855, #3456, #45041, #17083, #28378, #2994, #31161, #28155, #42027, #24228, #20758, #31842, #45257, #7156, #27700, #41804, #21232, #14080, #35312, #24917, #6682, #17776, #34850, #3214, #17305, #212, #31394, #6219, #34403, #2773, #45499, #14306, #42480, #10846, #16865, #10373, #30946, #24449, #13396, #6909, #17551, #28848, #29532, #39491, #25138, #7604, #21456, #22349, #43606, #42929, #32322, #11294, #43395, #39031, #18464, #21682, #32543, #35775, #29321, #11762, #18918, #8075, #25373, #11533, #36227, #4152, #39727, #676, #14777, #7847, #25828, #39942, #11973, #8286, #21925, #36453, #4817, #33013, #7380, #35534, #3908, #18003, #32076, #444, #44290, #32928, #18386, #39401, #43525, #15143, #36371, #18160, #4966, #26201, #15372, #43080, #25289, #36151, #19057, #25963, #11444, #40069, #40315, #39866, #596, #8207, #8431, #1483, #36610, #32466, #32235, #14697, #11678, #815, #28773, #21831, #25528, #39641, #32691, #7995, #4513, #18606, #25754, #22275, #37733, #26864, #5865, #30566, #3253, #6085, #40973, #15800, #2386, #44206, #43976, #26641, #37506, #36827, #30336, #33583, #45539, #16257, #44428, #13890, #16036, #23163, #17345, #9334, #27964, #12782, #40737, #44667, #13027, #40529, #19954, #19486, #12351, #23403, #8878, #1933, #33813, #22942, #5178, #19725, #29890, #8669, #27117, #22733, #9093, #19264, #34029, #30119, #33353, #16485, #37039, #2166, #26428, #37271, #12566, #5631, #5391, #1695, #41208, #34890, #9564, #23624, #20173, #31432, #24951, #32117, #32579, #710, #7885, #28419, #10639, #39529, #35344, #3720, #21, #21962, #28186, #18283, #35565, #36047, #39066, #42518, #7413, #4409, #10883, #42279, #10409, #14808, #17807, #25407, #18499, #922, #31874, #246, #21488, #14113, #3942, #18035, #14588, #24720, #28660, #35811, #3496, #42738, #15026, #11103, #25172, #39283, #7639, #24485, #38839, #7192, #21715, #38592, #14341, #32356, #42060, #21265, #28882, #4188, #42962, #11330, #6947, #21030, #35119, #17583, #31654, #18717, #4618, #36486, #32803, #43858, #36720, #12241, #22170, #39972, #5517, #1158, #8318, #5292, #5078, #33048, #43644, #8991, #22383, #1817, #4852, #15263, #19386, #8778, #22846, #2057, #29352, #44097, #1384, #29567, #43425, #15925, #11792, #29112, #43197, #25649, #12013, #36939, #37159, #19613, #33472, #18951, #12461, #15488, #36261, #11567, #26078, #40191, #33707, #8556, #22618, #19170, #39762, #26540, #8109, #33254, #1600, #15698, #30009, #29783, #26321, #40426, #40638, #23059, #27449, #38094, #41788, #30928, #2508, #9675, #13376, #44557, #34384, #23518, #30453, #5972, #20528, #16849, #24212, #20291, #27004, #41547, #16613, #23971, #9456, #19844, #34138, #30701, #13153, #44797, #12916, #9900, #41101, #33926, #6449, #37851, #45023, #12679, #45240, #6667, #34622, #37619, #2277, #13601, #16376, #2978, #17066, #2754, #27233, #31143, #27683, #20062, #41325, #6200, #5756, #37401, #10138, #38321, #20741, #34834, #16150, #9225, #44324, #40864, #23298, #45713, #25123, #24900, #7137, #17761, #28834, #42232, #21665, #14065, #20970, #39236, #28609, #42691, #21908, #3440, #18228, #21216, #3674, #17536, #35757, #31610, #3197, #17288, #45483, #31825, #11056, #11279, #39471, #7589, #6891, #32304, #10587, #42013, #31377, #24664, #38779, #25356, #196, #38538, #28137, #13839, #659, #7830, #35297, #14288, #28359, #4135, #27918, #10828, #39015, #7365, #21441, #14532, #14760, #42913, #17985, #35517, #3893, #428, #32057, #10358, #24434, #4575, #25812, #40381, #36672, #44043, #40136, #15216, #15644, #36435, #43804, #29304, #39711, #8268, #22333, #32997, #4799, #32756, #33211, #18667, #8060, #12187, #29517, #5032, #32528, #19334, #26492, #1548, #43378, #22123, #29726, #43150, #1335, #33418, #11957, #15440, #18901, #43590, #18449, #11746, #39925, #19123, #4360, #26025, #26267, #8500, #8732, #22798, #29958, #1761, #22568, #11515, #36891, #5244, #25601, #15870, #12412, #875, #40593, #8940, #35994, #14978, #29063, #36211, #30406, #37569, #17014, #23691, #13552, #13101, #41042, #13325, #27401, #9165, #20241, #33877, #12631, #41274, #23240, #16324, #2457, #37344, #5461, #34092, #30184 ),
 ( #27185, #27625, #41498, #34567, #9402, #5706, #20480, #44498, #12860, #26709, #2926, #19793, #44970, #16561, #31091, #20015, #23469, #5925, #45190, #44743, #2229, #37104, #9848, #26942, #6397, #41733, #23010, #9628, #37803, #6151, #40808, #34329, #2699, #16796, #30873, #23919, #38041, #19556, #33651, #2003, #16100, #44274, #28301, #34782, #42401, #21393, #39187, #24847, #20915, #25073, #28552, #3623, #24380, #371, #11006, #42645, #6836, #21163, #32245, #13791, #35694, #14013, #6617, #7537, #31772, #35012, #605, #17711, #143, #14706, #17482, #24603, #4071, #10770, #28782, #14233, #28082, #14472, #21612, #41965, #7316, #3390, #45428, #38966, #10308, #31562, #35245, #38484, #38270, #35466, #17235, #10087, #18169, #24161, #42178, #20691, #3839, #45662, #3145, #17931, #10528, #31999, #31322, #38721, #7082, #27869, #14924, #1706, #36160, #22742, #33361, #39874, #26210, #21841, #25762, #32936, #15809, #1492, #8677, #29242, #11455, #40324, #4522, #18614, #825, #36835, #29007, #19066, #36380, #5187, #8215, #43320, #22284, #19274, #11689, #43089, #11227, #15590, #32701, #42860, #25300, #39410, #1046, #15153, #4742, #25538, #18846, #1281, #15381, #39651, #29460, #43533, #7764, #40079, #11900, #29672, #35934, #25971, #4304, #8439, #22509, #18395, #36618, #8004, #12127, #43750, #4973, #22070, #33155, #32475, #16735, #26650, #40986, #6332, #33593, #9793, #33824, #26438, #13270, #2398, #27128, #6095, #23861, #27348, #16498, #37048, #23635, #19736, #19495, #2177, #13038, #12361, #23415, #44216, #20185, #30817, #44912, #40747, #9345, #20414, #1943, #37977, #16269, #40537, #41442, #30578, #41218, #34263, #34510, #2869, #44681, #5400, #37745, #30348, #16045, #44439, #9575, #8886, #5876, #9106, #29900, #37517, #19966, #43984, #37283, #12796, #22952, #2638, #30128, #34041, #26877, #12574, #23174, #5642, #14177, #27808, #6559, #35192, #3090, #10249, #42122, #31267, #45136, #28028, #24096, #35636, #21334, #31037, #34957, #27570, #38663, #38431, #41673, #31717, #17179, #10473, #38210, #3328, #41903, #17424, #34730, #21554, #24327, #10952, #7484, #13953, #311, #10031, #45606, #7019, #16960, #35412, #28494, #31502, #45368, #14414, #6782, #20858, #20636, #25024, #13731, #38910, #24548, #39133, #21109, #3568, #17656, #84, #42344, #10710, #24793, #3782, #7263, #17874, #31940, #12076, #43031, #11395, #4473, #21786, #11633, #32647, #25710, #32427, #39822, #18564, #1443, #1221, #25479, #22455, #26153, #22231, #28731, #36328, #15328, #33105, #18786, #14876, #19013, #36559, #39596, #7951, #989, #35881, #8168, #15094, #4688, #776, #32875, #29180, #15544, #29411, #22018, #4916, #40268, #43482, #42811, #11850, #25921, #43703, #40031, #28952, #8623, #22687, #8385, #18346, #4010, #18109, #32190, #36109, #551, #14654, #7707, #11171, #25243, #39352, #4256, #9292, #2339, #12987, #30767, #20129, #23362, #43932, #44622, #26597, #26384, #9052, #19911, #19226, #12740, #15997, #27297, #44384, #26820, #41391, #44158, #5587, #44858, #37463, #9739, #40926, #37223, #41168, #9519, #22905, #16439, #1886, #40485, #5825, #36996, #30078, #16212, #5351, #15760, #2124, #12311, #36783, #23585, #5140, #19679, #29848, #37690, #12523, #8837, #6038, #19444, #34205, #33539, #33773, #40696, #2577, #13220, #28430, #17126, #3729, #14352, #20801, #7203, #2817, #6727, #13899, #42529, #28195, #35354, #10195, #38158, #21275, #31211, #45306, #27511, #17817, #9968, #30, #17358, #31885, #34898, #24272, #3264, #255, #38379, #24037, #37916, #42288, #13667, #23805, #6271, #20357, #34455, #16908, #30988, #27748, #41850, #31442, #10650, #45085, #45548, #41611, #27972, #6508, #35128, #14123, #13441, #38601, #42068, #10418, #21042, #20585, #24494, #6958, #3038, #3507, #24731, #17592, #31663, #38851, #21726, #36274, #11339, #18727, #4199, #14598, #28892, #42974, #7896, #25418, #7647, #8119, #25181, #28671, #32815, #4419, #25658, #7424, #40601, #2013, #22180, #18291, #42749, #4631, #18046, #21970, #8952, #32589, #36056, #39539, #18509, #39075, #39293, #35820, #11578, #24962, #32366, #1770, #23020, #11111, #15881, #29969, #43207, #932, #44053, #39771, #721, #14819, #15035, #492, #32127, #29123, #12420, #5472, #19566, #33664, #3953, #30194, #10894, #21497, #35575, #20489, #20249, #2467, #13112, #24172, #37579, #17022, #9411, #16334, #34575, #23928, #38049, #17245, #30415, #13560, #16573, #44753, #44512, #31099, #12872, #44284, #12640, #40821, #41283, #6407, #6625, #34791, #2935, #2239, #27634, #5934, #37354, #26720, #20024, #34101, #20700, #9636, #33886, #26954, #23700, #45198, #30656, #41054, #37812, #6161, #34341, #2711, #23478, #41507, #16804, #30884, #41743, #44979, #13333, #9176, #10096, #3154, #9858, #27410, #38280, #23252, #5715, #19802, #28791, #7325, #42410, #14242, #17719, #13801, #14024, #28093, #32009, #45439, #38731, #7546, #42869, #3399, #35706, #25082, #17941, #31783, #21623, #381, #31571, #45671, #35021, #20925, #6845, #7093, #17493, #14484, #38975, #28563, #24389, #42187, #7776, #10537, #24613, #4081, #21401, #35254, #153, #11236, #21174, #18180, #3632, #28311, #32256, #11015, #39196, #4312, #10781, #614, #24858, #35475, #3850, #14715, #42653, #31331, #27878, #41976, #25309, #39422, #21853, #35946, #10318, #38493, #11467, #19284, #36170, #5411, #12807, #30590, #27578, #27138, #9116, #9584, #30138, #34519, #13504, #23644, #37755, #6104, #23870, #19506, #20194, #41451, #37989, #20426, #16969, #41684, #10038, #24107, #44226, #31724, #3790, #20865, #10719, #45614, #6789, #28036, #10959, #38918, #557, #42350, #3338, #28500, #25028, #21560, #7270, #17431, #35642, #4015, #91, #34964, #14659, #28736, #42816, #31511, #14183, #11178, #41913, #38219, #42129, #17186, #6566, #24799, #20644, #31274, #13739, #27816, #21341, #10257, #24334, #10480, #38438, #38670, #13962, #7029, #35199, #42374, #10743, #31971, #9252, #4644, #36741, #8342, #22407, #38117, #27935, #27471, #9697, #27707, #41811, #23541, #34643, #2532, #27027, #9922, #37643, #30725, #16869, #5993, #19869, #2777, #44580, #10377, #10157, #5781, #23762, #33948, #13400, #13177, #2299, #6470, #20086, #30951, #12941, #37875, #16637, #6223, #9478, #42031, #44819, #17310, #37424, #34408, #20765, #16397, #20315, #41570, #30477, #24233, #3220, #45045, #34161, #34856, #27258, #41348, #41126, #31401, #23995, #13623, #20546, #45506, #3000, #17088, #31167, #13859, #45263, #38342, #6687, #28852, #17780, #7852, #893, #32547, #31845, #217, #24921, #42252, #32080, #7384, #450, #7161, #14554, #39035, #21930, #21686, #14311, #42933, #14996, #42710, #3462, #11074, #28383, #11300, #24453, #21460, #10610, #35538, #28159, #35779, #680, #4378, #39255, #10852, #18008, #4157, #21235, #25142, #42485, #38805, #3914, #25378, #7609, #29083, #28632, #35315, #18252, #32326, #14780, #39495, #24686, #36015, #18468 ),
 ( #3693, #43170, #38560, #6914, #20994, #35087, #17555, #31627, #13512, #14084, #43824, #43612, #1783, #26287, #11765, #25833, #15236, #1123, #32776, #18923, #29325, #40400, #19141, #8750, #4592, #22354, #33675, #43399, #8290, #33440, #33228, #15459, #26046, #37126, #4821, #29979, #36459, #39945, #15893, #36908, #5262, #30205, #33018, #26510, #29537, #11978, #1356, #44066, #40157, #11538, #25620, #8080, #8522, #19354, #19580, #2025, #12431, #22587, #40611, #36691, #18687, #39731, #5050, #1568, #16119, #15666, #29746, #12208, #22142, #8962, #36231, #22816, #23031, #5483, #37591, #2251, #16588, #30670, #41298, #44767, #41066, #41520, #12884, #16346, #20502, #37824, #13348, #40833, #27650, #35432, #9872, #5945, #30426, #38063, #5728, #9648, #41759, #20264, #23713, #27204, #13126, #26730, #26969, #9424, #44992, #12650, #20036, #34591, #10109, #44526, #2948, #6420, #30898, #6175, #17036, #27423, #23491, #34113, #2480, #33897, #19814, #34355, #2724, #23943, #16820, #31114, #37366, #45210, #21354, #13573, #24186, #38292, #6639, #3803, #17894, #44295, #9191, #23266, #42829, #4031, #8184, #11653, #25729, #4937, #18130, #1244, #35900, #32445, #32209, #4705, #571, #31961, #332, #28516, #793, #39842, #40047, #22473, #22249, #35657, #15347, #25263, #25041, #14435, #39372, #21804, #8404, #14893, #21575, #14672, #42612, #29427, #36580, #4273, #7726, #18365, #36347, #10972, #28973, #28748, #43054, #11190, #43283, #18808, #11867, #1010, #11416, #25502, #29204, #39615, #4491, #7970, #22037, #36128, #32898, #32667, #39151, #18583, #15115, #43500, #25940, #7503, #40945, #16456, #36802, #23378, #12757, #5605, #5368, #9308, #33789, #19242, #33329, #22704, #8642, #40286, #26402, #5158, #2140, #26616, #16229, #12095, #29867, #41182, #1674, #15778, #37481, #40714, #22922, #33557, #44641, #12329, #5842, #43950, #40504, #19928, #44402, #26836, #37706, #8855, #34003, #37014, #19462, #1905, #2357, #16014, #19033, #33124, #15560, #30095, #30539, #27090, #9536, #13002, #44177, #23600, #12541, #26174, #1460, #9070, #23136, #29640, #37242, #19699, #30308, #43720, #35148, #14141, #9987, #45102, #24056, #10436, #6055, #3055, #23822, #17144, #9757, #17379, #27990, #31680, #20819, #38174, #45325, #3284, #34472, #24289, #13459, #20376, #41628, #24511, #6745, #28212, #10212, #16924, #31462, #6523, #13918, #27528, #37933, #20601, #34696, #31229, #13687, #2832, #45566, #31004, #6291, #42085, #27766, #34920, #2597, #3525, #42306, #38620, #41868, #38395, #6980, #13236, #21065, #17611, #47, #10670, #24754, #20146, #34222, #16698, #30783, #44874, #27314, #41407, #28913, #29378, #43226, #4650, #25202, #7443, #36292, #32148, #511, #42552, #18747, #24983, #15056, #32390, #32835, #35843, #7668, #21746, #1186, #4218, #39093, #7224, #11597, #14619, #22200, #15294, #43450, #28691, #42770, #18311, #10914, #741, #14840, #42994, #21518, #11360, #25439, #11817, #36074, #11130, #25675, #38869, #39560, #17836, #7915, #4441, #21295, #21985, #3972, #8136, #39788, #18527, #35595, #29142, #35373, #3748, #18066, #32609, #31903, #950, #275, #14372, #28453, #33279, #36049, #15028, #8111, #22385, #15265, #4411, #7415, #11569, #21718, #14590, #4190, #924, #28421, #7887, #42964, #36489, #25410, #18502, #17809, #29115, #36264, #4620, #18719, #32806, #10417, #24271, #24730, #38850, #6507, #42528, #10194, #38378, #38600, #6726, #17357, #45547, #13898, #34454, #6957, #24961, #2816, #16907, #22294, #29684, #36390, #19286, #33167, #4753, #29913, #36631, #22753, #1293, #12140, #4985, #26222, #43544, #8225, #8689, #11910, #1503, #26665, #40337, #26449, #1717, #43998, #22965, #37060, #40762, #5413, #33605, #1957, #16057, #44229, #12586, #21769, #28936, #32628, #18089, #7936, #42792, #3991, #25222, #39805, #36093, #43466, #39579, #534, #15075, #35863, #43246, #28711, #39115, #7689, #4240, #32410, #18330, #32171, #972, #14638, #7464, #11617, #43013, #4458, #31923, #18769, #25905, #29162, #11153, #21537, #25694, #42576, #759, #32855, #11377, #14860, #25460, #22003, #17857, #39334, #18547, #8153, #3767, #22216, #36309, #1205, #35619, #4671, #15313, #29395, #11834, #40014, #8366, #35394, #295, #14395, #25005, #10935, #28475, #12060, #37206, #30061, #5570, #15529, #33298, #44607, #26134, #19211, #44369, #44142, #26368, #36982, #2324, #15744, #40910, #1643, #40249, #12724, #2107, #16196, #41153, #8606, #37449, #40470, #22890, #22671, #9277, #36767, #22435, #36540, #18998, #5335, #30276, #30504, #12968, #26804, #5123, #5808, #29832, #29610, #4899, #43913, #12292, #27057, #19430, #8822, #33522, #33090, #19896, #1427, #1870, #15977, #43687, #12506, #26582, #40680, #23346, #9034, #23104, #19662, #33755, #33973, #16422, #24257, #9725, #3026, #16664, #41596, #34436, #9952, #27283, #14749, #2802, #35744, #647, #6493, #38585, #34188, #38142, #45292, #28822, #13883, #21023, #24023, #23789, #6941, #16893, #30974, #13205, #4123, #41376, #31425, #17113, #18217, #20571, #34667, #31194, #32292, #13651, #37901, #23568, #27958, #45072, #9504, #37673, #6022, #13427, #27497, #27732, #6254, #41835, #10181, #38365, #20342, #6711, #20788, #20113, #34883, #3247, #42054, #2559, #17338, #30749, #45531, #10402, #44843, #24479, #8048, #12177, #15635, #36425, #11504, #33202, #43796, #29718, #39700, #8258, #19324, #865, #22789, #1092, #39460, #26259, #15429, #40125, #19114, #36884, #40372, #29506, #4347, #36663, #32746, #32516, #15205, #26014, #25345, #18891, #22112, #33409, #4788, #32986, #1753, #4565, #11733, #5235, #43579, #15860, #1325, #29293, #1538, #8724, #29052, #8488, #36202, #14967, #11947, #43138, #18656, #22324, #25589, #43369, #25803, #22559, #11269, #39916, #42902, #7818, #5024, #21896, #35982, #18438, #16316, #20233, #44731, #30175, #44266, #33642, #19546, #5452, #37335, #1995, #13094, #37560, #27176, #23002, #40800, #6388, #16091, #26702, #6143, #5918, #33869, #44491, #9842, #23229, #2690, #9157, #12624, #34320, #9620, #23682, #2916, #5697, #44960, #2222, #30398, #19784, #16787, #12849, #29949, #44033, #26484, #26930, #37793, #38032, #20470, #30866, #41033, #13317, #9392, #37096, #12404, #23461, #20008, #34557, #34084, #2449, #16551, #40585, #27393, #8931, #30636, #41264, #41488, #23911, #17006, #14003, #34773, #28072, #20683, #28291, #38957, #42636, #31763, #3379, #10518, #14222, #45419, #35236, #38475, #31312, #6826, #21384, #17702, #39178, #21152, #27860, #42391, #17471, #24837, #10297, #3136, #35002, #31553, #42167, #45653, #13781, #10761, #41955, #17226, #7307, #24593, #133, #13543, #361, #7528, #3830, #20906, #38711, #17919, #24151, #7072, #14463, #3614, #31989, #28541, #10997, #41725, #21602, #10079, #35684, #31083, #38260, #6605, #11443, #25962, #1482, #21830, #8430, #43524, #36370, #36150, #40068, #18835, #4295, #18385, #7752, #39400, #25288, #25527 ),
 ( #7994, #4512, #32465, #22499, #35924, #22732, #18159, #595, #18605, #29451, #12119, #40314, #11890, #814, #19056, #43079, #42851, #4059, #39640, #22060, #26200, #32690, #14915, #28996, #32234, #33146, #8668, #1038, #15142, #29233, #36609, #14696, #43309, #11677, #25753, #39865, #15371, #4965, #29664, #32927, #8206, #22274, #1272, #4733, #15582, #43740, #28772, #11218, #39004, #35286, #42681, #38769, #45473, #14276, #3428, #42449, #27907, #38310, #6880, #17526, #31599, #45704, #31366, #31815, #3188, #6656, #10817, #28126, #3664, #31132, #32045, #25112, #185, #42004, #20730, #28347, #41777, #14055, #417, #10575, #24652, #7126, #34824, #24890, #21205, #17751, #45229, #14521, #39226, #7355, #10347, #17275, #21431, #10127, #35507, #28598, #3882, #11047, #7579, #34610, #17055, #13830, #24421, #2967, #13590, #38526, #24201, #19113, #39459, #26013, #15428, #8257, #8047, #11946, #36424, #21895, #35981, #25344, #11268, #42901, #29051, #7817, #4787, #29292, #18890, #14748, #32515, #43795, #4346, #18437, #43578, #43368, #25588, #36201, #1537, #14966, #40124, #864, #43137, #8487, #1324, #29505, #40371, #11503, #36662, #39699, #22111, #4564, #22558, #18655, #21656, #35743, #18216, #32745, #5023, #29717, #12176, #33201, #1091, #15634, #15204, #28821, #4122, #11732, #25802, #26258, #39915, #22323, #32985, #32291, #646, #16786, #12623, #1994, #26701, #13093, #8723, #5696, #26483, #19783, #12403, #20007, #30635, #34319, #23460, #40799, #2221, #5917, #37095, #26929, #16090, #23001, #44265, #27175, #9391, #30865, #12848, #19545, #34083, #9156, #16550, #30174, #40584, #23228, #37334, #33868, #16315, #5451, #2448, #33641, #44730, #27392, #8930, #23681, #30397, #44490, #41032, #41263, #37559, #22788, #36883, #5234, #9619, #37792, #44959, #13316, #6142, #20232, #2689, #19323, #1752, #33408, #15859, #29948, #44032, #41954, #31082, #45180, #38031, #38956, #3829, #45418, #34772, #13780, #14221, #41487, #38474, #13542, #6825, #27616, #7071, #17701, #21383, #10517, #27859, #3378, #38710, #24150, #14002, #3135, #10078, #31311, #42390, #42166, #360, #28071, #6604, #35235, #10296, #31762, #17225, #41724, #24370, #20905, #17470, #31552, #38259, #10760, #20682, #24592, #7306, #35457, #6387, #20469, #34556, #2915, #17005, #115, #38940, #19250, #32675, #22481, #22929, #1467, #36591, #8414, #11875, #7978, #8192, #22259, #26183, #39625, #32910, #1682, #37022, #43294, #29875, #33337, #12104, #25947, #15786, #40297, #25737, #39850, #29213, #15124, #1021, #1254, #11661, #8652, #33131, #22715, #18591, #36356, #1916, #4715, #18818, #43960, #15567, #29435, #40054, #5377, #15356, #12338, #43508, #4949, #26411, #5165, #40512, #8862, #19040, #36810, #29648, #43727, #19470, #33566, #16023, #30102, #44188, #22045, #25511, #36137, #4499, #16936, #26624, #30550, #40722, #34233, #34014, #9079, #27324, #12766, #6067, #19711, #44650, #37490, #13012, #30320, #17155, #5850, #38187, #3065, #9547, #41644, #37252, #41193, #2607, #31241, #31015, #24069, #27102, #26847, #9999, #19938, #2369, #16241, #6532, #44411, #34484, #20157, #20612, #23610, #37717, #16708, #34707, #30793, #40956, #23145, #45113, #16467, #12549, #5615, #33797, #44885, #13246, #41417, #9318, #9766, #23833, #37948, #23389, #6302, #20386, #2149, #2843, #13470, #27540, #21759, #17847, #24301, #31913, #10925, #28701, #14385, #10448, #14629, #18078, #38881, #13928, #35607, #523, #32158, #42097, #10682, #35853, #3297, #25212, #3540, #41879, #42780, #285, #42563, #21528, #39323, #11142, #28463, #6758, #39104, #35161, #34931, #17626, #24993, #27779, #21307, #24524, #4230, #7236, #35384, #18322, #6994, #14152, #7679, #7454, #45337, #3757, #31692, #13699, #38634, #38407, #10223, #21077, #60, #20831, #28222, #17391, #31476, #45580, #28003, #42317, #24764, #3981, #36302, #36758, #32402, #29387, #4451, #43459, #36085, #43680, #8595, #12281, #1420, #18758, #25896, #29602, #15067, #4889, #39798, #962, #22209, #5114, #33083, #40461, #36532, #43237, #12051, #32848, #40238, #25686, #18539, #4659, #1196, #11826, #15304, #29154, #26123, #11608, #32619, #22661, #40007, #15522, #28927, #15733, #22882, #19202, #8146, #8357, #33289, #39571, #22423, #29822, #18990, #1634, #43904, #26357, #14850, #8813, #36973, #5326, #752, #43005, #11369, #25452, #7926, #21996, #13197, #6011, #5799, #23780, #16656, #19653, #44359, #37195, #9025, #40671, #23336, #12715, #27276, #27045, #41368, #12497, #37439, #9943, #16413, #30493, #37893, #41143, #37662, #6244, #45064, #20334, #34427, #2794, #16886, #24015, #1861, #30049, #44132, #26573, #45013, #5745, #13366, #40851, #9212, #1026, #40104, #8468, #5003, #26466, #23203, #15616, #19304, #37312, #15839, #12605, #33851, #27156, #20662, #13760, #31533, #17205, #13297, #17450, #20886, #41705, #16764, #38456, #3359, #34981, #44940, #13524, #24574, #6123, #28055, #6365, #44710, #45634, #34754, #45397, #24352, #42148, #13983, #3115, #9602, #41933, #38011, #37774, #20448, #31292, #30613, #24129, #27373, #38691, #10059, #38239, #7050, #9821, #16987, #10499, #27838, #21134, #6585, #34537, #6807, #2428, #34297, #10278, #41468, #20213, #16529, #2668, #23889, #27597, #30844, #13070, #41245, #23662, #2896, #31064, #45162, #7508, #17682, #11196, #10977, #31742, #4278, #35437, #28754, #42370, #21580, #14442, #35663, #7288, #39847, #28521, #15120, #25734, #32214, #18588, #14203, #18136, #25268, #8189, #39621, #1017, #4036, #3808, #32672, #42617, #25047, #38937, #29210, #21361, #11421, #42834, #43289, #576, #14677, #39378, #11658, #7732, #17900, #3594, #7975, #39157, #35218, #111, #28271, #21810, #35905, #18370, #31967, #32450, #798, #14898, #337, #28979, #43059, #10739, #25508, #22042, #36134, #4496, #24817, #15564, #1679, #36586, #4711, #33334, #29432, #40952, #26621, #36353, #40292, #18814, #43955, #43724, #32905, #37019, #22478, #15783, #43505, #8648, #1464, #22709, #40051, #26843, #29645, #2146, #12763, #19247, #5611, #1250, #5162, #12334, #22255, #40718, #33794, #36806, #4942, #19706, #12101, #26178, #25944, #16237, #8410, #44183, #29871, #30314, #26407, #40508, #8859, #44408, #22926, #19037, #15353, #9076, #5374, #11872, #33128, #19467, #33561, #1911, #16019, #30099, #12545, #23142, #37247, #37713, #16932, #23829, #6753, #6528, #2603, #27772, #31470, #27536, #34010, #41638, #20608, #38403, #24064, #20151, #24297, #41875, #2839, #23606, #45332, #10219, #20826, #6062, #20381, #45573, #13008, #34927, #13242, #5847, #3292, #9994, #34703, #31237, #17387, #13924, #38182, #16464, #3062, #44881, #44646, #27320, #17151, #37487, #31011, #34228, #27997, #45109, #13466, #9314, #16703, #37941, #23385, #13694, #19935, #2364, #41413, #30547, #27098, #41189, #9543, #30789, #9762, #6298, #34480, #54, #38876, #18317, #18072, #281, #10920, #21991, #35378, #14846, #7232, #14147 ) ),
 .UNSPECIFIED., .T., .F., .T. ) 
 B_SPLINE_SURFACE_WITH_KNOTS ( ( 4, 3, 4 ),
 ( 3, 2, 2, 2, 2, 2, 2, 2, 2, 2, 2, 2, 2, 2, 2, 2, 2, 2, 2, 2, 2, 2, 2, 2, 2, 2, 2, 2, 2, 2, 2, 2, 2, 2, 2, 2, 2, 2, 2, 2, 2, 2, 2, 2, 2, 2, 2, 2, 2, 2, 2, 2, 2, 2, 2, 2, 2, 2, 2, 2, 2, 2, 2, 2, 2, 2, 2, 2, 2, 2, 2, 2, 2, 2, 2, 2, 2, 2, 2, 2, 2, 2, 2, 2, 2, 2, 2, 2, 2, 2, 2, 2, 2, 2, 2, 2, 2, 2, 2, 2, 2, 2, 2, 2, 2, 2, 2, 2, 2, 2, 2, 2, 2, 2, 2, 2, 2, 2, 2, 2, 2, 2, 2, 2, 2, 2, 2, 2, 2, 2, 2, 2, 2, 2, 2, 2, 2, 2, 2, 2, 2, 2, 2, 2, 2, 2, 2, 2, 2, 2, 2, 2, 2, 2, 2, 2, 2, 2, 2, 2, 2, 2, 2, 2, 2, 2, 2, 2, 2, 2, 2, 2, 2, 2, 2, 2, 2, 2, 2, 2, 2, 2, 2, 2, 2, 2, 2, 2, 2, 2, 2, 2, 2, 2, 2, 2, 2, 2, 2, 2, 2, 2, 2, 2, 2, 2, 2, 2, 2, 2, 2, 2, 2, 2, 2, 2, 2, 2, 2, 2, 2, 2, 2, 2, 2, 2, 2, 2, 2, 2, 2, 2, 2, 2, 2, 2, 2, 2, 2, 2, 2, 2, 2, 2, 2, 2, 2, 2, 2, 2, 2, 2, 2, 2, 2, 2, 2, 2, 2, 2, 2, 2, 2, 2, 2, 2, 2, 2, 2, 2, 2, 2, 2, 2, 2, 2, 2, 2, 2, 2, 2, 2, 2, 2, 2, 2, 2, 2, 2, 2, 2, 2, 2, 2, 2, 2, 2, 2, 2, 2, 2, 2, 2, 2, 2, 2, 2, 2, 2, 2, 2, 2, 2, 2, 2, 2, 2, 2, 2, 2, 2, 2, 2, 2, 2, 2, 2, 2, 2, 2, 2, 2, 2, 2, 2, 2, 2, 2, 2, 2, 2, 2, 2, 2, 2, 2, 2, 2, 2, 2, 2, 2, 2, 2, 2, 2, 2, 2, 2, 2, 2, 2, 2, 2, 2, 2, 2, 2, 2, 2, 2, 2, 2, 2, 2, 2, 2, 2, 2, 2, 2, 2, 2, 2, 2, 2, 2, 2, 2, 2, 2, 2, 2, 2, 2, 2, 2, 2, 2, 2, 2, 2, 2, 2, 2, 2, 2, 2, 2, 2, 2, 2, 2, 2, 2, 2, 2, 2, 2, 2, 2, 2, 2, 2, 2, 2, 2, 2, 2, 2, 2, 3 ),
 ( 0.000000000000000000, 0.5000000000000000000, 1.000000000000000000 ),
 ( 0.000000000000000000, 0.002272727272727272617, 0.004545454545454545234, 0.006818181818181817851, 0.009090909090909090468, 0.01136363636363636395, 0.01363636363636363570, 0.01590909090909090745, 0.01818181818181818094, 0.02045454545454545442, 0.02272727272727272790, 0.02500000000000000139, 0.02727272727272727140, 0.02954545454545454489, 0.03181818181818181490, 0.03409090909090908839, 0.03636363636363636187, 0.03863636363636363535, 0.04090909090909090884, 0.04318181818181818232, 0.04545454545454545581, 0.04772727272727272929, 0.05000000000000000278, 0.05227272727272726932, 0.05454545454545454281, 0.05681818181818181629, 0.05909090909090908977, 0.06136363636363636326, 0.06363636363636362980, 0.06590909090909090329, 0.06818181818181817677, 0.07045454545454545026, 0.07272727272727272374, 0.07499999999999999722, 0.07727272727272727071, 0.07954545454545454419, 0.08181818181818181768, 0.08409090909090909116, 0.08636363636363636465, 0.08863636363636363813, 0.09090909090909091161, 0.09318181818181818510, 0.09545454545454545858, 0.09772727272727273207, 0.1000000000000000056, 0.1022727272727272790, 0.1045454545454545386, 0.1068181818181818121, 0.1090909090909090856, 0.1113636363636363591, 0.1136363636363636326, 0.1159090909090909061, 0.1181818181818181795, 0.1204545454545454530, 0.1227272727272727265, 0.1250000000000000000, 0.1272727272727272596, 0.1295454545454545470, 0.1318181818181818066, 0.1340909090909090939, 0.1363636363636363535, 0.1386363636363636409, 0.1409090909090909005, 0.1431818181818181879, 0.1454545454545454475, 0.1477272727272727348, 0.1499999999999999944, 0.1522727272727272818, 0.1545454545454545414, 0.1568181818181818288, 0.1590909090909090884, 0.1613636363636363757, 0.1636363636363636354, 0.1659090909090909227, 0.1681818181818181823, 0.1704545454545454419, 0.1727272727272727293, 0.1749999999999999889, 0.1772727272727272763, 0.1795454545454545359, 0.1818181818181818232, 0.1840909090909090828, 0.1863636363636363702, 0.1886363636363636298, 0.1909090909090909172, 0.1931818181818181768, 0.1954545454545454641, 0.1977272727272727237, 0.2000000000000000111, 0.2022727272727272707, 0.2045454545454545581, 0.2068181818181818177, 0.2090909090909090773, 0.2113636363636363646, 0.2136363636363636243, 0.2159090909090909116, 0.2181818181818181712, 0.2204545454545454586, 0.2227272727272727182, 0.2250000000000000056, 0.2272727272727272652, 0.2295454545454545525, 0.2318181818181818121, 0.2340909090909090995, 0.2363636363636363591, 0.2386363636363636465, 0.2409090909090909061, 0.2431818181818181934, 0.2454545454545454530, 0.2477272727272727404, 0.2500000000000000000, 0.2522727272727272596, 0.2545454545454545192, 0.2568181818181818343, 0.2590909090909090939, 0.2613636363636363535, 0.2636363636363636131, 0.2659090909090909283, 0.2681818181818181879, 0.2704545454545454475, 0.2727272727272727071, 0.2750000000000000222, 0.2772727272727272818, 0.2795454545454545414, 0.2818181818181818010, 0.2840909090909091161, 0.2863636363636363757, 0.2886363636363636354, 0.2909090909090908950, 0.2931818181818181546, 0.2954545454545454697, 0.2977272727272727293, 0.2999999999999999889, 0.3022727272727272485, 0.3045454545454545636, 0.3068181818181818232, 0.3090909090909090828, 0.3113636363636363424, 0.3136363636363636576, 0.3159090909090909172, 0.3181818181818181768, 0.3204545454545454364, 0.3227272727272727515, 0.3250000000000000111, 0.3272727272727272707, 0.3295454545454545303, 0.3318181818181818454, 0.3340909090909091050, 0.3363636363636363646, 0.3386363636363636243, 0.3409090909090908839, 0.3431818181818181990, 0.3454545454545454586, 0.3477272727272727182, 0.3499999999999999778, 0.3522727272727272929, 0.3545454545454545525, 0.3568181818181818121, 0.3590909090909090717, 0.3613636363636363869, 0.3636363636363636465, 0.3659090909090909061, 0.3681818181818181657, 0.3704545454545454808, 0.3727272727272727404, 0.3750000000000000000, 0.3772727272727272596, 0.3795454545454545192, 0.3818181818181818343, 0.3840909090909090939, 0.3863636363636363535, 0.3886363636363636131, 0.3909090909090909283, 0.3931818181818181879, 0.3954545454545454475, 0.3977272727272727071, 0.4000000000000000222, 0.4022727272727272818, 0.4045454545454545414, 0.4068181818181818010, 0.4090909090909091161, 0.4113636363636363757, 0.4136363636363636354, 0.4159090909090908950, 0.4181818181818181546, 0.4204545454545454697, 0.4227272727272727293, 0.4249999999999999889, 0.4272727272727272485, 0.4295454545454545636, 0.4318181818181818232, 0.4340909090909090828, 0.4363636363636363424, 0.4386363636363636576, 0.4409090909090909172, 0.4431818181818181768, 0.4454545454545454364, 0.4477272727272727515, 0.4500000000000000111, 0.4522727272727272707, 0.4545454545454545303, 0.4568181818181818454, 0.4590909090909091050, 0.4613636363636363646, 0.4636363636363636243, 0.4659090909090908839, 0.4681818181818181990, 0.4704545454545454586, 0.4727272727272727182, 0.4749999999999999778, 0.4772727272727272929, 0.4795454545454545525, 0.4818181818181818121, 0.4840909090909090717, 0.4863636363636363869, 0.4886363636363636465, 0.4909090909090909061, 0.4931818181818181657, 0.4954545454545454808, 0.4977272727272727404, 0.5000000000000000000, 0.5022727272727273151, 0.5045454545454545192, 0.5068181818181818343, 0.5090909090909090384, 0.5113636363636363535, 0.5136363636363636687, 0.5159090909090908728, 0.5181818181818181879, 0.5204545454545455030, 0.5227272727272727071, 0.5250000000000000222, 0.5272727272727272263, 0.5295454545454545414, 0.5318181818181818565, 0.5340909090909090606, 0.5363636363636363757, 0.5386363636363636909, 0.5409090909090908950, 0.5431818181818182101, 0.5454545454545454142, 0.5477272727272727293, 0.5500000000000000444, 0.5522727272727272485, 0.5545454545454545636, 0.5568181818181817677, 0.5590909090909090828, 0.5613636363636363980, 0.5636363636363636020, 0.5659090909090909172, 0.5681818181818182323, 0.5704545454545454364, 0.5727272727272727515, 0.5749999999999999556, 0.5772727272727272707, 0.5795454545454545858, 0.5818181818181817899, 0.5840909090909091050, 0.5863636363636363091, 0.5886363636363636243, 0.5909090909090909394, 0.5931818181818181435, 0.5954545454545454586, 0.5977272727272727737, 0.5999999999999999778, 0.6022727272727272929, 0.6045454545454544970, 0.6068181818181818121, 0.6090909090909091272, 0.6113636363636363313, 0.6136363636363636465, 0.6159090909090909616, 0.6181818181818181657, 0.6204545454545454808, 0.6227272727272726849, 0.6250000000000000000, 0.6272727272727273151, 0.6295454545454545192, 0.6318181818181818343, 0.6340909090909090384, 0.6363636363636363535, 0.6386363636363636687, 0.6409090909090908728, 0.6431818181818181879, 0.6454545454545455030, 0.6477272727272727071, 0.6500000000000000222, 0.6522727272727272263, 0.6545454545454545414, 0.6568181818181818565, 0.6590909090909090606, 0.6613636363636363757, 0.6636363636363636909, 0.6659090909090908950, 0.6681818181818182101, 0.6704545454545454142, 0.6727272727272727293, 0.6750000000000000444, 0.6772727272727272485, 0.6795454545454545636, 0.6818181818181817677, 0.6840909090909090828, 0.6863636363636363980, 0.6886363636363636020, 0.6909090909090909172, 0.6931818181818182323, 0.6954545454545454364, 0.6977272727272727515, 0.6999999999999999556, 0.7022727272727272707, 0.7045454545454545858, 0.7068181818181817899, 0.7090909090909091050, 0.7113636363636363091, 0.7136363636363636243, 0.7159090909090909394, 0.7181818181818181435, 0.7204545454545454586, 0.7227272727272727737, 0.7249999999999999778, 0.7272727272727272929, 0.7295454545454544970, 0.7318181818181818121, 0.7340909090909091272, 0.7363636363636363313, 0.7386363636363636465, 0.7409090909090909616, 0.7431818181818181657, 0.7454545454545454808, 0.7477272727272726849, 0.7500000000000000000, 0.7522727272727273151, 0.7545454545454545192, 0.7568181818181818343, 0.7590909090909090384, 0.7613636363636363535, 0.7636363636363636687, 0.7659090909090908728, 0.7681818181818181879, 0.7704545454545455030, 0.7727272727272727071, 0.7750000000000000222, 0.7772727272727272263, 0.7795454545454545414, 0.7818181818181818565, 0.7840909090909090606, 0.7863636363636363757, 0.7886363636363636909, 0.7909090909090908950, 0.7931818181818182101, 0.7954545454545454142, 0.7977272727272727293, 0.8000000000000000444, 0.8022727272727272485, 0.8045454545454545636, 0.8068181818181817677, 0.8090909090909090828, 0.8113636363636363980, 0.8136363636363636020, 0.8159090909090909172, 0.8181818181818182323, 0.8204545454545454364, 0.8227272727272727515, 0.8249999999999999556, 0.8272727272727272707, 0.8295454545454545858, 0.8318181818181817899, 0.8340909090909091050, 0.8363636363636363091, 0.8386363636363636243, 0.8409090909090909394, 0.8431818181818181435, 0.8454545454545454586, 0.8477272727272727737, 0.8499999999999999778, 0.8522727272727272929, 0.8545454545454544970, 0.8568181818181818121, 0.8590909090909091272, 0.8613636363636363313, 0.8636363636363636465, 0.8659090909090909616, 0.8681818181818181657, 0.8704545454545454808, 0.8727272727272726849, 0.8750000000000000000, 0.8772727272727273151, 0.8795454545454545192, 0.8818181818181818343, 0.8840909090909090384, 0.8863636363636363535, 0.8886363636363636687, 0.8909090909090908728, 0.8931818181818181879, 0.8954545454545455030, 0.8977272727272727071, 0.9000000000000000222, 0.9022727272727272263, 0.9045454545454545414, 0.9068181818181818565, 0.9090909090909090606, 0.9113636363636363757, 0.9136363636363636909, 0.9159090909090908950, 0.9181818181818182101, 0.9204545454545454142, 0.9227272727272727293, 0.9250000000000000444, 0.9272727272727272485, 0.9295454545454545636, 0.9318181818181817677, 0.9340909090909090828, 0.9363636363636363980, 0.9386363636363636020, 0.9409090909090909172, 0.9431818181818182323, 0.9454545454545454364, 0.9477272727272727515, 0.9499999999999999556, 0.9522727272727272707, 0.9545454545454545858, 0.9568181818181817899, 0.9590909090909091050, 0.9613636363636363091, 0.9636363636363636243, 0.9659090909090909394, 0.9681818181818181435, 0.9704545454545454586, 0.9727272727272727737, 0.9749999999999999778, 0.9772727272727272929, 0.9781254700864303597 ),
 .UNSPECIFIED. ) 
 GEOMETRIC_REPRESENTATION_ITEM ( )  RATIONAL_B_SPLINE_SURFACE ( (
 ( 1.000000000000000000, 0.9898214418809326842, 1.000000000000000000, 0.9898214418809326842, 1.000000000000000000, 0.9898214418809326842, 1.000000000000000000, 0.9898214418809326842, 1.000000000000000000, 0.9898214418809326842, 1.000000000000000000, 0.9898214418809326842, 1.000000000000000000, 0.9898214418809326842, 1.000000000000000000, 0.9898214418809326842, 1.000000000000000000, 0.9898214418809326842, 1.000000000000000000, 0.9898214418809326842, 1.000000000000000000, 0.9898214418809326842, 1.000000000000000000, 0.9898214418809326842, 1.000000000000000000, 0.9898214418809326842, 1.000000000000000000, 0.9898214418809326842, 1.000000000000000000, 0.9898214418809326842, 1.000000000000000000, 0.9898214418809326842, 1.000000000000000000, 0.9898214418809326842, 1.000000000000000000, 0.9898214418809326842, 1.000000000000000000, 0.9898214418809326842, 1.000000000000000000, 0.9898214418809326842, 1.000000000000000000, 0.9898214418809326842, 1.000000000000000000, 0.9898214418809326842, 1.000000000000000000, 0.9898214418809326842, 1.000000000000000000, 0.9898214418809326842, 1.000000000000000000, 0.9898214418809326842, 1.000000000000000000, 0.9898214418809326842, 1.000000000000000000, 0.9898214418809326842, 1.000000000000000000, 0.9898214418809326842, 1.000000000000000000, 0.9898214418809326842, 1.000000000000000000, 0.9898214418809326842, 1.000000000000000000, 0.9898214418809326842, 1.000000000000000000, 0.9898214418809326842, 1.000000000000000000, 0.9898214418809326842, 1.000000000000000000, 0.9898214418809326842, 1.000000000000000000, 0.9898214418809326842, 1.000000000000000000, 0.9898214418809326842, 1.000000000000000000, 0.9898214418809326842, 1.000000000000000000, 0.9898214418809326842, 1.000000000000000000, 0.9898214418809326842, 1.000000000000000000, 0.9898214418809326842, 1.000000000000000000, 0.9898214418809326842, 1.000000000000000000, 0.9898214418809326842, 1.000000000000000000, 0.9898214418809326842, 1.000000000000000000, 0.9898214418809326842, 1.000000000000000000, 0.9898214418809326842, 1.000000000000000000, 0.9898214418809326842, 1.000000000000000000, 0.9898214418809326842, 1.000000000000000000, 0.9898214418809326842, 1.000000000000000000, 0.9898214418809326842, 1.000000000000000000, 0.9898214418809326842, 1.000000000000000000, 0.9898214418809326842, 1.000000000000000000, 0.9898214418809326842, 1.000000000000000000, 0.9898214418809326842, 1.000000000000000000, 0.9898214418809326842, 1.000000000000000000, 0.9898214418809326842, 1.000000000000000000, 0.9898214418809326842, 1.000000000000000000, 0.9898214418809326842, 1.000000000000000000, 0.9898214418809326842, 1.000000000000000000, 0.9898214418809326842, 1.000000000000000000, 0.9898214418809326842, 1.000000000000000000, 0.9898214418809326842, 1.000000000000000000, 0.9898214418809326842, 1.000000000000000000, 0.9898214418809326842, 1.000000000000000000, 0.9898214418809326842, 1.000000000000000000, 0.9898214418809326842, 1.000000000000000000, 0.9898214418809326842, 1.000000000000000000, 0.9898214418809326842, 1.000000000000000000, 0.9898214418809326842, 1.000000000000000000, 0.9898214418809326842, 1.000000000000000000, 0.9898214418809326842, 1.000000000000000000, 0.9898214418809326842, 1.000000000000000000, 0.9898214418809326842, 1.000000000000000000, 0.9898214418809326842, 1.000000000000000000, 0.9898214418809326842, 1.000000000000000000, 0.9898214418809326842, 1.000000000000000000, 0.9898214418809326842, 1.000000000000000000, 0.9898214418809326842, 1.000000000000000000, 0.9898214418809326842, 1.000000000000000000, 0.9898214418809326842, 1.000000000000000000, 0.9898214418809326842, 1.000000000000000000, 0.9898214418809326842, 1.000000000000000000, 0.9898214418809326842, 1.000000000000000000, 0.9898214418809326842, 1.000000000000000000, 0.9898214418809326842, 1.000000000000000000, 0.9898214418809326842, 1.000000000000000000, 0.9898214418809326842, 1.000000000000000000, 0.9898214418809326842, 1.000000000000000000, 0.9898214418809326842, 1.000000000000000000, 0.9898214418809326842, 1.000000000000000000, 0.9898214418809326842, 1.000000000000000000, 0.9898214418809326842, 1.000000000000000000, 0.9898214418809326842, 1.000000000000000000, 0.9898214418809326842, 1.000000000000000000, 0.9898214418809326842, 1.000000000000000000, 0.9898214418809326842, 1.000000000000000000, 0.9898214418809326842, 1.000000000000000000, 0.9898214418809326842, 1.000000000000000000, 0.9898214418809326842, 1.000000000000000000, 0.9898214418809326842, 1.000000000000000000, 0.9898214418809326842, 1.000000000000000000, 0.9898214418809326842, 1.000000000000000000, 0.9898214418809326842, 1.000000000000000000, 0.9898214418809326842, 1.000000000000000000, 0.9898214418809326842, 1.000000000000000000, 0.9898214418809326842, 1.000000000000000000, 0.9898214418809326842, 1.000000000000000000, 0.9898214418809326842, 1.000000000000000000, 0.9898214418809326842, 1.000000000000000000, 0.9898214418809326842, 1.000000000000000000, 0.9898214418809326842, 1.000000000000000000, 0.9898214418809326842, 1.000000000000000000, 0.9898214418809326842, 1.000000000000000000, 0.9898214418809326842, 1.000000000000000000, 0.9898214418809326842, 1.000000000000000000, 0.9898214418809326842, 1.000000000000000000, 0.9898214418809326842, 1.000000000000000000, 0.9898214418809326842, 1.000000000000000000, 0.9898214418809326842, 1.000000000000000000, 0.9898214418809326842, 1.000000000000000000, 0.9898214418809326842, 1.000000000000000000, 0.9898214418809326842, 1.000000000000000000, 0.9898214418809326842, 1.000000000000000000, 0.9898214418809326842, 1.000000000000000000, 0.9898214418809326842, 1.000000000000000000, 0.9898214418809326842, 1.000000000000000000, 0.9898214418809326842, 1.000000000000000000, 0.9898214418809326842, 1.000000000000000000, 0.9898214418809326842, 1.000000000000000000, 0.9898214418809326842, 1.000000000000000000, 0.9898214418809326842, 1.000000000000000000, 0.9898214418809326842, 1.000000000000000000, 0.9898214418809326842, 1.000000000000000000, 0.9898214418809326842, 1.000000000000000000, 0.9898214418809326842, 1.000000000000000000, 0.9898214418809326842, 1.000000000000000000, 0.9898214418809326842, 1.000000000000000000, 0.9898214418809326842, 1.000000000000000000, 0.9898214418809326842, 1.000000000000000000, 0.9898214418809326842, 1.000000000000000000, 0.9898214418809326842, 1.000000000000000000, 0.9898214418809326842, 1.000000000000000000, 0.9898214418809326842, 1.000000000000000000, 0.9898214418809326842, 1.000000000000000000, 0.9898214418809326842, 1.000000000000000000, 0.9898214418809326842, 1.000000000000000000, 0.9898214418809326842, 1.000000000000000000, 0.9898214418809326842, 1.000000000000000000, 0.9898214418809326842, 1.000000000000000000, 0.9898214418809326842, 1.000000000000000000, 0.9898214418809326842, 1.000000000000000000, 0.9898214418809326842, 1.000000000000000000, 0.9898214418809326842, 1.000000000000000000, 0.9898214418809326842, 1.000000000000000000, 0.9898214418809326842, 1.000000000000000000, 0.9898214418809326842, 1.000000000000000000, 0.9898214418809326842, 1.000000000000000000, 0.9898214418809326842, 1.000000000000000000, 0.9898214418809326842, 1.000000000000000000, 0.9898214418809326842, 1.000000000000000000, 0.9898214418809326842, 1.000000000000000000, 0.9898214418809326842, 1.000000000000000000, 0.9898214418809326842, 1.000000000000000000, 0.9898214418809326842, 1.000000000000000000, 0.9898214418809326842, 1.000000000000000000, 0.9898214418809326842, 1.000000000000000000, 0.9898214418809326842, 1.000000000000000000, 0.9898214418809326842, 1.000000000000000000, 0.9898214418809326842, 1.000000000000000000, 0.9898214418809326842, 1.000000000000000000, 0.9898214418809326842, 1.000000000000000000, 0.9898214418809326842, 1.000000000000000000, 0.9898214418809326842, 1.000000000000000000, 0.9898214418809326842, 1.000000000000000000, 0.9898214418809326842, 1.000000000000000000, 0.9898214418809326842, 1.000000000000000000, 0.9898214418809326842, 1.000000000000000000, 0.9898214418809326842, 1.000000000000000000, 0.9898214418809326842, 1.000000000000000000, 0.9898214418809326842, 1.000000000000000000, 0.9898214418809326842, 1.000000000000000000, 0.9898214418809326842, 1.000000000000000000, 0.9898214418809326842, 1.000000000000000000, 0.9898214418809326842, 1.000000000000000000, 0.9898214418809326842, 1.000000000000000000, 0.9898214418809326842, 1.000000000000000000, 0.9898214418809326842, 1.000000000000000000, 0.9898214418809326842, 1.000000000000000000, 0.9898214418809326842, 1.000000000000000000, 0.9898214418809326842, 1.000000000000000000, 0.9898214418809326842, 1.000000000000000000, 0.9898214418809326842, 1.000000000000000000, 0.9898214418809326842, 1.000000000000000000, 0.9898214418809326842, 1.000000000000000000, 0.9898214418809326842, 1.000000000000000000, 0.9898214418809326842, 1.000000000000000000, 0.9898214418809326842, 1.000000000000000000, 0.9898214418809326842, 1.000000000000000000, 0.9898214418809326842, 1.000000000000000000, 0.9898214418809326842, 1.000000000000000000, 0.9898214418809326842, 1.000000000000000000, 0.9898214418809326842, 1.000000000000000000, 0.9898214418809326842, 1.000000000000000000, 0.9898214418809326842, 1.000000000000000000, 0.9898214418809326842, 1.000000000000000000, 0.9898214418809326842, 1.000000000000000000, 0.9898214418809326842, 1.000000000000000000, 0.9898214418809326842, 1.000000000000000000, 0.9898214418809326842, 1.000000000000000000, 0.9898214418809326842, 1.000000000000000000, 0.9898214418809326842, 1.000000000000000000, 0.9898214418809326842, 1.000000000000000000, 0.9898214418809326842, 1.000000000000000000, 0.9898214418809326842, 1.000000000000000000, 0.9898214418809326842, 1.000000000000000000, 0.9898214418809326842, 1.000000000000000000, 0.9898214418809326842, 1.000000000000000000, 0.9898214418809326842, 1.000000000000000000, 0.9898214418809326842, 1.000000000000000000, 0.9898214418809326842, 1.000000000000000000, 0.9898214418809326842, 1.000000000000000000, 0.9898214418809326842, 1.000000000000000000, 0.9898214418809326842, 1.000000000000000000, 0.9898214418809326842, 1.000000000000000000, 0.9898214418809326842, 1.000000000000000000, 0.9898214418809326842, 1.000000000000000000, 0.9898214418809326842, 1.000000000000000000, 0.9898214418809326842, 1.000000000000000000, 0.9898214418809326842, 1.000000000000000000, 0.9898214418809326842, 1.000000000000000000, 0.9898214418809326842, 1.000000000000000000, 0.9898214418809326842, 1.000000000000000000, 0.9898214418809326842, 1.000000000000000000, 0.9898214418809326842, 1.000000000000000000, 0.9898214418809326842, 1.000000000000000000, 0.9898214418809326842, 1.000000000000000000, 0.9898214418809326842, 1.000000000000000000, 0.9898214418809326842, 1.000000000000000000, 0.9898214418809326842, 1.000000000000000000, 0.9898214418809326842, 1.000000000000000000, 0.9898214418809326842, 1.000000000000000000, 0.9898214418809326842, 1.000000000000000000, 0.9898214418809326842, 1.000000000000000000, 0.9898214418809326842, 1.000000000000000000, 0.9898214418809326842, 1.000000000000000000, 0.9898214418809326842, 1.000000000000000000, 0.9898214418809326842, 1.000000000000000000, 0.9898214418809326842, 1.000000000000000000, 0.9898214418809326842, 1.000000000000000000, 0.9898214418809326842, 1.000000000000000000, 0.9898214418809326842, 1.000000000000000000, 0.9898214418809326842, 1.000000000000000000, 0.9898214418809326842, 1.000000000000000000, 0.9898214418809326842, 1.000000000000000000, 0.9898214418809326842, 1.000000000000000000, 0.9898214418809326842, 1.000000000000000000, 0.9898214418809326842, 1.000000000000000000, 0.9898214418809326842, 1.000000000000000000, 0.9898214418809326842, 1.000000000000000000, 0.9898214418809326842, 1.000000000000000000, 0.9898214418809326842, 1.000000000000000000, 0.9898214418809326842, 1.000000000000000000, 0.9898214418809326842, 1.000000000000000000, 0.9898214418809326842, 1.000000000000000000, 0.9898214418809326842, 1.000000000000000000, 0.9898214418809326842, 1.000000000000000000, 0.9898214418809326842, 1.000000000000000000, 0.9898214418809326842, 1.000000000000000000, 0.9898214418809326842, 1.000000000000000000, 0.9898214418809326842, 1.000000000000000000, 0.9898214418809326842, 1.000000000000000000, 0.9898214418809326842, 1.000000000000000000, 0.9898214418809326842, 1.000000000000000000, 0.9898214418809326842, 1.000000000000000000, 0.9898214418809326842, 1.000000000000000000, 0.9898214418809326842, 1.000000000000000000, 0.9898214418809326842, 1.000000000000000000, 0.9898214418809326842, 1.000000000000000000, 0.9898214418809326842, 1.000000000000000000, 0.9898214418809326842, 1.000000000000000000, 0.9898214418809326842, 1.000000000000000000, 0.9898214418809326842, 1.000000000000000000, 0.9898214418809326842, 1.000000000000000000, 0.9898214418809326842, 1.000000000000000000, 0.9898214418809326842, 1.000000000000000000, 0.9898214418809326842, 1.000000000000000000, 0.9898214418809326842, 1.000000000000000000, 0.9898214418809326842, 1.000000000000000000, 0.9898214418809326842, 1.000000000000000000, 0.9898214418809326842, 1.000000000000000000, 0.9898214418809326842, 1.000000000000000000, 0.9898214418809326842, 1.000000000000000000, 0.9898214418809326842, 1.000000000000000000, 0.9898214418809326842, 1.000000000000000000, 0.9898214418809326842, 1.000000000000000000, 0.9898214418809326842, 1.000000000000000000, 0.9898214418809326842, 1.000000000000000000, 0.9898214418809326842, 1.000000000000000000, 0.9898214418809326842, 1.000000000000000000, 0.9898214418809326842, 1.000000000000000000, 0.9898214418809326842, 1.000000000000000000, 0.9898214418809326842, 1.000000000000000000, 0.9898214418809326842, 1.000000000000000000, 0.9898214418809326842, 1.000000000000000000, 0.9898214418809326842, 1.000000000000000000, 0.9898214418809326842, 1.000000000000000000, 0.9898214418809326842, 1.000000000000000000, 0.9898214418809326842, 1.000000000000000000, 0.9898214418809326842, 1.000000000000000000, 0.9898214418809326842, 1.000000000000000000, 0.9898214418809326842, 1.000000000000000000, 0.9898214418809326842, 1.000000000000000000, 0.9898214418809326842, 1.000000000000000000, 0.9898214418809326842, 1.000000000000000000, 0.9898214418809326842, 1.000000000000000000, 0.9898214418809326842, 1.000000000000000000, 0.9898214418809326842, 1.000000000000000000, 0.9898214418809326842, 1.000000000000000000, 0.9898214418809326842, 1.000000000000000000, 0.9898214418809326842, 1.000000000000000000, 0.9898214418809326842, 1.000000000000000000, 0.9898214418809326842, 1.000000000000000000, 0.9898214418809326842, 1.000000000000000000, 0.9898214418809326842, 1.000000000000000000, 0.9898214418809326842, 1.000000000000000000, 0.9898214418809326842, 1.000000000000000000, 0.9898214418809326842, 1.000000000000000000, 0.9898214418809326842, 1.000000000000000000, 0.9898214418809326842, 1.000000000000000000, 0.9898214418809326842, 1.000000000000000000, 0.9898214418809326842, 1.000000000000000000, 0.9898214418809326842, 1.000000000000000000, 0.9898214418809326842, 1.000000000000000000, 0.9898214418809326842, 1.000000000000000000, 0.9898214418809326842, 1.000000000000000000, 0.9898214418809326842, 1.000000000000000000, 0.9898214418809326842, 1.000000000000000000, 0.9898214418809326842, 1.000000000000000000, 0.9898214418809326842, 1.000000000000000000, 0.9898214418809326842, 1.000000000000000000, 0.9898214418809326842, 1.000000000000000000, 0.9898214418809326842, 1.000000000000000000, 0.9898214418809326842, 1.000000000000000000, 0.9898214418809326842, 1.000000000000000000, 0.9898214418809326842, 1.000000000000000000, 0.9898214418809326842, 1.000000000000000000, 0.9898214418809326842, 1.000000000000000000, 0.9898214418809326842, 1.000000000000000000, 0.9898214418809326842, 1.000000000000000000, 0.9898214418809326842, 1.000000000000000000, 0.9898214418809326842, 1.000000000000000000, 0.9898214418809326842, 1.000000000000000000, 0.9898214418809326842, 1.000000000000000000, 0.9898214418809326842, 1.000000000000000000, 0.9898214418809326842, 1.000000000000000000, 0.9898214418809326842, 1.000000000000000000, 0.9898214418809326842, 1.000000000000000000, 0.9898214418809326842, 1.000000000000000000, 0.9898214418809326842, 1.000000000000000000, 0.9898214418809326842, 1.000000000000000000, 0.9898214418809326842, 1.000000000000000000, 0.9898214418809326842, 1.000000000000000000, 0.9898214418809326842, 1.000000000000000000, 0.9898214418809326842, 1.000000000000000000, 0.9898214418809326842, 1.000000000000000000, 0.9898214418809326842, 1.000000000000000000, 0.9898214418809326842, 1.000000000000000000, 0.9898214418809326842, 1.000000000000000000, 0.9898214418809326842, 1.000000000000000000, 0.9898214418809326842, 1.000000000000000000, 0.9898214418809326842, 1.000000000000000000, 0.9898214418809326842, 1.000000000000000000, 0.9898214418809326842, 1.000000000000000000, 0.9898214418809326842, 1.000000000000000000, 0.9898214418809326842, 1.000000000000000000, 0.9898214418809326842, 1.000000000000000000, 0.9898214418809326842, 1.000000000000000000, 0.9898214418809326842, 1.000000000000000000, 0.9898214418809326842, 1.000000000000000000, 0.9898214418809326842, 1.000000000000000000, 0.9898214418809326842, 1.000000000000000000, 0.9898214418809326842, 1.000000000000000000, 0.9898214418809326842, 1.000000000000000000, 0.9898214418809326842, 1.000000000000000000, 0.9898214418809326842, 1.000000000000000000, 0.9898214418809326842, 1.000000000000000000, 0.9898214418809326842, 1.000000000000000000, 0.9898214418809326842, 1.000000000000000000, 0.9898214418809326842, 1.000000000000000000, 0.9898214418809326842, 1.000000000000000000, 0.9898214418809326842, 1.000000000000000000, 0.9898214418809326842, 1.000000000000000000, 0.9898214418809326842, 1.000000000000000000, 0.9898214418809326842, 1.000000000000000000, 0.9898214418809326842, 1.000000000000000000, 0.9898214418809326842, 1.000000000000000000, 0.9898214418809326842, 1.000000000000000000, 0.9898214418809326842, 1.000000000000000000, 0.9898214418809326842, 1.000000000000000000, 0.9898214418809326842, 1.000000000000000000, 0.9898214418809326842, 1.000000000000000000, 0.9898214418809326842, 1.000000000000000000, 0.9898214418809326842, 1.000000000000000000, 0.9898214418809326842, 1.000000000000000000, 0.9898214418809326842, 1.000000000000000000, 0.9898214418809326842, 1.000000000000000000, 0.9898214418809326842, 1.000000000000000000, 0.9898214418809326842, 1.000000000000000000, 0.9898214418809326842, 1.000000000000000000, 0.9898214418809326842, 1.000000000000000000, 0.9898214418809326842, 1.000000000000000000, 0.9898214418809326842, 1.000000000000000000, 0.9898214418809326842, 1.000000000000000000, 0.9898214418809326842, 1.000000000000000000, 0.9898214418809326842, 1.000000000000000000, 0.9898214418809326842, 1.000000000000000000, 0.9898214418809326842, 1.000000000000000000, 0.9898214418809326842, 1.000000000000000000, 0.9898214418809326842, 1.000000000000000000, 0.9898214418809326842, 1.000000000000000000, 0.9898214418809326842, 1.000000000000000000, 0.9898214418809326842, 1.000000000000000000, 0.9898214418809326842, 1.000000000000000000, 0.9898214418809326842, 1.000000000000000000, 0.9898214418809326842, 1.000000000000000000, 0.9898214418809326842, 1.000000000000000000, 0.9898214418809326842, 1.000000000000000000, 0.9898214418809326842, 1.000000000000000000, 0.9898214418809326842, 1.000000000000000000, 0.9898214418809326842, 1.000000000000000000, 0.9898214418809326842, 1.000000000000000000, 0.9961809353924466759, 0.9952277490961531914),
 ( 0.3333333333333333703, 0.3299404806269776169, 0.3333333333333333703, 0.3299404806269776169, 0.3333333333333333703, 0.3299404806269776169, 0.3333333333333333703, 0.3299404806269776169, 0.3333333333333333703, 0.3299404806269776169, 0.3333333333333333703, 0.3299404806269776169, 0.3333333333333333703, 0.3299404806269776169, 0.3333333333333333703, 0.3299404806269776169, 0.3333333333333333703, 0.3299404806269776169, 0.3333333333333333703, 0.3299404806269776169, 0.3333333333333333703, 0.3299404806269776169, 0.3333333333333333703, 0.3299404806269776169, 0.3333333333333333703, 0.3299404806269776169, 0.3333333333333333703, 0.3299404806269776169, 0.3333333333333333703, 0.3299404806269776169, 0.3333333333333333703, 0.3299404806269776169, 0.3333333333333333703, 0.3299404806269776169, 0.3333333333333333703, 0.3299404806269776169, 0.3333333333333333703, 0.3299404806269776169, 0.3333333333333333703, 0.3299404806269776169, 0.3333333333333333703, 0.3299404806269776169, 0.3333333333333333703, 0.3299404806269776169, 0.3333333333333333703, 0.3299404806269776169, 0.3333333333333333703, 0.3299404806269776169, 0.3333333333333333703, 0.3299404806269776169, 0.3333333333333333703, 0.3299404806269776169, 0.3333333333333333703, 0.3299404806269776169, 0.3333333333333333703, 0.3299404806269776169, 0.3333333333333333703, 0.3299404806269776169, 0.3333333333333333703, 0.3299404806269776169, 0.3333333333333333703, 0.3299404806269776169, 0.3333333333333333703, 0.3299404806269776169, 0.3333333333333333703, 0.3299404806269776169, 0.3333333333333333703, 0.3299404806269776169, 0.3333333333333333703, 0.3299404806269776169, 0.3333333333333333703, 0.3299404806269776169, 0.3333333333333333703, 0.3299404806269776169, 0.3333333333333333703, 0.3299404806269776169, 0.3333333333333333703, 0.3299404806269776169, 0.3333333333333333703, 0.3299404806269776169, 0.3333333333333333703, 0.3299404806269776169, 0.3333333333333333703, 0.3299404806269776169, 0.3333333333333333703, 0.3299404806269776169, 0.3333333333333333703, 0.3299404806269776169, 0.3333333333333333703, 0.3299404806269776169, 0.3333333333333333703, 0.3299404806269776169, 0.3333333333333333703, 0.3299404806269776169, 0.3333333333333333703, 0.3299404806269776169, 0.3333333333333333703, 0.3299404806269776169, 0.3333333333333333703, 0.3299404806269776169, 0.3333333333333333703, 0.3299404806269776169, 0.3333333333333333703, 0.3299404806269776169, 0.3333333333333333703, 0.3299404806269776169, 0.3333333333333333703, 0.3299404806269776169, 0.3333333333333333703, 0.3299404806269776169, 0.3333333333333333703, 0.3299404806269776169, 0.3333333333333333703, 0.3299404806269776169, 0.3333333333333333703, 0.3299404806269776169, 0.3333333333333333703, 0.3299404806269776169, 0.3333333333333333703, 0.3299404806269776169, 0.3333333333333333703, 0.3299404806269776169, 0.3333333333333333703, 0.3299404806269776169, 0.3333333333333333703, 0.3299404806269776169, 0.3333333333333333703, 0.3299404806269776169, 0.3333333333333333703, 0.3299404806269776169, 0.3333333333333333703, 0.3299404806269776169, 0.3333333333333333703, 0.3299404806269776169, 0.3333333333333333703, 0.3299404806269776169, 0.3333333333333333703, 0.3299404806269776169, 0.3333333333333333703, 0.3299404806269776169, 0.3333333333333333703, 0.3299404806269776169, 0.3333333333333333703, 0.3299404806269776169, 0.3333333333333333703, 0.3299404806269776169, 0.3333333333333333703, 0.3299404806269776169, 0.3333333333333333703, 0.3299404806269776169, 0.3333333333333333703, 0.3299404806269776169, 0.3333333333333333703, 0.3299404806269776169, 0.3333333333333333703, 0.3299404806269776169, 0.3333333333333333703, 0.3299404806269776169, 0.3333333333333333703, 0.3299404806269776169, 0.3333333333333333703, 0.3299404806269776169, 0.3333333333333333703, 0.3299404806269776169, 0.3333333333333333703, 0.3299404806269776169, 0.3333333333333333703, 0.3299404806269776169, 0.3333333333333333703, 0.3299404806269776169, 0.3333333333333333703, 0.3299404806269776169, 0.3333333333333333703, 0.3299404806269776169, 0.3333333333333333703, 0.3299404806269776169, 0.3333333333333333703, 0.3299404806269776169, 0.3333333333333333703, 0.3299404806269776169, 0.3333333333333333703, 0.3299404806269776169, 0.3333333333333333703, 0.3299404806269776169, 0.3333333333333333703, 0.3299404806269776169, 0.3333333333333333703, 0.3299404806269776169, 0.3333333333333333703, 0.3299404806269776169, 0.3333333333333333703, 0.3299404806269776169, 0.3333333333333333703, 0.3299404806269776169, 0.3333333333333333703, 0.3299404806269776169, 0.3333333333333333703, 0.3299404806269776169, 0.3333333333333333703, 0.3299404806269776169, 0.3333333333333333703, 0.3299404806269776169, 0.3333333333333333703, 0.3299404806269776169, 0.3333333333333333703, 0.3299404806269776169, 0.3333333333333333703, 0.3299404806269776169, 0.3333333333333333703, 0.3299404806269776169, 0.3333333333333333703, 0.3299404806269776169, 0.3333333333333333703, 0.3299404806269776169, 0.3333333333333333703, 0.3299404806269776169, 0.3333333333333333703, 0.3299404806269776169, 0.3333333333333333703, 0.3299404806269776169, 0.3333333333333333703, 0.3299404806269776169, 0.3333333333333333703, 0.3299404806269776169, 0.3333333333333333703, 0.3299404806269776169, 0.3333333333333333703, 0.3299404806269776169, 0.3333333333333333703, 0.3299404806269776169, 0.3333333333333333703, 0.3299404806269776169, 0.3333333333333333703, 0.3299404806269776169, 0.3333333333333333703, 0.3299404806269776169, 0.3333333333333333703, 0.3299404806269776169, 0.3333333333333333703, 0.3299404806269776169, 0.3333333333333333703, 0.3299404806269776169, 0.3333333333333333703, 0.3299404806269776169, 0.3333333333333333703, 0.3299404806269776169, 0.3333333333333333703, 0.3299404806269776169, 0.3333333333333333703, 0.3299404806269776169, 0.3333333333333333703, 0.3299404806269776169, 0.3333333333333333703, 0.3299404806269776169, 0.3333333333333333703, 0.3299404806269776169, 0.3333333333333333703, 0.3299404806269776169, 0.3333333333333333703, 0.3299404806269776169, 0.3333333333333333703, 0.3299404806269776169, 0.3333333333333333703, 0.3299404806269776169, 0.3333333333333333703, 0.3299404806269776169, 0.3333333333333333703, 0.3299404806269776169, 0.3333333333333333703, 0.3299404806269776169, 0.3333333333333333703, 0.3299404806269776169, 0.3333333333333333703, 0.3299404806269776169, 0.3333333333333333703, 0.3299404806269776169, 0.3333333333333333703, 0.3299404806269776169, 0.3333333333333333703, 0.3299404806269776169, 0.3333333333333333703, 0.3299404806269776169, 0.3333333333333333703, 0.3299404806269776169, 0.3333333333333333703, 0.3299404806269776169, 0.3333333333333333703, 0.3299404806269776169, 0.3333333333333333703, 0.3299404806269776169, 0.3333333333333333703, 0.3299404806269776169, 0.3333333333333333703, 0.3299404806269776169, 0.3333333333333333703, 0.3299404806269776169, 0.3333333333333333703, 0.3299404806269776169, 0.3333333333333333703, 0.3299404806269776169, 0.3333333333333333703, 0.3299404806269776169, 0.3333333333333333703, 0.3299404806269776169, 0.3333333333333333703, 0.3299404806269776169, 0.3333333333333333703, 0.3299404806269776169, 0.3333333333333333703, 0.3299404806269776169, 0.3333333333333333703, 0.3299404806269776169, 0.3333333333333333703, 0.3299404806269776169, 0.3333333333333333703, 0.3299404806269776169, 0.3333333333333333703, 0.3299404806269776169, 0.3333333333333333703, 0.3299404806269776169, 0.3333333333333333703, 0.3299404806269776169, 0.3333333333333333703, 0.3299404806269776169, 0.3333333333333333703, 0.3299404806269776169, 0.3333333333333333703, 0.3299404806269776169, 0.3333333333333333703, 0.3299404806269776169, 0.3333333333333333703, 0.3299404806269776169, 0.3333333333333333703, 0.3299404806269776169, 0.3333333333333333703, 0.3299404806269776169, 0.3333333333333333703, 0.3299404806269776169, 0.3333333333333333703, 0.3299404806269776169, 0.3333333333333333703, 0.3299404806269776169, 0.3333333333333333703, 0.3299404806269776169, 0.3333333333333333703, 0.3299404806269776169, 0.3333333333333333703, 0.3299404806269776169, 0.3333333333333333703, 0.3299404806269776169, 0.3333333333333333703, 0.3299404806269776169, 0.3333333333333333703, 0.3299404806269776169, 0.3333333333333333703, 0.3299404806269776169, 0.3333333333333333703, 0.3299404806269776169, 0.3333333333333333703, 0.3299404806269776169, 0.3333333333333333703, 0.3299404806269776169, 0.3333333333333333703, 0.3299404806269776169, 0.3333333333333333703, 0.3299404806269776169, 0.3333333333333333703, 0.3299404806269776169, 0.3333333333333333703, 0.3299404806269776169, 0.3333333333333333703, 0.3299404806269776169, 0.3333333333333333703, 0.3299404806269776169, 0.3333333333333333703, 0.3299404806269776169, 0.3333333333333333703, 0.3299404806269776169, 0.3333333333333333703, 0.3299404806269776169, 0.3333333333333333703, 0.3299404806269776169, 0.3333333333333333703, 0.3299404806269776169, 0.3333333333333333703, 0.3299404806269776169, 0.3333333333333333703, 0.3299404806269776169, 0.3333333333333333703, 0.3299404806269776169, 0.3333333333333333703, 0.3299404806269776169, 0.3333333333333333703, 0.3299404806269776169, 0.3333333333333333703, 0.3299404806269776169, 0.3333333333333333703, 0.3299404806269776169, 0.3333333333333333703, 0.3299404806269776169, 0.3333333333333333703, 0.3299404806269776169, 0.3333333333333333703, 0.3299404806269776169, 0.3333333333333333703, 0.3299404806269776169, 0.3333333333333333703, 0.3299404806269776169, 0.3333333333333333703, 0.3299404806269776169, 0.3333333333333333703, 0.3299404806269776169, 0.3333333333333333703, 0.3299404806269776169, 0.3333333333333333703, 0.3299404806269776169, 0.3333333333333333703, 0.3299404806269776169, 0.3333333333333333703, 0.3299404806269776169, 0.3333333333333333703, 0.3299404806269776169, 0.3333333333333333703, 0.3299404806269776169, 0.3333333333333333703, 0.3299404806269776169, 0.3333333333333333703, 0.3299404806269776169, 0.3333333333333333703, 0.3299404806269776169, 0.3333333333333333703, 0.3299404806269776169, 0.3333333333333333703, 0.3299404806269776169, 0.3333333333333333703, 0.3299404806269776169, 0.3333333333333333703, 0.3299404806269776169, 0.3333333333333333703, 0.3299404806269776169, 0.3333333333333333703, 0.3299404806269776169, 0.3333333333333333703, 0.3299404806269776169, 0.3333333333333333703, 0.3299404806269776169, 0.3333333333333333703, 0.3299404806269776169, 0.3333333333333333703, 0.3299404806269776169, 0.3333333333333333703, 0.3299404806269776169, 0.3333333333333333703, 0.3299404806269776169, 0.3333333333333333703, 0.3299404806269776169, 0.3333333333333333703, 0.3299404806269776169, 0.3333333333333333703, 0.3299404806269776169, 0.3333333333333333703, 0.3299404806269776169, 0.3333333333333333703, 0.3299404806269776169, 0.3333333333333333703, 0.3299404806269776169, 0.3333333333333333703, 0.3299404806269776169, 0.3333333333333333703, 0.3299404806269776169, 0.3333333333333333703, 0.3299404806269776169, 0.3333333333333333703, 0.3299404806269776169, 0.3333333333333333703, 0.3299404806269776169, 0.3333333333333333703, 0.3299404806269776169, 0.3333333333333333703, 0.3299404806269776169, 0.3333333333333333703, 0.3299404806269776169, 0.3333333333333333703, 0.3299404806269776169, 0.3333333333333333703, 0.3299404806269776169, 0.3333333333333333703, 0.3299404806269776169, 0.3333333333333333703, 0.3299404806269776169, 0.3333333333333333703, 0.3299404806269776169, 0.3333333333333333703, 0.3299404806269776169, 0.3333333333333333703, 0.3299404806269776169, 0.3333333333333333703, 0.3299404806269776169, 0.3333333333333333703, 0.3299404806269776169, 0.3333333333333333703, 0.3299404806269776169, 0.3333333333333333703, 0.3299404806269776169, 0.3333333333333333703, 0.3299404806269776169, 0.3333333333333333703, 0.3299404806269776169, 0.3333333333333333703, 0.3299404806269776169, 0.3333333333333333703, 0.3299404806269776169, 0.3333333333333333703, 0.3299404806269776169, 0.3333333333333333703, 0.3299404806269776169, 0.3333333333333333703, 0.3299404806269776169, 0.3333333333333333703, 0.3299404806269776169, 0.3333333333333333703, 0.3299404806269776169, 0.3333333333333333703, 0.3299404806269776169, 0.3333333333333333703, 0.3299404806269776169, 0.3333333333333333703, 0.3299404806269776169, 0.3333333333333333703, 0.3299404806269776169, 0.3333333333333333703, 0.3299404806269776169, 0.3333333333333333703, 0.3299404806269776169, 0.3333333333333333703, 0.3299404806269776169, 0.3333333333333333703, 0.3299404806269776169, 0.3333333333333333703, 0.3299404806269776169, 0.3333333333333333703, 0.3299404806269776169, 0.3333333333333333703, 0.3299404806269776169, 0.3333333333333333703, 0.3299404806269776169, 0.3333333333333333703, 0.3299404806269776169, 0.3333333333333333703, 0.3299404806269776169, 0.3333333333333333703, 0.3299404806269776169, 0.3333333333333333703, 0.3299404806269776169, 0.3333333333333333703, 0.3299404806269776169, 0.3333333333333333703, 0.3299404806269776169, 0.3333333333333333703, 0.3299404806269776169, 0.3333333333333333703, 0.3299404806269776169, 0.3333333333333333703, 0.3299404806269776169, 0.3333333333333333703, 0.3299404806269776169, 0.3333333333333333703, 0.3299404806269776169, 0.3333333333333333703, 0.3299404806269776169, 0.3333333333333333703, 0.3299404806269776169, 0.3333333333333333703, 0.3299404806269776169, 0.3333333333333333703, 0.3299404806269776169, 0.3333333333333333703, 0.3299404806269776169, 0.3333333333333333703, 0.3299404806269776169, 0.3333333333333333703, 0.3299404806269776169, 0.3333333333333333703, 0.3299404806269776169, 0.3333333333333333703, 0.3299404806269776169, 0.3333333333333333703, 0.3299404806269776169, 0.3333333333333333703, 0.3299404806269776169, 0.3333333333333333703, 0.3299404806269776169, 0.3333333333333333703, 0.3299404806269776169, 0.3333333333333333703, 0.3299404806269776169, 0.3333333333333333703, 0.3299404806269776169, 0.3333333333333333703, 0.3299404806269776169, 0.3333333333333333703, 0.3299404806269776169, 0.3333333333333333703, 0.3299404806269776169, 0.3333333333333333703, 0.3299404806269776169, 0.3333333333333333703, 0.3299404806269776169, 0.3333333333333333703, 0.3299404806269776169, 0.3333333333333333703, 0.3299404806269776169, 0.3333333333333333703, 0.3299404806269776169, 0.3333333333333333703, 0.3299404806269776169, 0.3333333333333333703, 0.3299404806269776169, 0.3333333333333333703, 0.3299404806269776169, 0.3333333333333333703, 0.3299404806269776169, 0.3333333333333333703, 0.3299404806269776169, 0.3333333333333333703, 0.3299404806269776169, 0.3333333333333333703, 0.3299404806269776169, 0.3333333333333333703, 0.3299404806269776169, 0.3333333333333333703, 0.3299404806269776169, 0.3333333333333333703, 0.3299404806269776169, 0.3333333333333333703, 0.3299404806269776169, 0.3333333333333333703, 0.3299404806269776169, 0.3333333333333333703, 0.3299404806269776169, 0.3333333333333333703, 0.3299404806269776169, 0.3333333333333333703, 0.3299404806269776169, 0.3333333333333333703, 0.3299404806269776169, 0.3333333333333333703, 0.3299404806269776169, 0.3333333333333333703, 0.3299404806269776169, 0.3333333333333333703, 0.3299404806269776169, 0.3333333333333333703, 0.3299404806269776169, 0.3333333333333333703, 0.3299404806269776169, 0.3333333333333333703, 0.3299404806269776169, 0.3333333333333333703, 0.3299404806269776169, 0.3333333333333333703, 0.3299404806269776169, 0.3333333333333333703, 0.3299404806269776169, 0.3333333333333333703, 0.3299404806269776169, 0.3333333333333333703, 0.3299404806269776169, 0.3333333333333333703, 0.3299404806269776169, 0.3333333333333333703, 0.3299404806269776169, 0.3333333333333333703, 0.3299404806269776169, 0.3333333333333333703, 0.3299404806269776169, 0.3333333333333333703, 0.3299404806269776169, 0.3333333333333333703, 0.3299404806269776169, 0.3333333333333333703, 0.3299404806269776169, 0.3333333333333333703, 0.3299404806269776169, 0.3333333333333333703, 0.3299404806269776169, 0.3333333333333333703, 0.3299404806269776169, 0.3333333333333333703, 0.3299404806269776169, 0.3333333333333333703, 0.3299404806269776169, 0.3333333333333333703, 0.3299404806269776169, 0.3333333333333333703, 0.3299404806269776169, 0.3333333333333333703, 0.3299404806269776169, 0.3333333333333333703, 0.3299404806269776169, 0.3333333333333333703, 0.3299404806269776169, 0.3333333333333333703, 0.3299404806269776169, 0.3333333333333333703, 0.3299404806269776169, 0.3333333333333333703, 0.3299404806269776169, 0.3333333333333333703, 0.3299404806269776169, 0.3333333333333333703, 0.3299404806269776169, 0.3333333333333333703, 0.3299404806269776169, 0.3333333333333333703, 0.3299404806269776169, 0.3333333333333333703, 0.3299404806269776169, 0.3333333333333333703, 0.3299404806269776169, 0.3333333333333333703, 0.3299404806269776169, 0.3333333333333333703, 0.3299404806269776169, 0.3333333333333333703, 0.3299404806269776169, 0.3333333333333333703, 0.3299404806269776169, 0.3333333333333333703, 0.3299404806269776169, 0.3333333333333333703, 0.3299404806269776169, 0.3333333333333333703, 0.3299404806269776169, 0.3333333333333333703, 0.3299404806269776169, 0.3333333333333333703, 0.3299404806269776169, 0.3333333333333333703, 0.3299404806269776169, 0.3333333333333333703, 0.3299404806269776169, 0.3333333333333333703, 0.3299404806269776169, 0.3333333333333333703, 0.3299404806269776169, 0.3333333333333333703, 0.3299404806269776169, 0.3333333333333333703, 0.3299404806269776169, 0.3333333333333333703, 0.3299404806269776169, 0.3333333333333333703, 0.3299404806269776169, 0.3333333333333333703, 0.3299404806269776169, 0.3333333333333333703, 0.3299404806269776169, 0.3333333333333333703, 0.3299404806269776169, 0.3333333333333333703, 0.3299404806269776169, 0.3333333333333333703, 0.3299404806269776169, 0.3333333333333333703, 0.3299404806269776169, 0.3333333333333333703, 0.3299404806269776169, 0.3333333333333333703, 0.3299404806269776169, 0.3333333333333333703, 0.3299404806269776169, 0.3333333333333333703, 0.3299404806269776169, 0.3333333333333333703, 0.3299404806269776169, 0.3333333333333333703, 0.3299404806269776169, 0.3333333333333333703, 0.3299404806269776169, 0.3333333333333333703, 0.3299404806269776169, 0.3333333333333333703, 0.3299404806269776169, 0.3333333333333333703, 0.3299404806269776169, 0.3333333333333333703, 0.3299404806269776169, 0.3333333333333333703, 0.3299404806269776169, 0.3333333333333333703, 0.3299404806269776169, 0.3333333333333333703, 0.3299404806269776169, 0.3333333333333333703, 0.3299404806269776169, 0.3333333333333333703, 0.3299404806269776169, 0.3333333333333333703, 0.3299404806269776169, 0.3333333333333333703, 0.3299404806269776169, 0.3333333333333333703, 0.3299404806269776169, 0.3333333333333333703, 0.3299404806269776169, 0.3333333333333333703, 0.3299404806269776169, 0.3333333333333333703, 0.3299404806269776169, 0.3333333333333333703, 0.3299404806269776169, 0.3333333333333333703, 0.3299404806269776169, 0.3333333333333333703, 0.3299404806269776169, 0.3333333333333333703, 0.3299404806269776169, 0.3333333333333333703, 0.3299404806269776169, 0.3333333333333333703, 0.3299404806269776169, 0.3333333333333333703, 0.3299404806269776169, 0.3333333333333333703, 0.3299404806269776169, 0.3333333333333333703, 0.3299404806269776169, 0.3333333333333333703, 0.3299404806269776169, 0.3333333333333333703, 0.3299404806269776169, 0.3333333333333333703, 0.3299404806269776169, 0.3333333333333333703, 0.3299404806269776169, 0.3333333333333333703, 0.3299404806269776169, 0.3333333333333333703, 0.3299404806269776169, 0.3333333333333333703, 0.3299404806269776169, 0.3333333333333333703, 0.3299404806269776169, 0.3333333333333333703, 0.3299404806269776169, 0.3333333333333333703, 0.3299404806269776169, 0.3333333333333333703, 0.3299404806269776169, 0.3333333333333333703, 0.3299404806269776169, 0.3333333333333333703, 0.3299404806269776169, 0.3333333333333333703, 0.3299404806269776169, 0.3333333333333333703, 0.3299404806269776169, 0.3333333333333333703, 0.3299404806269776169, 0.3333333333333333703, 0.3320603117974822438, 0.3317425830320511193),
 ( 0.3333333333333333703, 0.3299404806269776169, 0.3333333333333333703, 0.3299404806269776169, 0.3333333333333333703, 0.3299404806269776169, 0.3333333333333333703, 0.3299404806269776169, 0.3333333333333333703, 0.3299404806269776169, 0.3333333333333333703, 0.3299404806269776169, 0.3333333333333333703, 0.3299404806269776169, 0.3333333333333333703, 0.3299404806269776169, 0.3333333333333333703, 0.3299404806269776169, 0.3333333333333333703, 0.3299404806269776169, 0.3333333333333333703, 0.3299404806269776169, 0.3333333333333333703, 0.3299404806269776169, 0.3333333333333333703, 0.3299404806269776169, 0.3333333333333333703, 0.3299404806269776169, 0.3333333333333333703, 0.3299404806269776169, 0.3333333333333333703, 0.3299404806269776169, 0.3333333333333333703, 0.3299404806269776169, 0.3333333333333333703, 0.3299404806269776169, 0.3333333333333333703, 0.3299404806269776169, 0.3333333333333333703, 0.3299404806269776169, 0.3333333333333333703, 0.3299404806269776169, 0.3333333333333333703, 0.3299404806269776169, 0.3333333333333333703, 0.3299404806269776169, 0.3333333333333333703, 0.3299404806269776169, 0.3333333333333333703, 0.3299404806269776169, 0.3333333333333333703, 0.3299404806269776169, 0.3333333333333333703, 0.3299404806269776169, 0.3333333333333333703, 0.3299404806269776169, 0.3333333333333333703, 0.3299404806269776169, 0.3333333333333333703, 0.3299404806269776169, 0.3333333333333333703, 0.3299404806269776169, 0.3333333333333333703, 0.3299404806269776169, 0.3333333333333333703, 0.3299404806269776169, 0.3333333333333333703, 0.3299404806269776169, 0.3333333333333333703, 0.3299404806269776169, 0.3333333333333333703, 0.3299404806269776169, 0.3333333333333333703, 0.3299404806269776169, 0.3333333333333333703, 0.3299404806269776169, 0.3333333333333333703, 0.3299404806269776169, 0.3333333333333333703, 0.3299404806269776169, 0.3333333333333333703, 0.3299404806269776169, 0.3333333333333333703, 0.3299404806269776169, 0.3333333333333333703, 0.3299404806269776169, 0.3333333333333333703, 0.3299404806269776169, 0.3333333333333333703, 0.3299404806269776169, 0.3333333333333333703, 0.3299404806269776169, 0.3333333333333333703, 0.3299404806269776169, 0.3333333333333333703, 0.3299404806269776169, 0.3333333333333333703, 0.3299404806269776169, 0.3333333333333333703, 0.3299404806269776169, 0.3333333333333333703, 0.3299404806269776169, 0.3333333333333333703, 0.3299404806269776169, 0.3333333333333333703, 0.3299404806269776169, 0.3333333333333333703, 0.3299404806269776169, 0.3333333333333333703, 0.3299404806269776169, 0.3333333333333333703, 0.3299404806269776169, 0.3333333333333333703, 0.3299404806269776169, 0.3333333333333333703, 0.3299404806269776169, 0.3333333333333333703, 0.3299404806269776169, 0.3333333333333333703, 0.3299404806269776169, 0.3333333333333333703, 0.3299404806269776169, 0.3333333333333333703, 0.3299404806269776169, 0.3333333333333333703, 0.3299404806269776169, 0.3333333333333333703, 0.3299404806269776169, 0.3333333333333333703, 0.3299404806269776169, 0.3333333333333333703, 0.3299404806269776169, 0.3333333333333333703, 0.3299404806269776169, 0.3333333333333333703, 0.3299404806269776169, 0.3333333333333333703, 0.3299404806269776169, 0.3333333333333333703, 0.3299404806269776169, 0.3333333333333333703, 0.3299404806269776169, 0.3333333333333333703, 0.3299404806269776169, 0.3333333333333333703, 0.3299404806269776169, 0.3333333333333333703, 0.3299404806269776169, 0.3333333333333333703, 0.3299404806269776169, 0.3333333333333333703, 0.3299404806269776169, 0.3333333333333333703, 0.3299404806269776169, 0.3333333333333333703, 0.3299404806269776169, 0.3333333333333333703, 0.3299404806269776169, 0.3333333333333333703, 0.3299404806269776169, 0.3333333333333333703, 0.3299404806269776169, 0.3333333333333333703, 0.3299404806269776169, 0.3333333333333333703, 0.3299404806269776169, 0.3333333333333333703, 0.3299404806269776169, 0.3333333333333333703, 0.3299404806269776169, 0.3333333333333333703, 0.3299404806269776169, 0.3333333333333333703, 0.3299404806269776169, 0.3333333333333333703, 0.3299404806269776169, 0.3333333333333333703, 0.3299404806269776169, 0.3333333333333333703, 0.3299404806269776169, 0.3333333333333333703, 0.3299404806269776169, 0.3333333333333333703, 0.3299404806269776169, 0.3333333333333333703, 0.3299404806269776169, 0.3333333333333333703, 0.3299404806269776169, 0.3333333333333333703, 0.3299404806269776169, 0.3333333333333333703, 0.3299404806269776169, 0.3333333333333333703, 0.3299404806269776169, 0.3333333333333333703, 0.3299404806269776169, 0.3333333333333333703, 0.3299404806269776169, 0.3333333333333333703, 0.3299404806269776169, 0.3333333333333333703, 0.3299404806269776169, 0.3333333333333333703, 0.3299404806269776169, 0.3333333333333333703, 0.3299404806269776169, 0.3333333333333333703, 0.3299404806269776169, 0.3333333333333333703, 0.3299404806269776169, 0.3333333333333333703, 0.3299404806269776169, 0.3333333333333333703, 0.3299404806269776169, 0.3333333333333333703, 0.3299404806269776169, 0.3333333333333333703, 0.3299404806269776169, 0.3333333333333333703, 0.3299404806269776169, 0.3333333333333333703, 0.3299404806269776169, 0.3333333333333333703, 0.3299404806269776169, 0.3333333333333333703, 0.3299404806269776169, 0.3333333333333333703, 0.3299404806269776169, 0.3333333333333333703, 0.3299404806269776169, 0.3333333333333333703, 0.3299404806269776169, 0.3333333333333333703, 0.3299404806269776169, 0.3333333333333333703, 0.3299404806269776169, 0.3333333333333333703, 0.3299404806269776169, 0.3333333333333333703, 0.3299404806269776169, 0.3333333333333333703, 0.3299404806269776169, 0.3333333333333333703, 0.3299404806269776169, 0.3333333333333333703, 0.3299404806269776169, 0.3333333333333333703, 0.3299404806269776169, 0.3333333333333333703, 0.3299404806269776169, 0.3333333333333333703, 0.3299404806269776169, 0.3333333333333333703, 0.3299404806269776169, 0.3333333333333333703, 0.3299404806269776169, 0.3333333333333333703, 0.3299404806269776169, 0.3333333333333333703, 0.3299404806269776169, 0.3333333333333333703, 0.3299404806269776169, 0.3333333333333333703, 0.3299404806269776169, 0.3333333333333333703, 0.3299404806269776169, 0.3333333333333333703, 0.3299404806269776169, 0.3333333333333333703, 0.3299404806269776169, 0.3333333333333333703, 0.3299404806269776169, 0.3333333333333333703, 0.3299404806269776169, 0.3333333333333333703, 0.3299404806269776169, 0.3333333333333333703, 0.3299404806269776169, 0.3333333333333333703, 0.3299404806269776169, 0.3333333333333333703, 0.3299404806269776169, 0.3333333333333333703, 0.3299404806269776169, 0.3333333333333333703, 0.3299404806269776169, 0.3333333333333333703, 0.3299404806269776169, 0.3333333333333333703, 0.3299404806269776169, 0.3333333333333333703, 0.3299404806269776169, 0.3333333333333333703, 0.3299404806269776169, 0.3333333333333333703, 0.3299404806269776169, 0.3333333333333333703, 0.3299404806269776169, 0.3333333333333333703, 0.3299404806269776169, 0.3333333333333333703, 0.3299404806269776169, 0.3333333333333333703, 0.3299404806269776169, 0.3333333333333333703, 0.3299404806269776169, 0.3333333333333333703, 0.3299404806269776169, 0.3333333333333333703, 0.3299404806269776169, 0.3333333333333333703, 0.3299404806269776169, 0.3333333333333333703, 0.3299404806269776169, 0.3333333333333333703, 0.3299404806269776169, 0.3333333333333333703, 0.3299404806269776169, 0.3333333333333333703, 0.3299404806269776169, 0.3333333333333333703, 0.3299404806269776169, 0.3333333333333333703, 0.3299404806269776169, 0.3333333333333333703, 0.3299404806269776169, 0.3333333333333333703, 0.3299404806269776169, 0.3333333333333333703, 0.3299404806269776169, 0.3333333333333333703, 0.3299404806269776169, 0.3333333333333333703, 0.3299404806269776169, 0.3333333333333333703, 0.3299404806269776169, 0.3333333333333333703, 0.3299404806269776169, 0.3333333333333333703, 0.3299404806269776169, 0.3333333333333333703, 0.3299404806269776169, 0.3333333333333333703, 0.3299404806269776169, 0.3333333333333333703, 0.3299404806269776169, 0.3333333333333333703, 0.3299404806269776169, 0.3333333333333333703, 0.3299404806269776169, 0.3333333333333333703, 0.3299404806269776169, 0.3333333333333333703, 0.3299404806269776169, 0.3333333333333333703, 0.3299404806269776169, 0.3333333333333333703, 0.3299404806269776169, 0.3333333333333333703, 0.3299404806269776169, 0.3333333333333333703, 0.3299404806269776169, 0.3333333333333333703, 0.3299404806269776169, 0.3333333333333333703, 0.3299404806269776169, 0.3333333333333333703, 0.3299404806269776169, 0.3333333333333333703, 0.3299404806269776169, 0.3333333333333333703, 0.3299404806269776169, 0.3333333333333333703, 0.3299404806269776169, 0.3333333333333333703, 0.3299404806269776169, 0.3333333333333333703, 0.3299404806269776169, 0.3333333333333333703, 0.3299404806269776169, 0.3333333333333333703, 0.3299404806269776169, 0.3333333333333333703, 0.3299404806269776169, 0.3333333333333333703, 0.3299404806269776169, 0.3333333333333333703, 0.3299404806269776169, 0.3333333333333333703, 0.3299404806269776169, 0.3333333333333333703, 0.3299404806269776169, 0.3333333333333333703, 0.3299404806269776169, 0.3333333333333333703, 0.3299404806269776169, 0.3333333333333333703, 0.3299404806269776169, 0.3333333333333333703, 0.3299404806269776169, 0.3333333333333333703, 0.3299404806269776169, 0.3333333333333333703, 0.3299404806269776169, 0.3333333333333333703, 0.3299404806269776169, 0.3333333333333333703, 0.3299404806269776169, 0.3333333333333333703, 0.3299404806269776169, 0.3333333333333333703, 0.3299404806269776169, 0.3333333333333333703, 0.3299404806269776169, 0.3333333333333333703, 0.3299404806269776169, 0.3333333333333333703, 0.3299404806269776169, 0.3333333333333333703, 0.3299404806269776169, 0.3333333333333333703, 0.3299404806269776169, 0.3333333333333333703, 0.3299404806269776169, 0.3333333333333333703, 0.3299404806269776169, 0.3333333333333333703, 0.3299404806269776169, 0.3333333333333333703, 0.3299404806269776169, 0.3333333333333333703, 0.3299404806269776169, 0.3333333333333333703, 0.3299404806269776169, 0.3333333333333333703, 0.3299404806269776169, 0.3333333333333333703, 0.3299404806269776169, 0.3333333333333333703, 0.3299404806269776169, 0.3333333333333333703, 0.3299404806269776169, 0.3333333333333333703, 0.3299404806269776169, 0.3333333333333333703, 0.3299404806269776169, 0.3333333333333333703, 0.3299404806269776169, 0.3333333333333333703, 0.3299404806269776169, 0.3333333333333333703, 0.3299404806269776169, 0.3333333333333333703, 0.3299404806269776169, 0.3333333333333333703, 0.3299404806269776169, 0.3333333333333333703, 0.3299404806269776169, 0.3333333333333333703, 0.3299404806269776169, 0.3333333333333333703, 0.3299404806269776169, 0.3333333333333333703, 0.3299404806269776169, 0.3333333333333333703, 0.3299404806269776169, 0.3333333333333333703, 0.3299404806269776169, 0.3333333333333333703, 0.3299404806269776169, 0.3333333333333333703, 0.3299404806269776169, 0.3333333333333333703, 0.3299404806269776169, 0.3333333333333333703, 0.3299404806269776169, 0.3333333333333333703, 0.3299404806269776169, 0.3333333333333333703, 0.3299404806269776169, 0.3333333333333333703, 0.3299404806269776169, 0.3333333333333333703, 0.3299404806269776169, 0.3333333333333333703, 0.3299404806269776169, 0.3333333333333333703, 0.3299404806269776169, 0.3333333333333333703, 0.3299404806269776169, 0.3333333333333333703, 0.3299404806269776169, 0.3333333333333333703, 0.3299404806269776169, 0.3333333333333333703, 0.3299404806269776169, 0.3333333333333333703, 0.3299404806269776169, 0.3333333333333333703, 0.3299404806269776169, 0.3333333333333333703, 0.3299404806269776169, 0.3333333333333333703, 0.3299404806269776169, 0.3333333333333333703, 0.3299404806269776169, 0.3333333333333333703, 0.3299404806269776169, 0.3333333333333333703, 0.3299404806269776169, 0.3333333333333333703, 0.3299404806269776169, 0.3333333333333333703, 0.3299404806269776169, 0.3333333333333333703, 0.3299404806269776169, 0.3333333333333333703, 0.3299404806269776169, 0.3333333333333333703, 0.3299404806269776169, 0.3333333333333333703, 0.3299404806269776169, 0.3333333333333333703, 0.3299404806269776169, 0.3333333333333333703, 0.3299404806269776169, 0.3333333333333333703, 0.3299404806269776169, 0.3333333333333333703, 0.3299404806269776169, 0.3333333333333333703, 0.3299404806269776169, 0.3333333333333333703, 0.3299404806269776169, 0.3333333333333333703, 0.3299404806269776169, 0.3333333333333333703, 0.3299404806269776169, 0.3333333333333333703, 0.3299404806269776169, 0.3333333333333333703, 0.3299404806269776169, 0.3333333333333333703, 0.3299404806269776169, 0.3333333333333333703, 0.3299404806269776169, 0.3333333333333333703, 0.3299404806269776169, 0.3333333333333333703, 0.3299404806269776169, 0.3333333333333333703, 0.3299404806269776169, 0.3333333333333333703, 0.3299404806269776169, 0.3333333333333333703, 0.3299404806269776169, 0.3333333333333333703, 0.3299404806269776169, 0.3333333333333333703, 0.3299404806269776169, 0.3333333333333333703, 0.3299404806269776169, 0.3333333333333333703, 0.3299404806269776169, 0.3333333333333333703, 0.3299404806269776169, 0.3333333333333333703, 0.3299404806269776169, 0.3333333333333333703, 0.3299404806269776169, 0.3333333333333333703, 0.3299404806269776169, 0.3333333333333333703, 0.3299404806269776169, 0.3333333333333333703, 0.3299404806269776169, 0.3333333333333333703, 0.3299404806269776169, 0.3333333333333333703, 0.3299404806269776169, 0.3333333333333333703, 0.3299404806269776169, 0.3333333333333333703, 0.3299404806269776169, 0.3333333333333333703, 0.3299404806269776169, 0.3333333333333333703, 0.3299404806269776169, 0.3333333333333333703, 0.3299404806269776169, 0.3333333333333333703, 0.3299404806269776169, 0.3333333333333333703, 0.3299404806269776169, 0.3333333333333333703, 0.3299404806269776169, 0.3333333333333333703, 0.3299404806269776169, 0.3333333333333333703, 0.3299404806269776169, 0.3333333333333333703, 0.3299404806269776169, 0.3333333333333333703, 0.3299404806269776169, 0.3333333333333333703, 0.3299404806269776169, 0.3333333333333333703, 0.3299404806269776169, 0.3333333333333333703, 0.3299404806269776169, 0.3333333333333333703, 0.3299404806269776169, 0.3333333333333333703, 0.3299404806269776169, 0.3333333333333333703, 0.3299404806269776169, 0.3333333333333333703, 0.3299404806269776169, 0.3333333333333333703, 0.3299404806269776169, 0.3333333333333333703, 0.3299404806269776169, 0.3333333333333333703, 0.3299404806269776169, 0.3333333333333333703, 0.3299404806269776169, 0.3333333333333333703, 0.3299404806269776169, 0.3333333333333333703, 0.3299404806269776169, 0.3333333333333333703, 0.3299404806269776169, 0.3333333333333333703, 0.3299404806269776169, 0.3333333333333333703, 0.3299404806269776169, 0.3333333333333333703, 0.3299404806269776169, 0.3333333333333333703, 0.3299404806269776169, 0.3333333333333333703, 0.3299404806269776169, 0.3333333333333333703, 0.3299404806269776169, 0.3333333333333333703, 0.3299404806269776169, 0.3333333333333333703, 0.3299404806269776169, 0.3333333333333333703, 0.3299404806269776169, 0.3333333333333333703, 0.3299404806269776169, 0.3333333333333333703, 0.3299404806269776169, 0.3333333333333333703, 0.3299404806269776169, 0.3333333333333333703, 0.3299404806269776169, 0.3333333333333333703, 0.3299404806269776169, 0.3333333333333333703, 0.3299404806269776169, 0.3333333333333333703, 0.3299404806269776169, 0.3333333333333333703, 0.3299404806269776169, 0.3333333333333333703, 0.3299404806269776169, 0.3333333333333333703, 0.3299404806269776169, 0.3333333333333333703, 0.3299404806269776169, 0.3333333333333333703, 0.3299404806269776169, 0.3333333333333333703, 0.3299404806269776169, 0.3333333333333333703, 0.3299404806269776169, 0.3333333333333333703, 0.3299404806269776169, 0.3333333333333333703, 0.3299404806269776169, 0.3333333333333333703, 0.3299404806269776169, 0.3333333333333333703, 0.3299404806269776169, 0.3333333333333333703, 0.3299404806269776169, 0.3333333333333333703, 0.3299404806269776169, 0.3333333333333333703, 0.3299404806269776169, 0.3333333333333333703, 0.3299404806269776169, 0.3333333333333333703, 0.3299404806269776169, 0.3333333333333333703, 0.3299404806269776169, 0.3333333333333333703, 0.3299404806269776169, 0.3333333333333333703, 0.3299404806269776169, 0.3333333333333333703, 0.3299404806269776169, 0.3333333333333333703, 0.3299404806269776169, 0.3333333333333333703, 0.3299404806269776169, 0.3333333333333333703, 0.3299404806269776169, 0.3333333333333333703, 0.3299404806269776169, 0.3333333333333333703, 0.3299404806269776169, 0.3333333333333333703, 0.3299404806269776169, 0.3333333333333333703, 0.3299404806269776169, 0.3333333333333333703, 0.3299404806269776169, 0.3333333333333333703, 0.3299404806269776169, 0.3333333333333333703, 0.3299404806269776169, 0.3333333333333333703, 0.3299404806269776169, 0.3333333333333333703, 0.3299404806269776169, 0.3333333333333333703, 0.3299404806269776169, 0.3333333333333333703, 0.3299404806269776169, 0.3333333333333333703, 0.3299404806269776169, 0.3333333333333333703, 0.3299404806269776169, 0.3333333333333333703, 0.3299404806269776169, 0.3333333333333333703, 0.3299404806269776169, 0.3333333333333333703, 0.3299404806269776169, 0.3333333333333333703, 0.3299404806269776169, 0.3333333333333333703, 0.3299404806269776169, 0.3333333333333333703, 0.3299404806269776169, 0.3333333333333333703, 0.3299404806269776169, 0.3333333333333333703, 0.3299404806269776169, 0.3333333333333333703, 0.3299404806269776169, 0.3333333333333333703, 0.3299404806269776169, 0.3333333333333333703, 0.3299404806269776169, 0.3333333333333333703, 0.3299404806269776169, 0.3333333333333333703, 0.3299404806269776169, 0.3333333333333333703, 0.3299404806269776169, 0.3333333333333333703, 0.3299404806269776169, 0.3333333333333333703, 0.3299404806269776169, 0.3333333333333333703, 0.3299404806269776169, 0.3333333333333333703, 0.3299404806269776169, 0.3333333333333333703, 0.3299404806269776169, 0.3333333333333333703, 0.3299404806269776169, 0.3333333333333333703, 0.3299404806269776169, 0.3333333333333333703, 0.3299404806269776169, 0.3333333333333333703, 0.3299404806269776169, 0.3333333333333333703, 0.3299404806269776169, 0.3333333333333333703, 0.3299404806269776169, 0.3333333333333333703, 0.3299404806269776169, 0.3333333333333333703, 0.3299404806269776169, 0.3333333333333333703, 0.3299404806269776169, 0.3333333333333333703, 0.3299404806269776169, 0.3333333333333333703, 0.3299404806269776169, 0.3333333333333333703, 0.3299404806269776169, 0.3333333333333333703, 0.3299404806269776169, 0.3333333333333333703, 0.3299404806269776169, 0.3333333333333333703, 0.3299404806269776169, 0.3333333333333333703, 0.3299404806269776169, 0.3333333333333333703, 0.3299404806269776169, 0.3333333333333333703, 0.3299404806269776169, 0.3333333333333333703, 0.3299404806269776169, 0.3333333333333333703, 0.3299404806269776169, 0.3333333333333333703, 0.3299404806269776169, 0.3333333333333333703, 0.3299404806269776169, 0.3333333333333333703, 0.3299404806269776169, 0.3333333333333333703, 0.3299404806269776169, 0.3333333333333333703, 0.3299404806269776169, 0.3333333333333333703, 0.3299404806269776169, 0.3333333333333333703, 0.3299404806269776169, 0.3333333333333333703, 0.3299404806269776169, 0.3333333333333333703, 0.3299404806269776169, 0.3333333333333333703, 0.3299404806269776169, 0.3333333333333333703, 0.3299404806269776169, 0.3333333333333333703, 0.3299404806269776169, 0.3333333333333333703, 0.3299404806269776169, 0.3333333333333333703, 0.3299404806269776169, 0.3333333333333333703, 0.3299404806269776169, 0.3333333333333333703, 0.3299404806269776169, 0.3333333333333333703, 0.3299404806269776169, 0.3333333333333333703, 0.3299404806269776169, 0.3333333333333333703, 0.3299404806269776169, 0.3333333333333333703, 0.3299404806269776169, 0.3333333333333333703, 0.3299404806269776169, 0.3333333333333333703, 0.3299404806269776169, 0.3333333333333333703, 0.3299404806269776169, 0.3333333333333333703, 0.3320603117974822438, 0.3317425830320511193),
 ( 1.000000000000000000, 0.9898214418809326842, 1.000000000000000000, 0.9898214418809326842, 1.000000000000000000, 0.9898214418809326842, 1.000000000000000000, 0.9898214418809326842, 1.000000000000000000, 0.9898214418809326842, 1.000000000000000000, 0.9898214418809326842, 1.000000000000000000, 0.9898214418809326842, 1.000000000000000000, 0.9898214418809326842, 1.000000000000000000, 0.9898214418809326842, 1.000000000000000000, 0.9898214418809326842, 1.000000000000000000, 0.9898214418809326842, 1.000000000000000000, 0.9898214418809326842, 1.000000000000000000, 0.9898214418809326842, 1.000000000000000000, 0.9898214418809326842, 1.000000000000000000, 0.9898214418809326842, 1.000000000000000000, 0.9898214418809326842, 1.000000000000000000, 0.9898214418809326842, 1.000000000000000000, 0.9898214418809326842, 1.000000000000000000, 0.9898214418809326842, 1.000000000000000000, 0.9898214418809326842, 1.000000000000000000, 0.9898214418809326842, 1.000000000000000000, 0.9898214418809326842, 1.000000000000000000, 0.9898214418809326842, 1.000000000000000000, 0.9898214418809326842, 1.000000000000000000, 0.9898214418809326842, 1.000000000000000000, 0.9898214418809326842, 1.000000000000000000, 0.9898214418809326842, 1.000000000000000000, 0.9898214418809326842, 1.000000000000000000, 0.9898214418809326842, 1.000000000000000000, 0.9898214418809326842, 1.000000000000000000, 0.9898214418809326842, 1.000000000000000000, 0.9898214418809326842, 1.000000000000000000, 0.9898214418809326842, 1.000000000000000000, 0.9898214418809326842, 1.000000000000000000, 0.9898214418809326842, 1.000000000000000000, 0.9898214418809326842, 1.000000000000000000, 0.9898214418809326842, 1.000000000000000000, 0.9898214418809326842, 1.000000000000000000, 0.9898214418809326842, 1.000000000000000000, 0.9898214418809326842, 1.000000000000000000, 0.9898214418809326842, 1.000000000000000000, 0.9898214418809326842, 1.000000000000000000, 0.9898214418809326842, 1.000000000000000000, 0.9898214418809326842, 1.000000000000000000, 0.9898214418809326842, 1.000000000000000000, 0.9898214418809326842, 1.000000000000000000, 0.9898214418809326842, 1.000000000000000000, 0.9898214418809326842, 1.000000000000000000, 0.9898214418809326842, 1.000000000000000000, 0.9898214418809326842, 1.000000000000000000, 0.9898214418809326842, 1.000000000000000000, 0.9898214418809326842, 1.000000000000000000, 0.9898214418809326842, 1.000000000000000000, 0.9898214418809326842, 1.000000000000000000, 0.9898214418809326842, 1.000000000000000000, 0.9898214418809326842, 1.000000000000000000, 0.9898214418809326842, 1.000000000000000000, 0.9898214418809326842, 1.000000000000000000, 0.9898214418809326842, 1.000000000000000000, 0.9898214418809326842, 1.000000000000000000, 0.9898214418809326842, 1.000000000000000000, 0.9898214418809326842, 1.000000000000000000, 0.9898214418809326842, 1.000000000000000000, 0.9898214418809326842, 1.000000000000000000, 0.9898214418809326842, 1.000000000000000000, 0.9898214418809326842, 1.000000000000000000, 0.9898214418809326842, 1.000000000000000000, 0.9898214418809326842, 1.000000000000000000, 0.9898214418809326842, 1.000000000000000000, 0.9898214418809326842, 1.000000000000000000, 0.9898214418809326842, 1.000000000000000000, 0.9898214418809326842, 1.000000000000000000, 0.9898214418809326842, 1.000000000000000000, 0.9898214418809326842, 1.000000000000000000, 0.9898214418809326842, 1.000000000000000000, 0.9898214418809326842, 1.000000000000000000, 0.9898214418809326842, 1.000000000000000000, 0.9898214418809326842, 1.000000000000000000, 0.9898214418809326842, 1.000000000000000000, 0.9898214418809326842, 1.000000000000000000, 0.9898214418809326842, 1.000000000000000000, 0.9898214418809326842, 1.000000000000000000, 0.9898214418809326842, 1.000000000000000000, 0.9898214418809326842, 1.000000000000000000, 0.9898214418809326842, 1.000000000000000000, 0.9898214418809326842, 1.000000000000000000, 0.9898214418809326842, 1.000000000000000000, 0.9898214418809326842, 1.000000000000000000, 0.9898214418809326842, 1.000000000000000000, 0.9898214418809326842, 1.000000000000000000, 0.9898214418809326842, 1.000000000000000000, 0.9898214418809326842, 1.000000000000000000, 0.9898214418809326842, 1.000000000000000000, 0.9898214418809326842, 1.000000000000000000, 0.9898214418809326842, 1.000000000000000000, 0.9898214418809326842, 1.000000000000000000, 0.9898214418809326842, 1.000000000000000000, 0.9898214418809326842, 1.000000000000000000, 0.9898214418809326842, 1.000000000000000000, 0.9898214418809326842, 1.000000000000000000, 0.9898214418809326842, 1.000000000000000000, 0.9898214418809326842, 1.000000000000000000, 0.9898214418809326842, 1.000000000000000000, 0.9898214418809326842, 1.000000000000000000, 0.9898214418809326842, 1.000000000000000000, 0.9898214418809326842, 1.000000000000000000, 0.9898214418809326842, 1.000000000000000000, 0.9898214418809326842, 1.000000000000000000, 0.9898214418809326842, 1.000000000000000000, 0.9898214418809326842, 1.000000000000000000, 0.9898214418809326842, 1.000000000000000000, 0.9898214418809326842, 1.000000000000000000, 0.9898214418809326842, 1.000000000000000000, 0.9898214418809326842, 1.000000000000000000, 0.9898214418809326842, 1.000000000000000000, 0.9898214418809326842, 1.000000000000000000, 0.9898214418809326842, 1.000000000000000000, 0.9898214418809326842, 1.000000000000000000, 0.9898214418809326842, 1.000000000000000000, 0.9898214418809326842, 1.000000000000000000, 0.9898214418809326842, 1.000000000000000000, 0.9898214418809326842, 1.000000000000000000, 0.9898214418809326842, 1.000000000000000000, 0.9898214418809326842, 1.000000000000000000, 0.9898214418809326842, 1.000000000000000000, 0.9898214418809326842, 1.000000000000000000, 0.9898214418809326842, 1.000000000000000000, 0.9898214418809326842, 1.000000000000000000, 0.9898214418809326842, 1.000000000000000000, 0.9898214418809326842, 1.000000000000000000, 0.9898214418809326842, 1.000000000000000000, 0.9898214418809326842, 1.000000000000000000, 0.9898214418809326842, 1.000000000000000000, 0.9898214418809326842, 1.000000000000000000, 0.9898214418809326842, 1.000000000000000000, 0.9898214418809326842, 1.000000000000000000, 0.9898214418809326842, 1.000000000000000000, 0.9898214418809326842, 1.000000000000000000, 0.9898214418809326842, 1.000000000000000000, 0.9898214418809326842, 1.000000000000000000, 0.9898214418809326842, 1.000000000000000000, 0.9898214418809326842, 1.000000000000000000, 0.9898214418809326842, 1.000000000000000000, 0.9898214418809326842, 1.000000000000000000, 0.9898214418809326842, 1.000000000000000000, 0.9898214418809326842, 1.000000000000000000, 0.9898214418809326842, 1.000000000000000000, 0.9898214418809326842, 1.000000000000000000, 0.9898214418809326842, 1.000000000000000000, 0.9898214418809326842, 1.000000000000000000, 0.9898214418809326842, 1.000000000000000000, 0.9898214418809326842, 1.000000000000000000, 0.9898214418809326842, 1.000000000000000000, 0.9898214418809326842, 1.000000000000000000, 0.9898214418809326842, 1.000000000000000000, 0.9898214418809326842, 1.000000000000000000, 0.9898214418809326842, 1.000000000000000000, 0.9898214418809326842, 1.000000000000000000, 0.9898214418809326842, 1.000000000000000000, 0.9898214418809326842, 1.000000000000000000, 0.9898214418809326842, 1.000000000000000000, 0.9898214418809326842, 1.000000000000000000, 0.9898214418809326842, 1.000000000000000000, 0.9898214418809326842, 1.000000000000000000, 0.9898214418809326842, 1.000000000000000000, 0.9898214418809326842, 1.000000000000000000, 0.9898214418809326842, 1.000000000000000000, 0.9898214418809326842, 1.000000000000000000, 0.9898214418809326842, 1.000000000000000000, 0.9898214418809326842, 1.000000000000000000, 0.9898214418809326842, 1.000000000000000000, 0.9898214418809326842, 1.000000000000000000, 0.9898214418809326842, 1.000000000000000000, 0.9898214418809326842, 1.000000000000000000, 0.9898214418809326842, 1.000000000000000000, 0.9898214418809326842, 1.000000000000000000, 0.9898214418809326842, 1.000000000000000000, 0.9898214418809326842, 1.000000000000000000, 0.9898214418809326842, 1.000000000000000000, 0.9898214418809326842, 1.000000000000000000, 0.9898214418809326842, 1.000000000000000000, 0.9898214418809326842, 1.000000000000000000, 0.9898214418809326842, 1.000000000000000000, 0.9898214418809326842, 1.000000000000000000, 0.9898214418809326842, 1.000000000000000000, 0.9898214418809326842, 1.000000000000000000, 0.9898214418809326842, 1.000000000000000000, 0.9898214418809326842, 1.000000000000000000, 0.9898214418809326842, 1.000000000000000000, 0.9898214418809326842, 1.000000000000000000, 0.9898214418809326842, 1.000000000000000000, 0.9898214418809326842, 1.000000000000000000, 0.9898214418809326842, 1.000000000000000000, 0.9898214418809326842, 1.000000000000000000, 0.9898214418809326842, 1.000000000000000000, 0.9898214418809326842, 1.000000000000000000, 0.9898214418809326842, 1.000000000000000000, 0.9898214418809326842, 1.000000000000000000, 0.9898214418809326842, 1.000000000000000000, 0.9898214418809326842, 1.000000000000000000, 0.9898214418809326842, 1.000000000000000000, 0.9898214418809326842, 1.000000000000000000, 0.9898214418809326842, 1.000000000000000000, 0.9898214418809326842, 1.000000000000000000, 0.9898214418809326842, 1.000000000000000000, 0.9898214418809326842, 1.000000000000000000, 0.9898214418809326842, 1.000000000000000000, 0.9898214418809326842, 1.000000000000000000, 0.9898214418809326842, 1.000000000000000000, 0.9898214418809326842, 1.000000000000000000, 0.9898214418809326842, 1.000000000000000000, 0.9898214418809326842, 1.000000000000000000, 0.9898214418809326842, 1.000000000000000000, 0.9898214418809326842, 1.000000000000000000, 0.9898214418809326842, 1.000000000000000000, 0.9898214418809326842, 1.000000000000000000, 0.9898214418809326842, 1.000000000000000000, 0.9898214418809326842, 1.000000000000000000, 0.9898214418809326842, 1.000000000000000000, 0.9898214418809326842, 1.000000000000000000, 0.9898214418809326842, 1.000000000000000000, 0.9898214418809326842, 1.000000000000000000, 0.9898214418809326842, 1.000000000000000000, 0.9898214418809326842, 1.000000000000000000, 0.9898214418809326842, 1.000000000000000000, 0.9898214418809326842, 1.000000000000000000, 0.9898214418809326842, 1.000000000000000000, 0.9898214418809326842, 1.000000000000000000, 0.9898214418809326842, 1.000000000000000000, 0.9898214418809326842, 1.000000000000000000, 0.9898214418809326842, 1.000000000000000000, 0.9898214418809326842, 1.000000000000000000, 0.9898214418809326842, 1.000000000000000000, 0.9898214418809326842, 1.000000000000000000, 0.9898214418809326842, 1.000000000000000000, 0.9898214418809326842, 1.000000000000000000, 0.9898214418809326842, 1.000000000000000000, 0.9898214418809326842, 1.000000000000000000, 0.9898214418809326842, 1.000000000000000000, 0.9898214418809326842, 1.000000000000000000, 0.9898214418809326842, 1.000000000000000000, 0.9898214418809326842, 1.000000000000000000, 0.9898214418809326842, 1.000000000000000000, 0.9898214418809326842, 1.000000000000000000, 0.9898214418809326842, 1.000000000000000000, 0.9898214418809326842, 1.000000000000000000, 0.9898214418809326842, 1.000000000000000000, 0.9898214418809326842, 1.000000000000000000, 0.9898214418809326842, 1.000000000000000000, 0.9898214418809326842, 1.000000000000000000, 0.9898214418809326842, 1.000000000000000000, 0.9898214418809326842, 1.000000000000000000, 0.9898214418809326842, 1.000000000000000000, 0.9898214418809326842, 1.000000000000000000, 0.9898214418809326842, 1.000000000000000000, 0.9898214418809326842, 1.000000000000000000, 0.9898214418809326842, 1.000000000000000000, 0.9898214418809326842, 1.000000000000000000, 0.9898214418809326842, 1.000000000000000000, 0.9898214418809326842, 1.000000000000000000, 0.9898214418809326842, 1.000000000000000000, 0.9898214418809326842, 1.000000000000000000, 0.9898214418809326842, 1.000000000000000000, 0.9898214418809326842, 1.000000000000000000, 0.9898214418809326842, 1.000000000000000000, 0.9898214418809326842, 1.000000000000000000, 0.9898214418809326842, 1.000000000000000000, 0.9898214418809326842, 1.000000000000000000, 0.9898214418809326842, 1.000000000000000000, 0.9898214418809326842, 1.000000000000000000, 0.9898214418809326842, 1.000000000000000000, 0.9898214418809326842, 1.000000000000000000, 0.9898214418809326842, 1.000000000000000000, 0.9898214418809326842, 1.000000000000000000, 0.9898214418809326842, 1.000000000000000000, 0.9898214418809326842, 1.000000000000000000, 0.9898214418809326842, 1.000000000000000000, 0.9898214418809326842, 1.000000000000000000, 0.9898214418809326842, 1.000000000000000000, 0.9898214418809326842, 1.000000000000000000, 0.9898214418809326842, 1.000000000000000000, 0.9898214418809326842, 1.000000000000000000, 0.9898214418809326842, 1.000000000000000000, 0.9898214418809326842, 1.000000000000000000, 0.9898214418809326842, 1.000000000000000000, 0.9898214418809326842, 1.000000000000000000, 0.9898214418809326842, 1.000000000000000000, 0.9898214418809326842, 1.000000000000000000, 0.9898214418809326842, 1.000000000000000000, 0.9898214418809326842, 1.000000000000000000, 0.9898214418809326842, 1.000000000000000000, 0.9898214418809326842, 1.000000000000000000, 0.9898214418809326842, 1.000000000000000000, 0.9898214418809326842, 1.000000000000000000, 0.9898214418809326842, 1.000000000000000000, 0.9898214418809326842, 1.000000000000000000, 0.9898214418809326842, 1.000000000000000000, 0.9898214418809326842, 1.000000000000000000, 0.9898214418809326842, 1.000000000000000000, 0.9898214418809326842, 1.000000000000000000, 0.9898214418809326842, 1.000000000000000000, 0.9898214418809326842, 1.000000000000000000, 0.9898214418809326842, 1.000000000000000000, 0.9898214418809326842, 1.000000000000000000, 0.9898214418809326842, 1.000000000000000000, 0.9898214418809326842, 1.000000000000000000, 0.9898214418809326842, 1.000000000000000000, 0.9898214418809326842, 1.000000000000000000, 0.9898214418809326842, 1.000000000000000000, 0.9898214418809326842, 1.000000000000000000, 0.9898214418809326842, 1.000000000000000000, 0.9898214418809326842, 1.000000000000000000, 0.9898214418809326842, 1.000000000000000000, 0.9898214418809326842, 1.000000000000000000, 0.9898214418809326842, 1.000000000000000000, 0.9898214418809326842, 1.000000000000000000, 0.9898214418809326842, 1.000000000000000000, 0.9898214418809326842, 1.000000000000000000, 0.9898214418809326842, 1.000000000000000000, 0.9898214418809326842, 1.000000000000000000, 0.9898214418809326842, 1.000000000000000000, 0.9898214418809326842, 1.000000000000000000, 0.9898214418809326842, 1.000000000000000000, 0.9898214418809326842, 1.000000000000000000, 0.9898214418809326842, 1.000000000000000000, 0.9898214418809326842, 1.000000000000000000, 0.9898214418809326842, 1.000000000000000000, 0.9898214418809326842, 1.000000000000000000, 0.9898214418809326842, 1.000000000000000000, 0.9898214418809326842, 1.000000000000000000, 0.9898214418809326842, 1.000000000000000000, 0.9898214418809326842, 1.000000000000000000, 0.9898214418809326842, 1.000000000000000000, 0.9898214418809326842, 1.000000000000000000, 0.9898214418809326842, 1.000000000000000000, 0.9898214418809326842, 1.000000000000000000, 0.9898214418809326842, 1.000000000000000000, 0.9898214418809326842, 1.000000000000000000, 0.9898214418809326842, 1.000000000000000000, 0.9898214418809326842, 1.000000000000000000, 0.9898214418809326842, 1.000000000000000000, 0.9898214418809326842, 1.000000000000000000, 0.9898214418809326842, 1.000000000000000000, 0.9898214418809326842, 1.000000000000000000, 0.9898214418809326842, 1.000000000000000000, 0.9898214418809326842, 1.000000000000000000, 0.9898214418809326842, 1.000000000000000000, 0.9898214418809326842, 1.000000000000000000, 0.9898214418809326842, 1.000000000000000000, 0.9898214418809326842, 1.000000000000000000, 0.9898214418809326842, 1.000000000000000000, 0.9898214418809326842, 1.000000000000000000, 0.9898214418809326842, 1.000000000000000000, 0.9898214418809326842, 1.000000000000000000, 0.9898214418809326842, 1.000000000000000000, 0.9898214418809326842, 1.000000000000000000, 0.9898214418809326842, 1.000000000000000000, 0.9898214418809326842, 1.000000000000000000, 0.9898214418809326842, 1.000000000000000000, 0.9898214418809326842, 1.000000000000000000, 0.9898214418809326842, 1.000000000000000000, 0.9898214418809326842, 1.000000000000000000, 0.9898214418809326842, 1.000000000000000000, 0.9898214418809326842, 1.000000000000000000, 0.9898214418809326842, 1.000000000000000000, 0.9898214418809326842, 1.000000000000000000, 0.9898214418809326842, 1.000000000000000000, 0.9898214418809326842, 1.000000000000000000, 0.9898214418809326842, 1.000000000000000000, 0.9898214418809326842, 1.000000000000000000, 0.9898214418809326842, 1.000000000000000000, 0.9898214418809326842, 1.000000000000000000, 0.9898214418809326842, 1.000000000000000000, 0.9898214418809326842, 1.000000000000000000, 0.9898214418809326842, 1.000000000000000000, 0.9898214418809326842, 1.000000000000000000, 0.9898214418809326842, 1.000000000000000000, 0.9898214418809326842, 1.000000000000000000, 0.9898214418809326842, 1.000000000000000000, 0.9898214418809326842, 1.000000000000000000, 0.9898214418809326842, 1.000000000000000000, 0.9898214418809326842, 1.000000000000000000, 0.9898214418809326842, 1.000000000000000000, 0.9898214418809326842, 1.000000000000000000, 0.9898214418809326842, 1.000000000000000000, 0.9898214418809326842, 1.000000000000000000, 0.9898214418809326842, 1.000000000000000000, 0.9898214418809326842, 1.000000000000000000, 0.9898214418809326842, 1.000000000000000000, 0.9898214418809326842, 1.000000000000000000, 0.9898214418809326842, 1.000000000000000000, 0.9898214418809326842, 1.000000000000000000, 0.9898214418809326842, 1.000000000000000000, 0.9898214418809326842, 1.000000000000000000, 0.9898214418809326842, 1.000000000000000000, 0.9898214418809326842, 1.000000000000000000, 0.9898214418809326842, 1.000000000000000000, 0.9898214418809326842, 1.000000000000000000, 0.9898214418809326842, 1.000000000000000000, 0.9898214418809326842, 1.000000000000000000, 0.9898214418809326842, 1.000000000000000000, 0.9898214418809326842, 1.000000000000000000, 0.9898214418809326842, 1.000000000000000000, 0.9898214418809326842, 1.000000000000000000, 0.9898214418809326842, 1.000000000000000000, 0.9898214418809326842, 1.000000000000000000, 0.9898214418809326842, 1.000000000000000000, 0.9898214418809326842, 1.000000000000000000, 0.9898214418809326842, 1.000000000000000000, 0.9898214418809326842, 1.000000000000000000, 0.9898214418809326842, 1.000000000000000000, 0.9898214418809326842, 1.000000000000000000, 0.9898214418809326842, 1.000000000000000000, 0.9898214418809326842, 1.000000000000000000, 0.9898214418809326842, 1.000000000000000000, 0.9898214418809326842, 1.000000000000000000, 0.9898214418809326842, 1.000000000000000000, 0.9898214418809326842, 1.000000000000000000, 0.9898214418809326842, 1.000000000000000000, 0.9898214418809326842, 1.000000000000000000, 0.9898214418809326842, 1.000000000000000000, 0.9898214418809326842, 1.000000000000000000, 0.9898214418809326842, 1.000000000000000000, 0.9898214418809326842, 1.000000000000000000, 0.9898214418809326842, 1.000000000000000000, 0.9898214418809326842, 1.000000000000000000, 0.9898214418809326842, 1.000000000000000000, 0.9898214418809326842, 1.000000000000000000, 0.9898214418809326842, 1.000000000000000000, 0.9898214418809326842, 1.000000000000000000, 0.9961809353924466759, 0.9952277490961531914),
 ( 0.3333333333333333703, 0.3299404806269776169, 0.3333333333333333703, 0.3299404806269776169, 0.3333333333333333703, 0.3299404806269776169, 0.3333333333333333703, 0.3299404806269776169, 0.3333333333333333703, 0.3299404806269776169, 0.3333333333333333703, 0.3299404806269776169, 0.3333333333333333703, 0.3299404806269776169, 0.3333333333333333703, 0.3299404806269776169, 0.3333333333333333703, 0.3299404806269776169, 0.3333333333333333703, 0.3299404806269776169, 0.3333333333333333703, 0.3299404806269776169, 0.3333333333333333703, 0.3299404806269776169, 0.3333333333333333703, 0.3299404806269776169, 0.3333333333333333703, 0.3299404806269776169, 0.3333333333333333703, 0.3299404806269776169, 0.3333333333333333703, 0.3299404806269776169, 0.3333333333333333703, 0.3299404806269776169, 0.3333333333333333703, 0.3299404806269776169, 0.3333333333333333703, 0.3299404806269776169, 0.3333333333333333703, 0.3299404806269776169, 0.3333333333333333703, 0.3299404806269776169, 0.3333333333333333703, 0.3299404806269776169, 0.3333333333333333703, 0.3299404806269776169, 0.3333333333333333703, 0.3299404806269776169, 0.3333333333333333703, 0.3299404806269776169, 0.3333333333333333703, 0.3299404806269776169, 0.3333333333333333703, 0.3299404806269776169, 0.3333333333333333703, 0.3299404806269776169, 0.3333333333333333703, 0.3299404806269776169, 0.3333333333333333703, 0.3299404806269776169, 0.3333333333333333703, 0.3299404806269776169, 0.3333333333333333703, 0.3299404806269776169, 0.3333333333333333703, 0.3299404806269776169, 0.3333333333333333703, 0.3299404806269776169, 0.3333333333333333703, 0.3299404806269776169, 0.3333333333333333703, 0.3299404806269776169, 0.3333333333333333703, 0.3299404806269776169, 0.3333333333333333703, 0.3299404806269776169, 0.3333333333333333703, 0.3299404806269776169, 0.3333333333333333703, 0.3299404806269776169, 0.3333333333333333703, 0.3299404806269776169, 0.3333333333333333703, 0.3299404806269776169, 0.3333333333333333703, 0.3299404806269776169, 0.3333333333333333703, 0.3299404806269776169, 0.3333333333333333703, 0.3299404806269776169, 0.3333333333333333703, 0.3299404806269776169, 0.3333333333333333703, 0.3299404806269776169, 0.3333333333333333703, 0.3299404806269776169, 0.3333333333333333703, 0.3299404806269776169, 0.3333333333333333703, 0.3299404806269776169, 0.3333333333333333703, 0.3299404806269776169, 0.3333333333333333703, 0.3299404806269776169, 0.3333333333333333703, 0.3299404806269776169, 0.3333333333333333703, 0.3299404806269776169, 0.3333333333333333703, 0.3299404806269776169, 0.3333333333333333703, 0.3299404806269776169, 0.3333333333333333703, 0.3299404806269776169, 0.3333333333333333703, 0.3299404806269776169, 0.3333333333333333703, 0.3299404806269776169, 0.3333333333333333703, 0.3299404806269776169, 0.3333333333333333703, 0.3299404806269776169, 0.3333333333333333703, 0.3299404806269776169, 0.3333333333333333703, 0.3299404806269776169, 0.3333333333333333703, 0.3299404806269776169, 0.3333333333333333703, 0.3299404806269776169, 0.3333333333333333703, 0.3299404806269776169, 0.3333333333333333703, 0.3299404806269776169, 0.3333333333333333703, 0.3299404806269776169, 0.3333333333333333703, 0.3299404806269776169, 0.3333333333333333703, 0.3299404806269776169, 0.3333333333333333703, 0.3299404806269776169, 0.3333333333333333703, 0.3299404806269776169, 0.3333333333333333703, 0.3299404806269776169, 0.3333333333333333703, 0.3299404806269776169, 0.3333333333333333703, 0.3299404806269776169, 0.3333333333333333703, 0.3299404806269776169, 0.3333333333333333703, 0.3299404806269776169, 0.3333333333333333703, 0.3299404806269776169, 0.3333333333333333703, 0.3299404806269776169, 0.3333333333333333703, 0.3299404806269776169, 0.3333333333333333703, 0.3299404806269776169, 0.3333333333333333703, 0.3299404806269776169, 0.3333333333333333703, 0.3299404806269776169, 0.3333333333333333703, 0.3299404806269776169, 0.3333333333333333703, 0.3299404806269776169, 0.3333333333333333703, 0.3299404806269776169, 0.3333333333333333703, 0.3299404806269776169, 0.3333333333333333703, 0.3299404806269776169, 0.3333333333333333703, 0.3299404806269776169, 0.3333333333333333703, 0.3299404806269776169, 0.3333333333333333703, 0.3299404806269776169, 0.3333333333333333703, 0.3299404806269776169, 0.3333333333333333703, 0.3299404806269776169, 0.3333333333333333703, 0.3299404806269776169, 0.3333333333333333703, 0.3299404806269776169, 0.3333333333333333703, 0.3299404806269776169, 0.3333333333333333703, 0.3299404806269776169, 0.3333333333333333703, 0.3299404806269776169, 0.3333333333333333703, 0.3299404806269776169, 0.3333333333333333703, 0.3299404806269776169, 0.3333333333333333703, 0.3299404806269776169, 0.3333333333333333703, 0.3299404806269776169, 0.3333333333333333703, 0.3299404806269776169, 0.3333333333333333703, 0.3299404806269776169, 0.3333333333333333703, 0.3299404806269776169, 0.3333333333333333703, 0.3299404806269776169, 0.3333333333333333703, 0.3299404806269776169, 0.3333333333333333703, 0.3299404806269776169, 0.3333333333333333703, 0.3299404806269776169, 0.3333333333333333703, 0.3299404806269776169, 0.3333333333333333703, 0.3299404806269776169, 0.3333333333333333703, 0.3299404806269776169, 0.3333333333333333703, 0.3299404806269776169, 0.3333333333333333703, 0.3299404806269776169, 0.3333333333333333703, 0.3299404806269776169, 0.3333333333333333703, 0.3299404806269776169, 0.3333333333333333703, 0.3299404806269776169, 0.3333333333333333703, 0.3299404806269776169, 0.3333333333333333703, 0.3299404806269776169, 0.3333333333333333703, 0.3299404806269776169, 0.3333333333333333703, 0.3299404806269776169, 0.3333333333333333703, 0.3299404806269776169, 0.3333333333333333703, 0.3299404806269776169, 0.3333333333333333703, 0.3299404806269776169, 0.3333333333333333703, 0.3299404806269776169, 0.3333333333333333703, 0.3299404806269776169, 0.3333333333333333703, 0.3299404806269776169, 0.3333333333333333703, 0.3299404806269776169, 0.3333333333333333703, 0.3299404806269776169, 0.3333333333333333703, 0.3299404806269776169, 0.3333333333333333703, 0.3299404806269776169, 0.3333333333333333703, 0.3299404806269776169, 0.3333333333333333703, 0.3299404806269776169, 0.3333333333333333703, 0.3299404806269776169, 0.3333333333333333703, 0.3299404806269776169, 0.3333333333333333703, 0.3299404806269776169, 0.3333333333333333703, 0.3299404806269776169, 0.3333333333333333703, 0.3299404806269776169, 0.3333333333333333703, 0.3299404806269776169, 0.3333333333333333703, 0.3299404806269776169, 0.3333333333333333703, 0.3299404806269776169, 0.3333333333333333703, 0.3299404806269776169, 0.3333333333333333703, 0.3299404806269776169, 0.3333333333333333703, 0.3299404806269776169, 0.3333333333333333703, 0.3299404806269776169, 0.3333333333333333703, 0.3299404806269776169, 0.3333333333333333703, 0.3299404806269776169, 0.3333333333333333703, 0.3299404806269776169, 0.3333333333333333703, 0.3299404806269776169, 0.3333333333333333703, 0.3299404806269776169, 0.3333333333333333703, 0.3299404806269776169, 0.3333333333333333703, 0.3299404806269776169, 0.3333333333333333703, 0.3299404806269776169, 0.3333333333333333703, 0.3299404806269776169, 0.3333333333333333703, 0.3299404806269776169, 0.3333333333333333703, 0.3299404806269776169, 0.3333333333333333703, 0.3299404806269776169, 0.3333333333333333703, 0.3299404806269776169, 0.3333333333333333703, 0.3299404806269776169, 0.3333333333333333703, 0.3299404806269776169, 0.3333333333333333703, 0.3299404806269776169, 0.3333333333333333703, 0.3299404806269776169, 0.3333333333333333703, 0.3299404806269776169, 0.3333333333333333703, 0.3299404806269776169, 0.3333333333333333703, 0.3299404806269776169, 0.3333333333333333703, 0.3299404806269776169, 0.3333333333333333703, 0.3299404806269776169, 0.3333333333333333703, 0.3299404806269776169, 0.3333333333333333703, 0.3299404806269776169, 0.3333333333333333703, 0.3299404806269776169, 0.3333333333333333703, 0.3299404806269776169, 0.3333333333333333703, 0.3299404806269776169, 0.3333333333333333703, 0.3299404806269776169, 0.3333333333333333703, 0.3299404806269776169, 0.3333333333333333703, 0.3299404806269776169, 0.3333333333333333703, 0.3299404806269776169, 0.3333333333333333703, 0.3299404806269776169, 0.3333333333333333703, 0.3299404806269776169, 0.3333333333333333703, 0.3299404806269776169, 0.3333333333333333703, 0.3299404806269776169, 0.3333333333333333703, 0.3299404806269776169, 0.3333333333333333703, 0.3299404806269776169, 0.3333333333333333703, 0.3299404806269776169, 0.3333333333333333703, 0.3299404806269776169, 0.3333333333333333703, 0.3299404806269776169, 0.3333333333333333703, 0.3299404806269776169, 0.3333333333333333703, 0.3299404806269776169, 0.3333333333333333703, 0.3299404806269776169, 0.3333333333333333703, 0.3299404806269776169, 0.3333333333333333703, 0.3299404806269776169, 0.3333333333333333703, 0.3299404806269776169, 0.3333333333333333703, 0.3299404806269776169, 0.3333333333333333703, 0.3299404806269776169, 0.3333333333333333703, 0.3299404806269776169, 0.3333333333333333703, 0.3299404806269776169, 0.3333333333333333703, 0.3299404806269776169, 0.3333333333333333703, 0.3299404806269776169, 0.3333333333333333703, 0.3299404806269776169, 0.3333333333333333703, 0.3299404806269776169, 0.3333333333333333703, 0.3299404806269776169, 0.3333333333333333703, 0.3299404806269776169, 0.3333333333333333703, 0.3299404806269776169, 0.3333333333333333703, 0.3299404806269776169, 0.3333333333333333703, 0.3299404806269776169, 0.3333333333333333703, 0.3299404806269776169, 0.3333333333333333703, 0.3299404806269776169, 0.3333333333333333703, 0.3299404806269776169, 0.3333333333333333703, 0.3299404806269776169, 0.3333333333333333703, 0.3299404806269776169, 0.3333333333333333703, 0.3299404806269776169, 0.3333333333333333703, 0.3299404806269776169, 0.3333333333333333703, 0.3299404806269776169, 0.3333333333333333703, 0.3299404806269776169, 0.3333333333333333703, 0.3299404806269776169, 0.3333333333333333703, 0.3299404806269776169, 0.3333333333333333703, 0.3299404806269776169, 0.3333333333333333703, 0.3299404806269776169, 0.3333333333333333703, 0.3299404806269776169, 0.3333333333333333703, 0.3299404806269776169, 0.3333333333333333703, 0.3299404806269776169, 0.3333333333333333703, 0.3299404806269776169, 0.3333333333333333703, 0.3299404806269776169, 0.3333333333333333703, 0.3299404806269776169, 0.3333333333333333703, 0.3299404806269776169, 0.3333333333333333703, 0.3299404806269776169, 0.3333333333333333703, 0.3299404806269776169, 0.3333333333333333703, 0.3299404806269776169, 0.3333333333333333703, 0.3299404806269776169, 0.3333333333333333703, 0.3299404806269776169, 0.3333333333333333703, 0.3299404806269776169, 0.3333333333333333703, 0.3299404806269776169, 0.3333333333333333703, 0.3299404806269776169, 0.3333333333333333703, 0.3299404806269776169, 0.3333333333333333703, 0.3299404806269776169, 0.3333333333333333703, 0.3299404806269776169, 0.3333333333333333703, 0.3299404806269776169, 0.3333333333333333703, 0.3299404806269776169, 0.3333333333333333703, 0.3299404806269776169, 0.3333333333333333703, 0.3299404806269776169, 0.3333333333333333703, 0.3299404806269776169, 0.3333333333333333703, 0.3299404806269776169, 0.3333333333333333703, 0.3299404806269776169, 0.3333333333333333703, 0.3299404806269776169, 0.3333333333333333703, 0.3299404806269776169, 0.3333333333333333703, 0.3299404806269776169, 0.3333333333333333703, 0.3299404806269776169, 0.3333333333333333703, 0.3299404806269776169, 0.3333333333333333703, 0.3299404806269776169, 0.3333333333333333703, 0.3299404806269776169, 0.3333333333333333703, 0.3299404806269776169, 0.3333333333333333703, 0.3299404806269776169, 0.3333333333333333703, 0.3299404806269776169, 0.3333333333333333703, 0.3299404806269776169, 0.3333333333333333703, 0.3299404806269776169, 0.3333333333333333703, 0.3299404806269776169, 0.3333333333333333703, 0.3299404806269776169, 0.3333333333333333703, 0.3299404806269776169, 0.3333333333333333703, 0.3299404806269776169, 0.3333333333333333703, 0.3299404806269776169, 0.3333333333333333703, 0.3299404806269776169, 0.3333333333333333703, 0.3299404806269776169, 0.3333333333333333703, 0.3299404806269776169, 0.3333333333333333703, 0.3299404806269776169, 0.3333333333333333703, 0.3299404806269776169, 0.3333333333333333703, 0.3299404806269776169, 0.3333333333333333703, 0.3299404806269776169, 0.3333333333333333703, 0.3299404806269776169, 0.3333333333333333703, 0.3299404806269776169, 0.3333333333333333703, 0.3299404806269776169, 0.3333333333333333703, 0.3299404806269776169, 0.3333333333333333703, 0.3299404806269776169, 0.3333333333333333703, 0.3299404806269776169, 0.3333333333333333703, 0.3299404806269776169, 0.3333333333333333703, 0.3299404806269776169, 0.3333333333333333703, 0.3299404806269776169, 0.3333333333333333703, 0.3299404806269776169, 0.3333333333333333703, 0.3299404806269776169, 0.3333333333333333703, 0.3299404806269776169, 0.3333333333333333703, 0.3299404806269776169, 0.3333333333333333703, 0.3299404806269776169, 0.3333333333333333703, 0.3299404806269776169, 0.3333333333333333703, 0.3299404806269776169, 0.3333333333333333703, 0.3299404806269776169, 0.3333333333333333703, 0.3299404806269776169, 0.3333333333333333703, 0.3299404806269776169, 0.3333333333333333703, 0.3299404806269776169, 0.3333333333333333703, 0.3299404806269776169, 0.3333333333333333703, 0.3299404806269776169, 0.3333333333333333703, 0.3299404806269776169, 0.3333333333333333703, 0.3299404806269776169, 0.3333333333333333703, 0.3299404806269776169, 0.3333333333333333703, 0.3299404806269776169, 0.3333333333333333703, 0.3299404806269776169, 0.3333333333333333703, 0.3299404806269776169, 0.3333333333333333703, 0.3299404806269776169, 0.3333333333333333703, 0.3299404806269776169, 0.3333333333333333703, 0.3299404806269776169, 0.3333333333333333703, 0.3299404806269776169, 0.3333333333333333703, 0.3299404806269776169, 0.3333333333333333703, 0.3299404806269776169, 0.3333333333333333703, 0.3299404806269776169, 0.3333333333333333703, 0.3299404806269776169, 0.3333333333333333703, 0.3299404806269776169, 0.3333333333333333703, 0.3299404806269776169, 0.3333333333333333703, 0.3299404806269776169, 0.3333333333333333703, 0.3299404806269776169, 0.3333333333333333703, 0.3299404806269776169, 0.3333333333333333703, 0.3299404806269776169, 0.3333333333333333703, 0.3299404806269776169, 0.3333333333333333703, 0.3299404806269776169, 0.3333333333333333703, 0.3299404806269776169, 0.3333333333333333703, 0.3299404806269776169, 0.3333333333333333703, 0.3299404806269776169, 0.3333333333333333703, 0.3299404806269776169, 0.3333333333333333703, 0.3299404806269776169, 0.3333333333333333703, 0.3299404806269776169, 0.3333333333333333703, 0.3299404806269776169, 0.3333333333333333703, 0.3299404806269776169, 0.3333333333333333703, 0.3299404806269776169, 0.3333333333333333703, 0.3299404806269776169, 0.3333333333333333703, 0.3299404806269776169, 0.3333333333333333703, 0.3299404806269776169, 0.3333333333333333703, 0.3299404806269776169, 0.3333333333333333703, 0.3299404806269776169, 0.3333333333333333703, 0.3299404806269776169, 0.3333333333333333703, 0.3299404806269776169, 0.3333333333333333703, 0.3299404806269776169, 0.3333333333333333703, 0.3299404806269776169, 0.3333333333333333703, 0.3299404806269776169, 0.3333333333333333703, 0.3299404806269776169, 0.3333333333333333703, 0.3299404806269776169, 0.3333333333333333703, 0.3299404806269776169, 0.3333333333333333703, 0.3299404806269776169, 0.3333333333333333703, 0.3299404806269776169, 0.3333333333333333703, 0.3299404806269776169, 0.3333333333333333703, 0.3299404806269776169, 0.3333333333333333703, 0.3299404806269776169, 0.3333333333333333703, 0.3299404806269776169, 0.3333333333333333703, 0.3299404806269776169, 0.3333333333333333703, 0.3299404806269776169, 0.3333333333333333703, 0.3299404806269776169, 0.3333333333333333703, 0.3299404806269776169, 0.3333333333333333703, 0.3299404806269776169, 0.3333333333333333703, 0.3299404806269776169, 0.3333333333333333703, 0.3299404806269776169, 0.3333333333333333703, 0.3299404806269776169, 0.3333333333333333703, 0.3299404806269776169, 0.3333333333333333703, 0.3299404806269776169, 0.3333333333333333703, 0.3299404806269776169, 0.3333333333333333703, 0.3299404806269776169, 0.3333333333333333703, 0.3299404806269776169, 0.3333333333333333703, 0.3299404806269776169, 0.3333333333333333703, 0.3299404806269776169, 0.3333333333333333703, 0.3299404806269776169, 0.3333333333333333703, 0.3299404806269776169, 0.3333333333333333703, 0.3299404806269776169, 0.3333333333333333703, 0.3299404806269776169, 0.3333333333333333703, 0.3299404806269776169, 0.3333333333333333703, 0.3299404806269776169, 0.3333333333333333703, 0.3299404806269776169, 0.3333333333333333703, 0.3299404806269776169, 0.3333333333333333703, 0.3299404806269776169, 0.3333333333333333703, 0.3299404806269776169, 0.3333333333333333703, 0.3299404806269776169, 0.3333333333333333703, 0.3299404806269776169, 0.3333333333333333703, 0.3299404806269776169, 0.3333333333333333703, 0.3299404806269776169, 0.3333333333333333703, 0.3299404806269776169, 0.3333333333333333703, 0.3299404806269776169, 0.3333333333333333703, 0.3299404806269776169, 0.3333333333333333703, 0.3299404806269776169, 0.3333333333333333703, 0.3299404806269776169, 0.3333333333333333703, 0.3299404806269776169, 0.3333333333333333703, 0.3299404806269776169, 0.3333333333333333703, 0.3299404806269776169, 0.3333333333333333703, 0.3299404806269776169, 0.3333333333333333703, 0.3299404806269776169, 0.3333333333333333703, 0.3299404806269776169, 0.3333333333333333703, 0.3299404806269776169, 0.3333333333333333703, 0.3299404806269776169, 0.3333333333333333703, 0.3299404806269776169, 0.3333333333333333703, 0.3299404806269776169, 0.3333333333333333703, 0.3299404806269776169, 0.3333333333333333703, 0.3299404806269776169, 0.3333333333333333703, 0.3299404806269776169, 0.3333333333333333703, 0.3299404806269776169, 0.3333333333333333703, 0.3299404806269776169, 0.3333333333333333703, 0.3299404806269776169, 0.3333333333333333703, 0.3299404806269776169, 0.3333333333333333703, 0.3299404806269776169, 0.3333333333333333703, 0.3299404806269776169, 0.3333333333333333703, 0.3299404806269776169, 0.3333333333333333703, 0.3299404806269776169, 0.3333333333333333703, 0.3299404806269776169, 0.3333333333333333703, 0.3299404806269776169, 0.3333333333333333703, 0.3299404806269776169, 0.3333333333333333703, 0.3299404806269776169, 0.3333333333333333703, 0.3299404806269776169, 0.3333333333333333703, 0.3299404806269776169, 0.3333333333333333703, 0.3299404806269776169, 0.3333333333333333703, 0.3299404806269776169, 0.3333333333333333703, 0.3299404806269776169, 0.3333333333333333703, 0.3299404806269776169, 0.3333333333333333703, 0.3299404806269776169, 0.3333333333333333703, 0.3299404806269776169, 0.3333333333333333703, 0.3299404806269776169, 0.3333333333333333703, 0.3299404806269776169, 0.3333333333333333703, 0.3299404806269776169, 0.3333333333333333703, 0.3299404806269776169, 0.3333333333333333703, 0.3299404806269776169, 0.3333333333333333703, 0.3299404806269776169, 0.3333333333333333703, 0.3299404806269776169, 0.3333333333333333703, 0.3299404806269776169, 0.3333333333333333703, 0.3299404806269776169, 0.3333333333333333703, 0.3299404806269776169, 0.3333333333333333703, 0.3299404806269776169, 0.3333333333333333703, 0.3299404806269776169, 0.3333333333333333703, 0.3299404806269776169, 0.3333333333333333703, 0.3299404806269776169, 0.3333333333333333703, 0.3299404806269776169, 0.3333333333333333703, 0.3299404806269776169, 0.3333333333333333703, 0.3299404806269776169, 0.3333333333333333703, 0.3299404806269776169, 0.3333333333333333703, 0.3299404806269776169, 0.3333333333333333703, 0.3299404806269776169, 0.3333333333333333703, 0.3299404806269776169, 0.3333333333333333703, 0.3299404806269776169, 0.3333333333333333703, 0.3299404806269776169, 0.3333333333333333703, 0.3299404806269776169, 0.3333333333333333703, 0.3299404806269776169, 0.3333333333333333703, 0.3320603117974822438, 0.3317425830320511193),
 ( 0.3333333333333333703, 0.3299404806269776169, 0.3333333333333333703, 0.3299404806269776169, 0.3333333333333333703, 0.3299404806269776169, 0.3333333333333333703, 0.3299404806269776169, 0.3333333333333333703, 0.3299404806269776169, 0.3333333333333333703, 0.3299404806269776169, 0.3333333333333333703, 0.3299404806269776169, 0.3333333333333333703, 0.3299404806269776169, 0.3333333333333333703, 0.3299404806269776169, 0.3333333333333333703, 0.3299404806269776169, 0.3333333333333333703, 0.3299404806269776169, 0.3333333333333333703, 0.3299404806269776169, 0.3333333333333333703, 0.3299404806269776169, 0.3333333333333333703, 0.3299404806269776169, 0.3333333333333333703, 0.3299404806269776169, 0.3333333333333333703, 0.3299404806269776169, 0.3333333333333333703, 0.3299404806269776169, 0.3333333333333333703, 0.3299404806269776169, 0.3333333333333333703, 0.3299404806269776169, 0.3333333333333333703, 0.3299404806269776169, 0.3333333333333333703, 0.3299404806269776169, 0.3333333333333333703, 0.3299404806269776169, 0.3333333333333333703, 0.3299404806269776169, 0.3333333333333333703, 0.3299404806269776169, 0.3333333333333333703, 0.3299404806269776169, 0.3333333333333333703, 0.3299404806269776169, 0.3333333333333333703, 0.3299404806269776169, 0.3333333333333333703, 0.3299404806269776169, 0.3333333333333333703, 0.3299404806269776169, 0.3333333333333333703, 0.3299404806269776169, 0.3333333333333333703, 0.3299404806269776169, 0.3333333333333333703, 0.3299404806269776169, 0.3333333333333333703, 0.3299404806269776169, 0.3333333333333333703, 0.3299404806269776169, 0.3333333333333333703, 0.3299404806269776169, 0.3333333333333333703, 0.3299404806269776169, 0.3333333333333333703, 0.3299404806269776169, 0.3333333333333333703, 0.3299404806269776169, 0.3333333333333333703, 0.3299404806269776169, 0.3333333333333333703, 0.3299404806269776169, 0.3333333333333333703, 0.3299404806269776169, 0.3333333333333333703, 0.3299404806269776169, 0.3333333333333333703, 0.3299404806269776169, 0.3333333333333333703, 0.3299404806269776169, 0.3333333333333333703, 0.3299404806269776169, 0.3333333333333333703, 0.3299404806269776169, 0.3333333333333333703, 0.3299404806269776169, 0.3333333333333333703, 0.3299404806269776169, 0.3333333333333333703, 0.3299404806269776169, 0.3333333333333333703, 0.3299404806269776169, 0.3333333333333333703, 0.3299404806269776169, 0.3333333333333333703, 0.3299404806269776169, 0.3333333333333333703, 0.3299404806269776169, 0.3333333333333333703, 0.3299404806269776169, 0.3333333333333333703, 0.3299404806269776169, 0.3333333333333333703, 0.3299404806269776169, 0.3333333333333333703, 0.3299404806269776169, 0.3333333333333333703, 0.3299404806269776169, 0.3333333333333333703, 0.3299404806269776169, 0.3333333333333333703, 0.3299404806269776169, 0.3333333333333333703, 0.3299404806269776169, 0.3333333333333333703, 0.3299404806269776169, 0.3333333333333333703, 0.3299404806269776169, 0.3333333333333333703, 0.3299404806269776169, 0.3333333333333333703, 0.3299404806269776169, 0.3333333333333333703, 0.3299404806269776169, 0.3333333333333333703, 0.3299404806269776169, 0.3333333333333333703, 0.3299404806269776169, 0.3333333333333333703, 0.3299404806269776169, 0.3333333333333333703, 0.3299404806269776169, 0.3333333333333333703, 0.3299404806269776169, 0.3333333333333333703, 0.3299404806269776169, 0.3333333333333333703, 0.3299404806269776169, 0.3333333333333333703, 0.3299404806269776169, 0.3333333333333333703, 0.3299404806269776169, 0.3333333333333333703, 0.3299404806269776169, 0.3333333333333333703, 0.3299404806269776169, 0.3333333333333333703, 0.3299404806269776169, 0.3333333333333333703, 0.3299404806269776169, 0.3333333333333333703, 0.3299404806269776169, 0.3333333333333333703, 0.3299404806269776169, 0.3333333333333333703, 0.3299404806269776169, 0.3333333333333333703, 0.3299404806269776169, 0.3333333333333333703, 0.3299404806269776169, 0.3333333333333333703, 0.3299404806269776169, 0.3333333333333333703, 0.3299404806269776169, 0.3333333333333333703, 0.3299404806269776169, 0.3333333333333333703, 0.3299404806269776169, 0.3333333333333333703, 0.3299404806269776169, 0.3333333333333333703, 0.3299404806269776169, 0.3333333333333333703, 0.3299404806269776169, 0.3333333333333333703, 0.3299404806269776169, 0.3333333333333333703, 0.3299404806269776169, 0.3333333333333333703, 0.3299404806269776169, 0.3333333333333333703, 0.3299404806269776169, 0.3333333333333333703, 0.3299404806269776169, 0.3333333333333333703, 0.3299404806269776169, 0.3333333333333333703, 0.3299404806269776169, 0.3333333333333333703, 0.3299404806269776169, 0.3333333333333333703, 0.3299404806269776169, 0.3333333333333333703, 0.3299404806269776169, 0.3333333333333333703, 0.3299404806269776169, 0.3333333333333333703, 0.3299404806269776169, 0.3333333333333333703, 0.3299404806269776169, 0.3333333333333333703, 0.3299404806269776169, 0.3333333333333333703, 0.3299404806269776169, 0.3333333333333333703, 0.3299404806269776169, 0.3333333333333333703, 0.3299404806269776169, 0.3333333333333333703, 0.3299404806269776169, 0.3333333333333333703, 0.3299404806269776169, 0.3333333333333333703, 0.3299404806269776169, 0.3333333333333333703, 0.3299404806269776169, 0.3333333333333333703, 0.3299404806269776169, 0.3333333333333333703, 0.3299404806269776169, 0.3333333333333333703, 0.3299404806269776169, 0.3333333333333333703, 0.3299404806269776169, 0.3333333333333333703, 0.3299404806269776169, 0.3333333333333333703, 0.3299404806269776169, 0.3333333333333333703, 0.3299404806269776169, 0.3333333333333333703, 0.3299404806269776169, 0.3333333333333333703, 0.3299404806269776169, 0.3333333333333333703, 0.3299404806269776169, 0.3333333333333333703, 0.3299404806269776169, 0.3333333333333333703, 0.3299404806269776169, 0.3333333333333333703, 0.3299404806269776169, 0.3333333333333333703, 0.3299404806269776169, 0.3333333333333333703, 0.3299404806269776169, 0.3333333333333333703, 0.3299404806269776169, 0.3333333333333333703, 0.3299404806269776169, 0.3333333333333333703, 0.3299404806269776169, 0.3333333333333333703, 0.3299404806269776169, 0.3333333333333333703, 0.3299404806269776169, 0.3333333333333333703, 0.3299404806269776169, 0.3333333333333333703, 0.3299404806269776169, 0.3333333333333333703, 0.3299404806269776169, 0.3333333333333333703, 0.3299404806269776169, 0.3333333333333333703, 0.3299404806269776169, 0.3333333333333333703, 0.3299404806269776169, 0.3333333333333333703, 0.3299404806269776169, 0.3333333333333333703, 0.3299404806269776169, 0.3333333333333333703, 0.3299404806269776169, 0.3333333333333333703, 0.3299404806269776169, 0.3333333333333333703, 0.3299404806269776169, 0.3333333333333333703, 0.3299404806269776169, 0.3333333333333333703, 0.3299404806269776169, 0.3333333333333333703, 0.3299404806269776169, 0.3333333333333333703, 0.3299404806269776169, 0.3333333333333333703, 0.3299404806269776169, 0.3333333333333333703, 0.3299404806269776169, 0.3333333333333333703, 0.3299404806269776169, 0.3333333333333333703, 0.3299404806269776169, 0.3333333333333333703, 0.3299404806269776169, 0.3333333333333333703, 0.3299404806269776169, 0.3333333333333333703, 0.3299404806269776169, 0.3333333333333333703, 0.3299404806269776169, 0.3333333333333333703, 0.3299404806269776169, 0.3333333333333333703, 0.3299404806269776169, 0.3333333333333333703, 0.3299404806269776169, 0.3333333333333333703, 0.3299404806269776169, 0.3333333333333333703, 0.3299404806269776169, 0.3333333333333333703, 0.3299404806269776169, 0.3333333333333333703, 0.3299404806269776169, 0.3333333333333333703, 0.3299404806269776169, 0.3333333333333333703, 0.3299404806269776169, 0.3333333333333333703, 0.3299404806269776169, 0.3333333333333333703, 0.3299404806269776169, 0.3333333333333333703, 0.3299404806269776169, 0.3333333333333333703, 0.3299404806269776169, 0.3333333333333333703, 0.3299404806269776169, 0.3333333333333333703, 0.3299404806269776169, 0.3333333333333333703, 0.3299404806269776169, 0.3333333333333333703, 0.3299404806269776169, 0.3333333333333333703, 0.3299404806269776169, 0.3333333333333333703, 0.3299404806269776169, 0.3333333333333333703, 0.3299404806269776169, 0.3333333333333333703, 0.3299404806269776169, 0.3333333333333333703, 0.3299404806269776169, 0.3333333333333333703, 0.3299404806269776169, 0.3333333333333333703, 0.3299404806269776169, 0.3333333333333333703, 0.3299404806269776169, 0.3333333333333333703, 0.3299404806269776169, 0.3333333333333333703, 0.3299404806269776169, 0.3333333333333333703, 0.3299404806269776169, 0.3333333333333333703, 0.3299404806269776169, 0.3333333333333333703, 0.3299404806269776169, 0.3333333333333333703, 0.3299404806269776169, 0.3333333333333333703, 0.3299404806269776169, 0.3333333333333333703, 0.3299404806269776169, 0.3333333333333333703, 0.3299404806269776169, 0.3333333333333333703, 0.3299404806269776169, 0.3333333333333333703, 0.3299404806269776169, 0.3333333333333333703, 0.3299404806269776169, 0.3333333333333333703, 0.3299404806269776169, 0.3333333333333333703, 0.3299404806269776169, 0.3333333333333333703, 0.3299404806269776169, 0.3333333333333333703, 0.3299404806269776169, 0.3333333333333333703, 0.3299404806269776169, 0.3333333333333333703, 0.3299404806269776169, 0.3333333333333333703, 0.3299404806269776169, 0.3333333333333333703, 0.3299404806269776169, 0.3333333333333333703, 0.3299404806269776169, 0.3333333333333333703, 0.3299404806269776169, 0.3333333333333333703, 0.3299404806269776169, 0.3333333333333333703, 0.3299404806269776169, 0.3333333333333333703, 0.3299404806269776169, 0.3333333333333333703, 0.3299404806269776169, 0.3333333333333333703, 0.3299404806269776169, 0.3333333333333333703, 0.3299404806269776169, 0.3333333333333333703, 0.3299404806269776169, 0.3333333333333333703, 0.3299404806269776169, 0.3333333333333333703, 0.3299404806269776169, 0.3333333333333333703, 0.3299404806269776169, 0.3333333333333333703, 0.3299404806269776169, 0.3333333333333333703, 0.3299404806269776169, 0.3333333333333333703, 0.3299404806269776169, 0.3333333333333333703, 0.3299404806269776169, 0.3333333333333333703, 0.3299404806269776169, 0.3333333333333333703, 0.3299404806269776169, 0.3333333333333333703, 0.3299404806269776169, 0.3333333333333333703, 0.3299404806269776169, 0.3333333333333333703, 0.3299404806269776169, 0.3333333333333333703, 0.3299404806269776169, 0.3333333333333333703, 0.3299404806269776169, 0.3333333333333333703, 0.3299404806269776169, 0.3333333333333333703, 0.3299404806269776169, 0.3333333333333333703, 0.3299404806269776169, 0.3333333333333333703, 0.3299404806269776169, 0.3333333333333333703, 0.3299404806269776169, 0.3333333333333333703, 0.3299404806269776169, 0.3333333333333333703, 0.3299404806269776169, 0.3333333333333333703, 0.3299404806269776169, 0.3333333333333333703, 0.3299404806269776169, 0.3333333333333333703, 0.3299404806269776169, 0.3333333333333333703, 0.3299404806269776169, 0.3333333333333333703, 0.3299404806269776169, 0.3333333333333333703, 0.3299404806269776169, 0.3333333333333333703, 0.3299404806269776169, 0.3333333333333333703, 0.3299404806269776169, 0.3333333333333333703, 0.3299404806269776169, 0.3333333333333333703, 0.3299404806269776169, 0.3333333333333333703, 0.3299404806269776169, 0.3333333333333333703, 0.3299404806269776169, 0.3333333333333333703, 0.3299404806269776169, 0.3333333333333333703, 0.3299404806269776169, 0.3333333333333333703, 0.3299404806269776169, 0.3333333333333333703, 0.3299404806269776169, 0.3333333333333333703, 0.3299404806269776169, 0.3333333333333333703, 0.3299404806269776169, 0.3333333333333333703, 0.3299404806269776169, 0.3333333333333333703, 0.3299404806269776169, 0.3333333333333333703, 0.3299404806269776169, 0.3333333333333333703, 0.3299404806269776169, 0.3333333333333333703, 0.3299404806269776169, 0.3333333333333333703, 0.3299404806269776169, 0.3333333333333333703, 0.3299404806269776169, 0.3333333333333333703, 0.3299404806269776169, 0.3333333333333333703, 0.3299404806269776169, 0.3333333333333333703, 0.3299404806269776169, 0.3333333333333333703, 0.3299404806269776169, 0.3333333333333333703, 0.3299404806269776169, 0.3333333333333333703, 0.3299404806269776169, 0.3333333333333333703, 0.3299404806269776169, 0.3333333333333333703, 0.3299404806269776169, 0.3333333333333333703, 0.3299404806269776169, 0.3333333333333333703, 0.3299404806269776169, 0.3333333333333333703, 0.3299404806269776169, 0.3333333333333333703, 0.3299404806269776169, 0.3333333333333333703, 0.3299404806269776169, 0.3333333333333333703, 0.3299404806269776169, 0.3333333333333333703, 0.3299404806269776169, 0.3333333333333333703, 0.3299404806269776169, 0.3333333333333333703, 0.3299404806269776169, 0.3333333333333333703, 0.3299404806269776169, 0.3333333333333333703, 0.3299404806269776169, 0.3333333333333333703, 0.3299404806269776169, 0.3333333333333333703, 0.3299404806269776169, 0.3333333333333333703, 0.3299404806269776169, 0.3333333333333333703, 0.3299404806269776169, 0.3333333333333333703, 0.3299404806269776169, 0.3333333333333333703, 0.3299404806269776169, 0.3333333333333333703, 0.3299404806269776169, 0.3333333333333333703, 0.3299404806269776169, 0.3333333333333333703, 0.3299404806269776169, 0.3333333333333333703, 0.3299404806269776169, 0.3333333333333333703, 0.3299404806269776169, 0.3333333333333333703, 0.3299404806269776169, 0.3333333333333333703, 0.3299404806269776169, 0.3333333333333333703, 0.3299404806269776169, 0.3333333333333333703, 0.3299404806269776169, 0.3333333333333333703, 0.3299404806269776169, 0.3333333333333333703, 0.3299404806269776169, 0.3333333333333333703, 0.3299404806269776169, 0.3333333333333333703, 0.3299404806269776169, 0.3333333333333333703, 0.3299404806269776169, 0.3333333333333333703, 0.3299404806269776169, 0.3333333333333333703, 0.3299404806269776169, 0.3333333333333333703, 0.3299404806269776169, 0.3333333333333333703, 0.3299404806269776169, 0.3333333333333333703, 0.3299404806269776169, 0.3333333333333333703, 0.3299404806269776169, 0.3333333333333333703, 0.3299404806269776169, 0.3333333333333333703, 0.3299404806269776169, 0.3333333333333333703, 0.3299404806269776169, 0.3333333333333333703, 0.3299404806269776169, 0.3333333333333333703, 0.3299404806269776169, 0.3333333333333333703, 0.3299404806269776169, 0.3333333333333333703, 0.3299404806269776169, 0.3333333333333333703, 0.3299404806269776169, 0.3333333333333333703, 0.3299404806269776169, 0.3333333333333333703, 0.3299404806269776169, 0.3333333333333333703, 0.3299404806269776169, 0.3333333333333333703, 0.3299404806269776169, 0.3333333333333333703, 0.3299404806269776169, 0.3333333333333333703, 0.3299404806269776169, 0.3333333333333333703, 0.3299404806269776169, 0.3333333333333333703, 0.3299404806269776169, 0.3333333333333333703, 0.3299404806269776169, 0.3333333333333333703, 0.3299404806269776169, 0.3333333333333333703, 0.3299404806269776169, 0.3333333333333333703, 0.3299404806269776169, 0.3333333333333333703, 0.3299404806269776169, 0.3333333333333333703, 0.3299404806269776169, 0.3333333333333333703, 0.3299404806269776169, 0.3333333333333333703, 0.3299404806269776169, 0.3333333333333333703, 0.3299404806269776169, 0.3333333333333333703, 0.3299404806269776169, 0.3333333333333333703, 0.3299404806269776169, 0.3333333333333333703, 0.3299404806269776169, 0.3333333333333333703, 0.3299404806269776169, 0.3333333333333333703, 0.3299404806269776169, 0.3333333333333333703, 0.3299404806269776169, 0.3333333333333333703, 0.3299404806269776169, 0.3333333333333333703, 0.3299404806269776169, 0.3333333333333333703, 0.3299404806269776169, 0.3333333333333333703, 0.3299404806269776169, 0.3333333333333333703, 0.3299404806269776169, 0.3333333333333333703, 0.3299404806269776169, 0.3333333333333333703, 0.3299404806269776169, 0.3333333333333333703, 0.3299404806269776169, 0.3333333333333333703, 0.3299404806269776169, 0.3333333333333333703, 0.3299404806269776169, 0.3333333333333333703, 0.3299404806269776169, 0.3333333333333333703, 0.3299404806269776169, 0.3333333333333333703, 0.3299404806269776169, 0.3333333333333333703, 0.3299404806269776169, 0.3333333333333333703, 0.3299404806269776169, 0.3333333333333333703, 0.3299404806269776169, 0.3333333333333333703, 0.3299404806269776169, 0.3333333333333333703, 0.3299404806269776169, 0.3333333333333333703, 0.3299404806269776169, 0.3333333333333333703, 0.3299404806269776169, 0.3333333333333333703, 0.3299404806269776169, 0.3333333333333333703, 0.3299404806269776169, 0.3333333333333333703, 0.3299404806269776169, 0.3333333333333333703, 0.3299404806269776169, 0.3333333333333333703, 0.3299404806269776169, 0.3333333333333333703, 0.3299404806269776169, 0.3333333333333333703, 0.3299404806269776169, 0.3333333333333333703, 0.3299404806269776169, 0.3333333333333333703, 0.3299404806269776169, 0.3333333333333333703, 0.3299404806269776169, 0.3333333333333333703, 0.3299404806269776169, 0.3333333333333333703, 0.3299404806269776169, 0.3333333333333333703, 0.3299404806269776169, 0.3333333333333333703, 0.3299404806269776169, 0.3333333333333333703, 0.3299404806269776169, 0.3333333333333333703, 0.3299404806269776169, 0.3333333333333333703, 0.3299404806269776169, 0.3333333333333333703, 0.3299404806269776169, 0.3333333333333333703, 0.3299404806269776169, 0.3333333333333333703, 0.3299404806269776169, 0.3333333333333333703, 0.3299404806269776169, 0.3333333333333333703, 0.3299404806269776169, 0.3333333333333333703, 0.3299404806269776169, 0.3333333333333333703, 0.3299404806269776169, 0.3333333333333333703, 0.3299404806269776169, 0.3333333333333333703, 0.3299404806269776169, 0.3333333333333333703, 0.3299404806269776169, 0.3333333333333333703, 0.3299404806269776169, 0.3333333333333333703, 0.3299404806269776169, 0.3333333333333333703, 0.3299404806269776169, 0.3333333333333333703, 0.3299404806269776169, 0.3333333333333333703, 0.3299404806269776169, 0.3333333333333333703, 0.3299404806269776169, 0.3333333333333333703, 0.3299404806269776169, 0.3333333333333333703, 0.3299404806269776169, 0.3333333333333333703, 0.3299404806269776169, 0.3333333333333333703, 0.3299404806269776169, 0.3333333333333333703, 0.3299404806269776169, 0.3333333333333333703, 0.3299404806269776169, 0.3333333333333333703, 0.3299404806269776169, 0.3333333333333333703, 0.3299404806269776169, 0.3333333333333333703, 0.3299404806269776169, 0.3333333333333333703, 0.3299404806269776169, 0.3333333333333333703, 0.3299404806269776169, 0.3333333333333333703, 0.3299404806269776169, 0.3333333333333333703, 0.3299404806269776169, 0.3333333333333333703, 0.3299404806269776169, 0.3333333333333333703, 0.3299404806269776169, 0.3333333333333333703, 0.3299404806269776169, 0.3333333333333333703, 0.3299404806269776169, 0.3333333333333333703, 0.3299404806269776169, 0.3333333333333333703, 0.3299404806269776169, 0.3333333333333333703, 0.3299404806269776169, 0.3333333333333333703, 0.3299404806269776169, 0.3333333333333333703, 0.3299404806269776169, 0.3333333333333333703, 0.3299404806269776169, 0.3333333333333333703, 0.3299404806269776169, 0.3333333333333333703, 0.3299404806269776169, 0.3333333333333333703, 0.3299404806269776169, 0.3333333333333333703, 0.3299404806269776169, 0.3333333333333333703, 0.3299404806269776169, 0.3333333333333333703, 0.3299404806269776169, 0.3333333333333333703, 0.3299404806269776169, 0.3333333333333333703, 0.3299404806269776169, 0.3333333333333333703, 0.3299404806269776169, 0.3333333333333333703, 0.3299404806269776169, 0.3333333333333333703, 0.3299404806269776169, 0.3333333333333333703, 0.3299404806269776169, 0.3333333333333333703, 0.3299404806269776169, 0.3333333333333333703, 0.3299404806269776169, 0.3333333333333333703, 0.3299404806269776169, 0.3333333333333333703, 0.3299404806269776169, 0.3333333333333333703, 0.3299404806269776169, 0.3333333333333333703, 0.3299404806269776169, 0.3333333333333333703, 0.3299404806269776169, 0.3333333333333333703, 0.3299404806269776169, 0.3333333333333333703, 0.3299404806269776169, 0.3333333333333333703, 0.3299404806269776169, 0.3333333333333333703, 0.3299404806269776169, 0.3333333333333333703, 0.3320603117974822438, 0.3317425830320511193),
 ( 1.000000000000000000, 0.9898214418809326842, 1.000000000000000000, 0.9898214418809326842, 1.000000000000000000, 0.9898214418809326842, 1.000000000000000000, 0.9898214418809326842, 1.000000000000000000, 0.9898214418809326842, 1.000000000000000000, 0.9898214418809326842, 1.000000000000000000, 0.9898214418809326842, 1.000000000000000000, 0.9898214418809326842, 1.000000000000000000, 0.9898214418809326842, 1.000000000000000000, 0.9898214418809326842, 1.000000000000000000, 0.9898214418809326842, 1.000000000000000000, 0.9898214418809326842, 1.000000000000000000, 0.9898214418809326842, 1.000000000000000000, 0.9898214418809326842, 1.000000000000000000, 0.9898214418809326842, 1.000000000000000000, 0.9898214418809326842, 1.000000000000000000, 0.9898214418809326842, 1.000000000000000000, 0.9898214418809326842, 1.000000000000000000, 0.9898214418809326842, 1.000000000000000000, 0.9898214418809326842, 1.000000000000000000, 0.9898214418809326842, 1.000000000000000000, 0.9898214418809326842, 1.000000000000000000, 0.9898214418809326842, 1.000000000000000000, 0.9898214418809326842, 1.000000000000000000, 0.9898214418809326842, 1.000000000000000000, 0.9898214418809326842, 1.000000000000000000, 0.9898214418809326842, 1.000000000000000000, 0.9898214418809326842, 1.000000000000000000, 0.9898214418809326842, 1.000000000000000000, 0.9898214418809326842, 1.000000000000000000, 0.9898214418809326842, 1.000000000000000000, 0.9898214418809326842, 1.000000000000000000, 0.9898214418809326842, 1.000000000000000000, 0.9898214418809326842, 1.000000000000000000, 0.9898214418809326842, 1.000000000000000000, 0.9898214418809326842, 1.000000000000000000, 0.9898214418809326842, 1.000000000000000000, 0.9898214418809326842, 1.000000000000000000, 0.9898214418809326842, 1.000000000000000000, 0.9898214418809326842, 1.000000000000000000, 0.9898214418809326842, 1.000000000000000000, 0.9898214418809326842, 1.000000000000000000, 0.9898214418809326842, 1.000000000000000000, 0.9898214418809326842, 1.000000000000000000, 0.9898214418809326842, 1.000000000000000000, 0.9898214418809326842, 1.000000000000000000, 0.9898214418809326842, 1.000000000000000000, 0.9898214418809326842, 1.000000000000000000, 0.9898214418809326842, 1.000000000000000000, 0.9898214418809326842, 1.000000000000000000, 0.9898214418809326842, 1.000000000000000000, 0.9898214418809326842, 1.000000000000000000, 0.9898214418809326842, 1.000000000000000000, 0.9898214418809326842, 1.000000000000000000, 0.9898214418809326842, 1.000000000000000000, 0.9898214418809326842, 1.000000000000000000, 0.9898214418809326842, 1.000000000000000000, 0.9898214418809326842, 1.000000000000000000, 0.9898214418809326842, 1.000000000000000000, 0.9898214418809326842, 1.000000000000000000, 0.9898214418809326842, 1.000000000000000000, 0.9898214418809326842, 1.000000000000000000, 0.9898214418809326842, 1.000000000000000000, 0.9898214418809326842, 1.000000000000000000, 0.9898214418809326842, 1.000000000000000000, 0.9898214418809326842, 1.000000000000000000, 0.9898214418809326842, 1.000000000000000000, 0.9898214418809326842, 1.000000000000000000, 0.9898214418809326842, 1.000000000000000000, 0.9898214418809326842, 1.000000000000000000, 0.9898214418809326842, 1.000000000000000000, 0.9898214418809326842, 1.000000000000000000, 0.9898214418809326842, 1.000000000000000000, 0.9898214418809326842, 1.000000000000000000, 0.9898214418809326842, 1.000000000000000000, 0.9898214418809326842, 1.000000000000000000, 0.9898214418809326842, 1.000000000000000000, 0.9898214418809326842, 1.000000000000000000, 0.9898214418809326842, 1.000000000000000000, 0.9898214418809326842, 1.000000000000000000, 0.9898214418809326842, 1.000000000000000000, 0.9898214418809326842, 1.000000000000000000, 0.9898214418809326842, 1.000000000000000000, 0.9898214418809326842, 1.000000000000000000, 0.9898214418809326842, 1.000000000000000000, 0.9898214418809326842, 1.000000000000000000, 0.9898214418809326842, 1.000000000000000000, 0.9898214418809326842, 1.000000000000000000, 0.9898214418809326842, 1.000000000000000000, 0.9898214418809326842, 1.000000000000000000, 0.9898214418809326842, 1.000000000000000000, 0.9898214418809326842, 1.000000000000000000, 0.9898214418809326842, 1.000000000000000000, 0.9898214418809326842, 1.000000000000000000, 0.9898214418809326842, 1.000000000000000000, 0.9898214418809326842, 1.000000000000000000, 0.9898214418809326842, 1.000000000000000000, 0.9898214418809326842, 1.000000000000000000, 0.9898214418809326842, 1.000000000000000000, 0.9898214418809326842, 1.000000000000000000, 0.9898214418809326842, 1.000000000000000000, 0.9898214418809326842, 1.000000000000000000, 0.9898214418809326842, 1.000000000000000000, 0.9898214418809326842, 1.000000000000000000, 0.9898214418809326842, 1.000000000000000000, 0.9898214418809326842, 1.000000000000000000, 0.9898214418809326842, 1.000000000000000000, 0.9898214418809326842, 1.000000000000000000, 0.9898214418809326842, 1.000000000000000000, 0.9898214418809326842, 1.000000000000000000, 0.9898214418809326842, 1.000000000000000000, 0.9898214418809326842, 1.000000000000000000, 0.9898214418809326842, 1.000000000000000000, 0.9898214418809326842, 1.000000000000000000, 0.9898214418809326842, 1.000000000000000000, 0.9898214418809326842, 1.000000000000000000, 0.9898214418809326842, 1.000000000000000000, 0.9898214418809326842, 1.000000000000000000, 0.9898214418809326842, 1.000000000000000000, 0.9898214418809326842, 1.000000000000000000, 0.9898214418809326842, 1.000000000000000000, 0.9898214418809326842, 1.000000000000000000, 0.9898214418809326842, 1.000000000000000000, 0.9898214418809326842, 1.000000000000000000, 0.9898214418809326842, 1.000000000000000000, 0.9898214418809326842, 1.000000000000000000, 0.9898214418809326842, 1.000000000000000000, 0.9898214418809326842, 1.000000000000000000, 0.9898214418809326842, 1.000000000000000000, 0.9898214418809326842, 1.000000000000000000, 0.9898214418809326842, 1.000000000000000000, 0.9898214418809326842, 1.000000000000000000, 0.9898214418809326842, 1.000000000000000000, 0.9898214418809326842, 1.000000000000000000, 0.9898214418809326842, 1.000000000000000000, 0.9898214418809326842, 1.000000000000000000, 0.9898214418809326842, 1.000000000000000000, 0.9898214418809326842, 1.000000000000000000, 0.9898214418809326842, 1.000000000000000000, 0.9898214418809326842, 1.000000000000000000, 0.9898214418809326842, 1.000000000000000000, 0.9898214418809326842, 1.000000000000000000, 0.9898214418809326842, 1.000000000000000000, 0.9898214418809326842, 1.000000000000000000, 0.9898214418809326842, 1.000000000000000000, 0.9898214418809326842, 1.000000000000000000, 0.9898214418809326842, 1.000000000000000000, 0.9898214418809326842, 1.000000000000000000, 0.9898214418809326842, 1.000000000000000000, 0.9898214418809326842, 1.000000000000000000, 0.9898214418809326842, 1.000000000000000000, 0.9898214418809326842, 1.000000000000000000, 0.9898214418809326842, 1.000000000000000000, 0.9898214418809326842, 1.000000000000000000, 0.9898214418809326842, 1.000000000000000000, 0.9898214418809326842, 1.000000000000000000, 0.9898214418809326842, 1.000000000000000000, 0.9898214418809326842, 1.000000000000000000, 0.9898214418809326842, 1.000000000000000000, 0.9898214418809326842, 1.000000000000000000, 0.9898214418809326842, 1.000000000000000000, 0.9898214418809326842, 1.000000000000000000, 0.9898214418809326842, 1.000000000000000000, 0.9898214418809326842, 1.000000000000000000, 0.9898214418809326842, 1.000000000000000000, 0.9898214418809326842, 1.000000000000000000, 0.9898214418809326842, 1.000000000000000000, 0.9898214418809326842, 1.000000000000000000, 0.9898214418809326842, 1.000000000000000000, 0.9898214418809326842, 1.000000000000000000, 0.9898214418809326842, 1.000000000000000000, 0.9898214418809326842, 1.000000000000000000, 0.9898214418809326842, 1.000000000000000000, 0.9898214418809326842, 1.000000000000000000, 0.9898214418809326842, 1.000000000000000000, 0.9898214418809326842, 1.000000000000000000, 0.9898214418809326842, 1.000000000000000000, 0.9898214418809326842, 1.000000000000000000, 0.9898214418809326842, 1.000000000000000000, 0.9898214418809326842, 1.000000000000000000, 0.9898214418809326842, 1.000000000000000000, 0.9898214418809326842, 1.000000000000000000, 0.9898214418809326842, 1.000000000000000000, 0.9898214418809326842, 1.000000000000000000, 0.9898214418809326842, 1.000000000000000000, 0.9898214418809326842, 1.000000000000000000, 0.9898214418809326842, 1.000000000000000000, 0.9898214418809326842, 1.000000000000000000, 0.9898214418809326842, 1.000000000000000000, 0.9898214418809326842, 1.000000000000000000, 0.9898214418809326842, 1.000000000000000000, 0.9898214418809326842, 1.000000000000000000, 0.9898214418809326842, 1.000000000000000000, 0.9898214418809326842, 1.000000000000000000, 0.9898214418809326842, 1.000000000000000000, 0.9898214418809326842, 1.000000000000000000, 0.9898214418809326842, 1.000000000000000000, 0.9898214418809326842, 1.000000000000000000, 0.9898214418809326842, 1.000000000000000000, 0.9898214418809326842, 1.000000000000000000, 0.9898214418809326842, 1.000000000000000000, 0.9898214418809326842, 1.000000000000000000, 0.9898214418809326842, 1.000000000000000000, 0.9898214418809326842, 1.000000000000000000, 0.9898214418809326842, 1.000000000000000000, 0.9898214418809326842, 1.000000000000000000, 0.9898214418809326842, 1.000000000000000000, 0.9898214418809326842, 1.000000000000000000, 0.9898214418809326842, 1.000000000000000000, 0.9898214418809326842, 1.000000000000000000, 0.9898214418809326842, 1.000000000000000000, 0.9898214418809326842, 1.000000000000000000, 0.9898214418809326842, 1.000000000000000000, 0.9898214418809326842, 1.000000000000000000, 0.9898214418809326842, 1.000000000000000000, 0.9898214418809326842, 1.000000000000000000, 0.9898214418809326842, 1.000000000000000000, 0.9898214418809326842, 1.000000000000000000, 0.9898214418809326842, 1.000000000000000000, 0.9898214418809326842, 1.000000000000000000, 0.9898214418809326842, 1.000000000000000000, 0.9898214418809326842, 1.000000000000000000, 0.9898214418809326842, 1.000000000000000000, 0.9898214418809326842, 1.000000000000000000, 0.9898214418809326842, 1.000000000000000000, 0.9898214418809326842, 1.000000000000000000, 0.9898214418809326842, 1.000000000000000000, 0.9898214418809326842, 1.000000000000000000, 0.9898214418809326842, 1.000000000000000000, 0.9898214418809326842, 1.000000000000000000, 0.9898214418809326842, 1.000000000000000000, 0.9898214418809326842, 1.000000000000000000, 0.9898214418809326842, 1.000000000000000000, 0.9898214418809326842, 1.000000000000000000, 0.9898214418809326842, 1.000000000000000000, 0.9898214418809326842, 1.000000000000000000, 0.9898214418809326842, 1.000000000000000000, 0.9898214418809326842, 1.000000000000000000, 0.9898214418809326842, 1.000000000000000000, 0.9898214418809326842, 1.000000000000000000, 0.9898214418809326842, 1.000000000000000000, 0.9898214418809326842, 1.000000000000000000, 0.9898214418809326842, 1.000000000000000000, 0.9898214418809326842, 1.000000000000000000, 0.9898214418809326842, 1.000000000000000000, 0.9898214418809326842, 1.000000000000000000, 0.9898214418809326842, 1.000000000000000000, 0.9898214418809326842, 1.000000000000000000, 0.9898214418809326842, 1.000000000000000000, 0.9898214418809326842, 1.000000000000000000, 0.9898214418809326842, 1.000000000000000000, 0.9898214418809326842, 1.000000000000000000, 0.9898214418809326842, 1.000000000000000000, 0.9898214418809326842, 1.000000000000000000, 0.9898214418809326842, 1.000000000000000000, 0.9898214418809326842, 1.000000000000000000, 0.9898214418809326842, 1.000000000000000000, 0.9898214418809326842, 1.000000000000000000, 0.9898214418809326842, 1.000000000000000000, 0.9898214418809326842, 1.000000000000000000, 0.9898214418809326842, 1.000000000000000000, 0.9898214418809326842, 1.000000000000000000, 0.9898214418809326842, 1.000000000000000000, 0.9898214418809326842, 1.000000000000000000, 0.9898214418809326842, 1.000000000000000000, 0.9898214418809326842, 1.000000000000000000, 0.9898214418809326842, 1.000000000000000000, 0.9898214418809326842, 1.000000000000000000, 0.9898214418809326842, 1.000000000000000000, 0.9898214418809326842, 1.000000000000000000, 0.9898214418809326842, 1.000000000000000000, 0.9898214418809326842, 1.000000000000000000, 0.9898214418809326842, 1.000000000000000000, 0.9898214418809326842, 1.000000000000000000, 0.9898214418809326842, 1.000000000000000000, 0.9898214418809326842, 1.000000000000000000, 0.9898214418809326842, 1.000000000000000000, 0.9898214418809326842, 1.000000000000000000, 0.9898214418809326842, 1.000000000000000000, 0.9898214418809326842, 1.000000000000000000, 0.9898214418809326842, 1.000000000000000000, 0.9898214418809326842, 1.000000000000000000, 0.9898214418809326842, 1.000000000000000000, 0.9898214418809326842, 1.000000000000000000, 0.9898214418809326842, 1.000000000000000000, 0.9898214418809326842, 1.000000000000000000, 0.9898214418809326842, 1.000000000000000000, 0.9898214418809326842, 1.000000000000000000, 0.9898214418809326842, 1.000000000000000000, 0.9898214418809326842, 1.000000000000000000, 0.9898214418809326842, 1.000000000000000000, 0.9898214418809326842, 1.000000000000000000, 0.9898214418809326842, 1.000000000000000000, 0.9898214418809326842, 1.000000000000000000, 0.9898214418809326842, 1.000000000000000000, 0.9898214418809326842, 1.000000000000000000, 0.9898214418809326842, 1.000000000000000000, 0.9898214418809326842, 1.000000000000000000, 0.9898214418809326842, 1.000000000000000000, 0.9898214418809326842, 1.000000000000000000, 0.9898214418809326842, 1.000000000000000000, 0.9898214418809326842, 1.000000000000000000, 0.9898214418809326842, 1.000000000000000000, 0.9898214418809326842, 1.000000000000000000, 0.9898214418809326842, 1.000000000000000000, 0.9898214418809326842, 1.000000000000000000, 0.9898214418809326842, 1.000000000000000000, 0.9898214418809326842, 1.000000000000000000, 0.9898214418809326842, 1.000000000000000000, 0.9898214418809326842, 1.000000000000000000, 0.9898214418809326842, 1.000000000000000000, 0.9898214418809326842, 1.000000000000000000, 0.9898214418809326842, 1.000000000000000000, 0.9898214418809326842, 1.000000000000000000, 0.9898214418809326842, 1.000000000000000000, 0.9898214418809326842, 1.000000000000000000, 0.9898214418809326842, 1.000000000000000000, 0.9898214418809326842, 1.000000000000000000, 0.9898214418809326842, 1.000000000000000000, 0.9898214418809326842, 1.000000000000000000, 0.9898214418809326842, 1.000000000000000000, 0.9898214418809326842, 1.000000000000000000, 0.9898214418809326842, 1.000000000000000000, 0.9898214418809326842, 1.000000000000000000, 0.9898214418809326842, 1.000000000000000000, 0.9898214418809326842, 1.000000000000000000, 0.9898214418809326842, 1.000000000000000000, 0.9898214418809326842, 1.000000000000000000, 0.9898214418809326842, 1.000000000000000000, 0.9898214418809326842, 1.000000000000000000, 0.9898214418809326842, 1.000000000000000000, 0.9898214418809326842, 1.000000000000000000, 0.9898214418809326842, 1.000000000000000000, 0.9898214418809326842, 1.000000000000000000, 0.9898214418809326842, 1.000000000000000000, 0.9898214418809326842, 1.000000000000000000, 0.9898214418809326842, 1.000000000000000000, 0.9898214418809326842, 1.000000000000000000, 0.9898214418809326842, 1.000000000000000000, 0.9898214418809326842, 1.000000000000000000, 0.9898214418809326842, 1.000000000000000000, 0.9898214418809326842, 1.000000000000000000, 0.9898214418809326842, 1.000000000000000000, 0.9898214418809326842, 1.000000000000000000, 0.9898214418809326842, 1.000000000000000000, 0.9898214418809326842, 1.000000000000000000, 0.9898214418809326842, 1.000000000000000000, 0.9898214418809326842, 1.000000000000000000, 0.9898214418809326842, 1.000000000000000000, 0.9898214418809326842, 1.000000000000000000, 0.9898214418809326842, 1.000000000000000000, 0.9898214418809326842, 1.000000000000000000, 0.9898214418809326842, 1.000000000000000000, 0.9898214418809326842, 1.000000000000000000, 0.9898214418809326842, 1.000000000000000000, 0.9898214418809326842, 1.000000000000000000, 0.9898214418809326842, 1.000000000000000000, 0.9898214418809326842, 1.000000000000000000, 0.9898214418809326842, 1.000000000000000000, 0.9898214418809326842, 1.000000000000000000, 0.9898214418809326842, 1.000000000000000000, 0.9898214418809326842, 1.000000000000000000, 0.9898214418809326842, 1.000000000000000000, 0.9898214418809326842, 1.000000000000000000, 0.9898214418809326842, 1.000000000000000000, 0.9898214418809326842, 1.000000000000000000, 0.9898214418809326842, 1.000000000000000000, 0.9898214418809326842, 1.000000000000000000, 0.9898214418809326842, 1.000000000000000000, 0.9898214418809326842, 1.000000000000000000, 0.9898214418809326842, 1.000000000000000000, 0.9898214418809326842, 1.000000000000000000, 0.9898214418809326842, 1.000000000000000000, 0.9898214418809326842, 1.000000000000000000, 0.9898214418809326842, 1.000000000000000000, 0.9898214418809326842, 1.000000000000000000, 0.9898214418809326842, 1.000000000000000000, 0.9898214418809326842, 1.000000000000000000, 0.9898214418809326842, 1.000000000000000000, 0.9898214418809326842, 1.000000000000000000, 0.9898214418809326842, 1.000000000000000000, 0.9898214418809326842, 1.000000000000000000, 0.9898214418809326842, 1.000000000000000000, 0.9898214418809326842, 1.000000000000000000, 0.9898214418809326842, 1.000000000000000000, 0.9898214418809326842, 1.000000000000000000, 0.9898214418809326842, 1.000000000000000000, 0.9898214418809326842, 1.000000000000000000, 0.9898214418809326842, 1.000000000000000000, 0.9898214418809326842, 1.000000000000000000, 0.9898214418809326842, 1.000000000000000000, 0.9898214418809326842, 1.000000000000000000, 0.9898214418809326842, 1.000000000000000000, 0.9898214418809326842, 1.000000000000000000, 0.9898214418809326842, 1.000000000000000000, 0.9898214418809326842, 1.000000000000000000, 0.9898214418809326842, 1.000000000000000000, 0.9898214418809326842, 1.000000000000000000, 0.9898214418809326842, 1.000000000000000000, 0.9898214418809326842, 1.000000000000000000, 0.9898214418809326842, 1.000000000000000000, 0.9898214418809326842, 1.000000000000000000, 0.9898214418809326842, 1.000000000000000000, 0.9898214418809326842, 1.000000000000000000, 0.9898214418809326842, 1.000000000000000000, 0.9898214418809326842, 1.000000000000000000, 0.9898214418809326842, 1.000000000000000000, 0.9898214418809326842, 1.000000000000000000, 0.9898214418809326842, 1.000000000000000000, 0.9898214418809326842, 1.000000000000000000, 0.9898214418809326842, 1.000000000000000000, 0.9898214418809326842, 1.000000000000000000, 0.9898214418809326842, 1.000000000000000000, 0.9898214418809326842, 1.000000000000000000, 0.9898214418809326842, 1.000000000000000000, 0.9898214418809326842, 1.000000000000000000, 0.9898214418809326842, 1.000000000000000000, 0.9898214418809326842, 1.000000000000000000, 0.9898214418809326842, 1.000000000000000000, 0.9898214418809326842, 1.000000000000000000, 0.9898214418809326842, 1.000000000000000000, 0.9898214418809326842, 1.000000000000000000, 0.9898214418809326842, 1.000000000000000000, 0.9898214418809326842, 1.000000000000000000, 0.9898214418809326842, 1.000000000000000000, 0.9898214418809326842, 1.000000000000000000, 0.9898214418809326842, 1.000000000000000000, 0.9898214418809326842, 1.000000000000000000, 0.9898214418809326842, 1.000000000000000000, 0.9898214418809326842, 1.000000000000000000, 0.9961809353924466759, 0.9952277490961531914) ) ) 
 REPRESENTATION_ITEM ( '' )  SURFACE ( )  );
#25891 = CARTESIAN_POINT ( 'NONE',  ( 745.1769319972822814, -161.8055962898689870, 346.2694204179732083 ) ) ;
#25892 = CARTESIAN_POINT ( 'NONE',  ( 805.1927285166397041, -16.81642084023866701, -341.8018195045277707 ) ) ;
#25893 = CARTESIAN_POINT ( 'NONE',  ( 760.5453621957607311, -117.0783235625963528, -323.8424801807151425 ) ) ;
#25894 = CARTESIAN_POINT ( 'NONE',  ( 792.1044303154645831, -132.4527844766018916, -317.8323909638837677 ) ) ;
#25895 = CARTESIAN_POINT ( 'NONE',  ( 783.7566961878529810, 23.10349461922137237, -305.1792804349288417 ) ) ;
#25897 = CARTESIAN_POINT ( 'NONE',  ( 805.1927285166399315, -256.8164208402379245, 341.8018195045277707 ) ) ;
#25896 = CARTESIAN_POINT ( 'NONE',  ( 792.1044303154645831, -252.4527844766015789, 317.8323909638837677 ) ) ;
#25898 = AXIS2_PLACEMENT_3D ( 'NONE', #16215, #37226, #26600 ) ;
#25899 = DIRECTION ( 'NONE',  ( -0.000000000000000000, 1.000000000000000000, -0.000000000000000000 ) ) ;
#25900 = ORIENTED_EDGE ( 'NONE', *, *, #21009, .F. ) ;
#25901 = CARTESIAN_POINT ( 'NONE',  ( 755.0488828828309806, 6.194403710130517382, 344.1219089521771934 ) ) ;
#25902 = ORIENTED_EDGE ( 'NONE', *, *, #40995, .T. ) ;
#25903 = SHAPE_REPRESENTATION_RELATIONSHIP ( 'NONE' , 'NONE' ,  #27662, #17201 ) ;
#25904 = CARTESIAN_POINT ( 'NONE',  ( 808.0189434323515343, -182.0891481129654323, 319.0252816721025511 ) ) ;
#25905 = CARTESIAN_POINT ( 'NONE',  ( 804.4086373105744769, -265.6454272087889876, 333.3843516231986541 ) ) ;
#25906 = CARTESIAN_POINT ( 'NONE',  ( 790.8726784830453198, -394.7146871989591546, 362.5472867521010585 ) ) ;
#25907 = ORIENTED_EDGE ( 'NONE', *, *, #40496, .T. ) ;
#25908 = CARTESIAN_POINT ( 'NONE',  ( 790.0220218866281812, -79.09997266333503774, -363.2186876482849129 ) ) ;
#25909 = CARTESIAN_POINT ( 'NONE',  ( 748.3538107759620743, -208.7146871989596946, 355.8262568251490165 ) ) ;
#25910 = CARTESIAN_POINT ( 'NONE',  ( 755.3201227861273992, -267.7255117493287457, -345.3687786644892981 ) ) ;
#25911 = ORIENTED_EDGE ( 'NONE', *, *, #19866, .F. ) ;
#25912 = CARTESIAN_POINT ( 'NONE',  ( 754.8072714833581358, -388.8164208402374129, -338.1981804954720587 ) ) ;
#25913 = CARTESIAN_POINT ( 'NONE',  ( 797.6776695296629214, -43.54369356751131903, -357.6776695296636603 ) ) ;
#25914 = CARTESIAN_POINT ( 'NONE',  ( 805.1016975059191054, -270.8965053807777394, 343.0745993439771837 ) ) ;
#25915 = DIRECTION ( 'NONE',  ( 0.000000000000000000, 0.000000000000000000, 1.000000000000000000 ) ) ;
#25916 = CARTESIAN_POINT ( 'NONE',  ( -338.8365100919713200, 256.5000000000001137, -199.9999999999917861 ) ) ;
#25917 = CARTESIAN_POINT ( 'NONE',  ( 802.2119215644370342, -30.00906357242607925, -367.5423716828165084 ) ) ;
#25918 = CARTESIAN_POINT ( 'NONE',  ( -521.6730038022808458, 9.808315785437627339E-14, 339.9999999999999432 ) ) ;
#25919 = VERTEX_POINT ( 'NONE', #2459 ) ;
#25920 = CARTESIAN_POINT ( 'NONE',  ( 773.7305795820266212, -321.2817908451525000, -374.8230680027170365 ) ) ;
#25921 = CARTESIAN_POINT ( 'NONE',  ( 768.9521613784389729, -177.8272453906074304, 373.2346286133773106 ) ) ;
#25923 = CARTESIAN_POINT ( 'NONE',  ( 788.8264449731200330, -309.1800572038740711, -363.6646147819171233 ) ) ;
#25922 = FACE_BOUND ( 'NONE', #23458, .T. ) ;
#25924 = CARTESIAN_POINT ( 'NONE',  ( 939.9999999999992042, 74.99999999999984368, 360.0000000000000000 ) ) ;
#25925 = CARTESIAN_POINT ( 'NONE',  ( 790.0220218866281812, -151.0999726633347677, -363.2186876482849129 ) ) ;
#25926 = CARTESIAN_POINT ( 'NONE',  ( 808.3070685750230950, -18.99823902205683979, 361.1904061080339261 ) ) ;
#25927 = VECTOR ( 'NONE', #45309, 1000.000000000000000 ) ;
#25928 = DIRECTION ( 'NONE',  ( 0.000000000000000000, 0.000000000000000000, 1.000000000000000000 ) ) ;
#25929 = CARTESIAN_POINT ( 'NONE',  ( 812.6845335610512393, -7.987414471687621642, -353.5525998758768651 ) ) ;
#25930 = CARTESIAN_POINT ( 'NONE',  ( 751.9810565676468741, -338.0891481129649492, -360.9747183278973921 ) ) ;
#25931 = DIRECTION ( 'NONE',  ( 0.3826814224632300032, 0.000000000000000000, -0.9238803650373347276 ) ) ;
#25932 = CARTESIAN_POINT ( 'NONE',  ( 754.8072714833581358, -28.81642084023863148, 338.1981804954720587 ) ) ;
#25933 = CARTESIAN_POINT ( 'NONE',  ( 797.8822607201568644, -270.5545181178798657, 370.1134526219340160 ) ) ;
#25934 = CARTESIAN_POINT ( 'NONE',  ( 791.1614460488616487, -251.2601417444141134, -373.5763878283158874 ) ) ;
#25935 = CARTESIAN_POINT ( 'NONE',  ( 814.9108240113580450, -256.2709662947834204, 337.5031285880265273 ) ) ;
#25936 = CARTESIAN_POINT ( 'NONE',  ( 792.3570229623688874, 2.819942796124898177, -373.1304606946836202 ) ) ;
#25937 = FACE_BOUND ( 'NONE', #1929, .T. ) ;
#25938 = VERTEX_POINT ( 'NONE', #26710 ) ;
#25939 = CARTESIAN_POINT ( 'NONE',  ( 797.6776695296629214, -355.5436935675103882, 357.6776695296636603 ) ) ;
#25940 = CARTESIAN_POINT ( 'NONE',  ( 793.0897708529556667, -102.5545181178804057, 361.3366627262616362 ) ) ;
#25941 = CARTESIAN_POINT ( 'NONE',  ( 798.7617431975189675, -3.623778108051270319, -323.0428371773161871 ) ) ;
#25942 = DIRECTION ( 'NONE',  ( -0.000000000000000000, -0.000000000000000000, 1.000000000000000000 ) ) ;
#25943 = LINE ( 'NONE', #43954, #40269 ) ;
#25944 = CARTESIAN_POINT ( 'NONE',  ( 804.6798772138708955, -399.7255117493283478, 334.6312213355107019 ) ) ;
#25945 = ORIENTED_EDGE ( 'NONE', *, *, #36798, .T. ) ;
#25946 = CARTESIAN_POINT ( 'NONE',  ( 804.1601925771018387, -343.4419599262320162, -346.5483106153029098 ) ) ;
#25947 = CARTESIAN_POINT ( 'NONE',  ( 764.8639956371174549, -152.0891481129655460, 319.7806653035542013 ) ) ;
#25948 = CARTESIAN_POINT ( 'NONE',  ( 768.8385539511368734, -335.2601417444137724, -306.4236121716840557 ) ) ;
#25949 = PLANE ( 'NONE',  #2766 ) ;
#25950 = CARTESIAN_POINT ( 'NONE',  ( 810.1134526219336749, -440.5328690171407970, 357.8822607201570349 ) ) ;
#25951 = ORIENTED_EDGE ( 'NONE', *, *, #27454, .F. ) ;
#25952 = CARTESIAN_POINT ( 'NONE',  ( 781.7834795799800531, -346.8164208402376971, 315.0636971347436202 ) ) ;
#25953 = CARTESIAN_POINT ( 'NONE',  ( 794.1144889064781864, -82.16923265350558836, -360.9840315886528401 ) ) ;
#25954 = VERTEX_POINT ( 'NONE', #30407 ) ;
#25955 = CARTESIAN_POINT ( 'NONE',  ( 756.3353852180819104, -437.9073299311463074, 331.1735550268788302 ) ) ;
#25956 = CARTESIAN_POINT ( 'NONE',  ( 810.7187646348534145, -186.4527844766017779, -356.7737145352016341 ) ) ;
#25957 = ORIENTED_EDGE ( 'NONE', *, *, #25787, .F. ) ;
#25958 = VECTOR ( 'NONE', #28788, 1000.000000000000000 ) ;
#25959 = CARTESIAN_POINT ( 'NONE',  ( 759.7806653035535192, -174.9982390220563673, -324.8639956371181370 ) ) ;
#25960 = ORIENTED_EDGE ( 'NONE', *, *, #13763, .F. ) ;
#25961 = CARTESIAN_POINT ( 'NONE',  ( 804.1105419155481968, -435.8272453906066062, -347.6308680596136469 ) ) ;
#25962 = CARTESIAN_POINT ( 'NONE',  ( 799.2566176426618085, -456.0090635724247932, 324.0069404352559559 ) ) ;
#25963 = CARTESIAN_POINT ( 'NONE',  ( 758.8095938919642549, -224.0891481129653187, 311.6929314249763365 ) ) ;
#25964 = CARTESIAN_POINT ( 'NONE',  ( 759.2295555964440155, -160.1692326535053326, 353.9708237608231229 ) ) ;
#25966 = CARTESIAN_POINT ( 'NONE',  ( 939.9999999999993179, -590.0000000000001137, -360.0000000000000000 ) ) ;
#25965 = DIRECTION ( 'NONE',  ( 0.000000000000000000, 1.000000000000000000, -0.000000000000000000 ) ) ;
#25967 = ORIENTED_EDGE ( 'NONE', *, *, #26932, .F. ) ;
#25968 = CARTESIAN_POINT ( 'NONE',  ( 757.4527132478984868, -424.3726999360612808, -329.1273215169538844 ) ) ;
#25969 = CARTESIAN_POINT ( 'NONE',  ( 794.9999999999993179, -365.3551492539851893, -28.13243251470704109 ) ) ;
#25970 = CARTESIAN_POINT ( 'NONE',  ( 809.0717654672305343, -220.9181544815164102, -360.1688906516309885 ) ) ;
#25971 = CARTESIAN_POINT ( 'NONE',  ( 793.5525998758768083, -79.09997266333503774, 372.6845335610516941 ) ) ;
#25973 = CARTESIAN_POINT ( 'NONE',  ( 199.6009925648704098, 290.0000000000001137, -244.9999999999999716 ) ) ;
#25972 = LINE ( 'NONE', #16270, #42573 ) ;
#25974 = CARTESIAN_POINT ( 'NONE',  ( 800.7704444035546203, -316.1692326535048210, -326.0291762391768771 ) ) ;
#25975 = DIRECTION ( 'NONE',  ( 0.000000000000000000, 0.000000000000000000, 1.000000000000000000 ) ) ;
#25976 = CARTESIAN_POINT ( 'NONE',  ( 814.2805881961230625, -217.6454272087891582, -331.2368401574024119 ) ) ;
#25977 = DIRECTION ( 'NONE',  ( -1.000000000000000000, 0.000000000000000000, 0.000000000000000000 ) ) ;
#25978 = CARTESIAN_POINT ( 'NONE',  ( 998.9999999999992042, 249.9999999999998863, 360.0000000000000000 ) ) ;
#25979 = CARTESIAN_POINT ( 'NONE',  ( 780.5236548040995785, -404.7363362996975980, 314.9735926884559944 ) ) ;
#25980 = VECTOR ( 'NONE', #25818, 1000.000000000000000 ) ;
#25981 = CARTESIAN_POINT ( 'NONE',  ( 746.8695393053151292, -245.9073299311469896, -327.6429770376306578 ) ) ;
#25982 = CARTESIAN_POINT ( 'NONE',  ( 769.9999999999992042, 240.0000000000000853, -360.0000000000000000 ) ) ;
#25983 = CARTESIAN_POINT ( 'NONE',  ( 757.8323909638827445, -26.63460265842045871, -352.1044303154654358 ) ) ;
#25984 = CARTESIAN_POINT ( 'NONE',  ( 799.9636004259356241, -190.9181544815164955, 311.2241431872006956 ) ) ;
#25985 = CARTESIAN_POINT ( 'NONE',  ( 812.6845335610512393, -127.9874144716872308, -353.5525998758768651 ) ) ;
#25986 = CARTESIAN_POINT ( 'NONE',  ( 813.1304606946830518, -161.9073299311472454, 352.3570229623690580 ) ) ;
#25987 = CARTESIAN_POINT ( 'NONE',  ( 751.6929314249748586, -366.9982390220556567, -318.8095938919659034 ) ) ;
#25988 = CARTESIAN_POINT ( 'NONE',  ( -338.8365100919713200, 260.0000000000001137, -193.8809999999918148 ) ) ;
#25989 = CARTESIAN_POINT ( 'NONE',  ( 521.6730038022808458, 239.9999999999999432, 350.0000000000000000 ) ) ;
#25990 = CARTESIAN_POINT ( 'NONE',  ( 791.9812246680005501, -212.6346026584198796, 361.9419747391813189 ) ) ;
#25991 = CARTESIAN_POINT ( 'NONE',  ( 766.9102291470427417, -18.55451811788065797, 318.6633372737382501 ) ) ;
#25992 = CARTESIAN_POINT ( 'NONE',  ( 755.3201227861273992, -387.7255117493283478, -345.3687786644892981 ) ) ;
#25993 = CARTESIAN_POINT ( 'NONE',  ( 812.3518521366052028, -1.099972663335260226, -326.5853460496235243 ) ) ;
#25994 = DIRECTION ( 'NONE',  ( -1.000000000000000000, -0.000000000000000000, -0.000000000000000000 ) ) ;
#25995 = CARTESIAN_POINT ( 'NONE',  ( 768.8385539511368734, -23.26014174441484883, 306.4236121716840557 ) ) ;
#25996 = EDGE_LOOP ( 'NONE', ( #44409, #25534, #28980, #44363 ) ) ;
#25997 = CARTESIAN_POINT ( 'NONE',  ( 757.2208543904082489, -232.7146871989596377, -350.9844846989624330 ) ) ;
#25998 = CARTESIAN_POINT ( 'NONE',  ( 794.9819416627830151, -36.99823902205679360, 319.9864689768909898 ) ) ;
#25999 = CARTESIAN_POINT ( 'NONE',  ( 744.8212110874229666, -210.8965053807778816, -336.2046728542121627 ) ) ;
#26000 = FILL_AREA_STYLE ('',( #25572 ) ) ;
#26001 = CARTESIAN_POINT ( 'NONE',  ( 776.2433038121456548, -348.8965053807774552, 374.8207195650711014 ) ) ;
#26002 = ORIENTED_EDGE ( 'NONE', *, *, #43103, .F. ) ;
#26003 = CARTESIAN_POINT ( 'NONE',  ( 795.6651683502461765, -418.7146871989590409, 371.3240766477733814 ) ) ;
#26004 = CARTESIAN_POINT ( 'NONE',  ( 804.4286716492782716, -137.3618753856928265, -345.3141322388244703 ) ) ;
#26005 = CARTESIAN_POINT ( 'NONE',  ( 771.2633955100217236, -335.9073299311468190, 363.4237431249939618 ) ) ;
#26006 = CARTESIAN_POINT ( 'NONE',  ( 747.2067596250078623, -75.18005720387485269, -352.2312462859687230 ) ) ;
#26007 = AXIS2_PLACEMENT_3D ( 'NONE', #38491, #378, #3397 ) ;
#26008 = CARTESIAN_POINT ( 'NONE',  ( 778.2165204200184689, -70.81642084023850714, -364.9363028652563230 ) ) ;
#26009 = EDGE_LOOP ( 'NONE', ( #36547, #26126 ) ) ;
#26010 = CARTESIAN_POINT ( 'NONE',  ( 769.0155153010367712, -10.37269993606250473, -362.7791456095907279 ) ) ;
#26011 = ORIENTED_EDGE ( 'NONE', *, *, #27506, .F. ) ;
#26012 = CARTESIAN_POINT ( 'NONE',  ( 754.7162404726377645, -326.7363362996979390, -339.4709603349214717 ) ) ;
#26014 = CARTESIAN_POINT ( 'NONE',  ( 783.0745993439762742, -368.1908817542433212, 365.1016975059196739 ) ) ;
#26013 = CARTESIAN_POINT ( 'NONE',  ( 800.2193346964447755, -42.99823902205675807, 355.1360043628815788 ) ) ;
#26015 = CARTESIAN_POINT ( 'NONE',  ( 785.3141322388236176, -333.7255117493286320, -364.4286716492789537 ) ) ;
#26018 = CARTESIAN_POINT ( 'NONE',  ( 776.2433038121456548, -324.8965053807775121, 374.8207195650711014 ) ) ;
#26017 = FACE_OUTER_BOUND ( 'NONE', #10357, .T. ) ;
#26016 = CARTESIAN_POINT ( 'NONE',  ( 782.4968714119720516, -418.8164208402374129, 305.0891759886411023 ) ) ;
#26019 = CARTESIAN_POINT ( 'NONE',  ( 746.0683387631852383, -91.44195992623282621, 331.3260364891676204 ) ) ;
#26020 = CARTESIAN_POINT ( 'NONE',  ( 790.9844846989617508, -334.3726999360615082, -317.2208543904092721 ) ) ;
#26021 = CARTESIAN_POINT ( 'NONE',  ( 800.2193346964447755, -282.9982390220558841, -355.1360043628815788 ) ) ;
#26022 = PLANE ( 'NONE',  #36130 ) ;
#26023 = CARTESIAN_POINT ( 'NONE',  ( 803.6646147819161570, -137.9073299311473875, -348.8264449731210561 ) ) ;
#26024 = CARTESIAN_POINT ( 'NONE',  ( 829.9999999999992042, 290.0000000000001137, -244.9999999999999716 ) ) ;
#26025 = CARTESIAN_POINT ( 'NONE',  ( 772.4837098697144029, -431.3618753856918033, 374.5518280994205611 ) ) ;
#26027 = LINE ( 'NONE', #21667, #13050 ) ;
#26026 = DIRECTION ( 'NONE',  ( 0.000000000000000000, 0.000000000000000000, 1.000000000000000000 ) ) ;
#26028 = CARTESIAN_POINT ( 'NONE',  ( 814.4686193811664907, -75.28179084515321051, -346.2056067578752732 ) ) ;
#26029 = DIRECTION ( 'NONE',  ( -1.000000000000000000, -0.000000000000000000, -0.000000000000000000 ) ) ;
#26030 = CARTESIAN_POINT ( 'NONE',  ( -208.8365100919714052, 260.0000000000001137, -199.9999999999926956 ) ) ;
#26031 = ADVANCED_FACE ( 'NONE', ( #40810 ), #5245, .F. ) ;
#26032 = CARTESIAN_POINT ( 'NONE',  ( 759.0159684113467620, -304.9181544815161828, 325.8855110935213020 ) ) ;
#26033 = CARTESIAN_POINT ( 'NONE',  ( 762.3223304703356007, -175.5436935675108998, 322.3223304703362828 ) ) ;
#26034 = ORIENTED_EDGE ( 'NONE', *, *, #13086, .T. ) ;
#26035 = CARTESIAN_POINT ( 'NONE',  ( 815.2698199232962679, -136.8164208402382656, -342.5225473063383674 ) ) ;
#26036 = CARTESIAN_POINT ( 'NONE',  ( 773.3843516231979720, -325.4419599262320162, 364.4086373105754433 ) ) ;
#26037 = CARTESIAN_POINT ( 'NONE',  ( 795.8262568251477660, -70.37269993606230400, 308.3538107759623585 ) ) ;
#26038 = CARTESIAN_POINT ( 'NONE',  ( 811.0346526505616112, -278.6346026584196807, -323.0537975583477532 ) ) ;
#26039 = EDGE_CURVE ( 'NONE', #39585, #17206, #8941, .T. ) ;
#26040 = CARTESIAN_POINT ( 'NONE',  ( 792.1044303154645831, -132.4527844766018916, 317.8323909638837677 ) ) ;
#26041 = VECTOR ( 'NONE', #10582, 1000.000000000000000 ) ;
#26042 = VERTEX_POINT ( 'NONE', #30647 ) ;
#26043 = CARTESIAN_POINT ( 'NONE',  ( 768.8385539511368734, -359.2601417444137724, -306.4236121716840557 ) ) ;
#26044 = AXIS2_PLACEMENT_3D ( 'NONE', #8820, #2556, #44605 ) ;
#26045 = CARTESIAN_POINT ( 'NONE',  ( 777.4774526936600978, -106.2709662947838467, -304.7301800767027657 ) ) ;
#26046 = CARTESIAN_POINT ( 'NONE',  ( 766.0291762391763086, -10.91815448151704793, 360.7704444035551319 ) ) ;
#26047 = CARTESIAN_POINT ( 'NONE',  ( 747.2067596250078623, -339.1800572038740142, -352.2312462859687230 ) ) ;
#26048 = CARTESIAN_POINT ( 'NONE',  ( 879.9999999999992042, 259.9999999999998863, -219.9999999999999716 ) ) ;
#26049 = CARTESIAN_POINT ( 'NONE',  ( 786.6156483768007774, -385.4419599262319593, 315.5913626894246136 ) ) ;
#26050 = EDGE_LOOP ( 'NONE', ( #9382, #11848 ) ) ;
#26051 = CARTESIAN_POINT ( 'NONE',  ( 766.7756240680305382, -86.53286901714194812, 361.5560724626415663 ) ) ;
#26052 = CARTESIAN_POINT ( 'NONE',  ( 774.6312213355099630, -431.3618753856918033, -364.6798772138717482 ) ) ;
#26053 = CARTESIAN_POINT ( 'NONE',  ( 764.8639956371174549, -224.0891481129653187, -319.7806653035542013 ) ) ;
#26054 = CARTESIAN_POINT ( 'NONE',  ( 746.0683387631852383, -115.4419599262327409, -331.3260364891676204 ) ) ;
#26055 = DIRECTION ( 'NONE',  ( -0.000000000000000000, 1.000000000000000000, -0.000000000000000000 ) ) ;
#26056 = CARTESIAN_POINT ( 'NONE',  ( 766.5853460496234675, -253.9874144716868329, 372.3518521366060554 ) ) ;
#26057 = CARTESIAN_POINT ( 'NONE',  ( 802.1676090361155502, -62.63460265842032726, 327.8955696845344505 ) ) ;
#26058 = EDGE_CURVE ( 'NONE', #10523, #17262, #44783, .T. ) ;
#26059 = CARTESIAN_POINT ( 'NONE',  ( 805.0264073115434940, -246.3510508353232638, -339.4763451958999099 ) ) ;
#26060 = CARTESIAN_POINT ( 'NONE',  ( 778.2165204200184689, -238.8164208402379813, 364.9363028652563230 ) ) ;
#26061 = CARTESIAN_POINT ( 'NONE',  ( 805.9055244015594326, -435.6237781080499190, -315.8990559732753240 ) ) ;
#26062 = CARTESIAN_POINT ( 'NONE',  ( 773.7943932421234194, -71.80559628986922860, -305.5313806188329409 ) ) ;
#26063 = DIRECTION ( 'NONE',  ( 0.000000000000000000, 0.000000000000000000, 1.000000000000000000 ) ) ;
#26064 = EDGE_LOOP ( 'NONE', ( #29767, #35351 ) ) ;
#26065 = VERTEX_POINT ( 'NONE', #23011 ) ;
#26066 = CARTESIAN_POINT ( 'NONE',  ( 811.3240766477731540, -388.3726999360613945, -355.6651683502462902 ) ) ;
#26067 = CARTESIAN_POINT ( 'NONE',  ( 808.0189434323515343, -278.0891481129651197, 319.0252816721025511 ) ) ;
#26068 = CARTESIAN_POINT ( 'NONE',  ( 788.7631598425961101, -25.44195992623301450, 305.7194118038759143 ) ) ;
#26069 = CARTESIAN_POINT ( 'NONE',  ( 783.0745993439762742, -176.1908817542438328, -365.1016975059196739 ) ) ;
#26070 = CARTESIAN_POINT ( 'NONE',  ( 759.9864689768902508, -170.0891481129654608, -354.9819416627836404 ) ) ;
#26071 = CIRCLE ( 'NONE', #9866, 9.999999999999980460 ) ;
#26072 = CARTESIAN_POINT ( 'NONE',  ( 804.6798772138710092, -399.7255117493283478, -334.6312213355106451 ) ) ;
#26073 = ORIENTED_EDGE ( 'NONE', *, *, #10732, .T. ) ;
#26074 = CARTESIAN_POINT ( 'NONE',  ( 764.8639956371174549, -224.0891481129653187, 319.7806653035542013 ) ) ;
#26075 = AXIS2_PLACEMENT_3D ( 'NONE', #36942, #26543, #23062 ) ;
#26076 = CARTESIAN_POINT ( 'NONE',  ( 780.5290396650775619, 11.64894916467595642, -365.2837595273619513 ) ) ;
#26077 = ORIENTED_EDGE ( 'NONE', *, *, #7473, .F. ) ;
#26078 = CARTESIAN_POINT ( 'NONE',  ( 804.7487373415286811, -331.5436935675104451, 364.7487373415288516 ) ) ;
#26079 = EDGE_CURVE ( 'NONE', #10694, #40245, #7167, .T. ) ;
#26080 = PLANE ( 'NONE',  #3430 ) ;
#26081 = CARTESIAN_POINT ( 'NONE',  ( 765.8855110935204493, -358.1692326535047641, 319.0159684113471599 ) ) ;
#26082 = DIRECTION ( 'NONE',  ( 0.000000000000000000, -1.000000000000000000, 0.000000000000000000 ) ) ;
#26083 = CYLINDRICAL_SURFACE ( 'NONE', #9105, 6.119000000000013095 ) ;
#26084 = EDGE_CURVE ( 'NONE', #6776, #36186, #11586, .T. ) ;
#26085 = CARTESIAN_POINT ( 'NONE',  ( 793.0897708529556667, -198.5545181178800647, 361.3366627262616362 ) ) ;
#26086 = CARTESIAN_POINT ( 'NONE',  ( 804.4286716492782716, -65.36187538569306810, 345.3141322388244703 ) ) ;
#26087 = ORIENTED_EDGE ( 'NONE', *, *, #11778, .F. ) ;
#26088 = CARTESIAN_POINT ( 'NONE',  ( 781.2370466360911223, -404.7363362996975980, -304.9990715423533629 ) ) ;
#26089 = CARTESIAN_POINT ( 'NONE',  ( 772.5602148656447525, -33.72551174932952733, -305.7998596910095443 ) ) ;
#26090 = CARTESIAN_POINT ( 'NONE',  ( 804.9511171171677688, -221.8055962898687881, 335.8780910478229202 ) ) ;
#26091 = CARTESIAN_POINT ( 'NONE',  ( 800.2193346964447755, -402.9982390220555430, -355.1360043628815788 ) ) ;
#26092 = CARTESIAN_POINT ( 'NONE',  ( 765.0180583372156207, -0.9982390220569063999, -360.0135310231089534 ) ) ;
#26093 = AXIS2_PLACEMENT_3D ( 'NONE', #9794, #6783, #20637 ) ;
#26094 = CARTESIAN_POINT ( 'NONE',  ( 772.4837098697144029, -431.3618753856918033, 374.5518280994205611 ) ) ;
#26095 = DIRECTION ( 'NONE',  ( -0.000000000000000000, 1.000000000000000000, -0.000000000000000000 ) ) ;
#26096 = CARTESIAN_POINT ( 'NONE',  ( 761.4292242960306112, -257.4636090269708575, -323.2154366446414429 ) ) ;
#26097 = ADVANCED_FACE ( 'NONE', ( #8733 ), #38890, .F. ) ;
#26098 = CARTESIAN_POINT ( 'NONE',  ( 787.4397851343537695, -165.7255117493291152, -374.2001403089903988 ) ) ;
#26099 = EDGE_CURVE ( 'NONE', #14626, #18157, #31826, .T. ) ;
#26100 = CARTESIAN_POINT ( 'NONE',  ( 763.0537975583475827, -48.45278447660219712, 371.0346526505627480 ) ) ;
#26101 = CARTESIAN_POINT ( 'NONE',  ( 751.9810565676468741, -122.0891481129656171, 360.9747183278973921 ) ) ;
#26102 = CARTESIAN_POINT ( 'NONE',  ( 790.2803779376845341, 16.45630643248849623, -314.3272116953297086 ) ) ;
#26103 = CARTESIAN_POINT ( 'NONE',  ( -37.63011601220122770, -563.3203001761231690, -342.3463313526983143 ) ) ;
#26104 = CARTESIAN_POINT ( 'NONE',  ( 749.5768839229115201, -396.5545181178794678, 358.0661480581553064 ) ) ;
#26105 = CARTESIAN_POINT ( 'NONE',  ( 311.1634899080286232, 260.0000000000000000, -208.0249999999963109 ) ) ;
#26106 = CARTESIAN_POINT ( 'NONE',  ( 755.2512626584698410, -367.5436935675102745, 315.2512626584710915 ) ) ;
#26107 = CARTESIAN_POINT ( 'NONE',  ( 785.3687786644884454, -323.3618753856923149, -315.3201227861279676 ) ) ;
#26108 = CARTESIAN_POINT ( 'NONE',  ( 780.5290396650775619, 11.64894916467595642, 365.2837595273619513 ) ) ;
#26109 = CIRCLE ( 'NONE', #4006, 20.00000000000001776 ) ;
#26110 = AXIS2_PLACEMENT_3D ( 'NONE', #13054, #9120, #8899 ) ;
#26111 = CARTESIAN_POINT ( 'NONE',  ( 745.5313806188320314, -111.2817908451530968, -333.7943932421247268 ) ) ;
#26112 = CARTESIAN_POINT ( 'NONE',  ( 787.6308680596127942, -107.2601417444145824, -364.1105419155492768 ) ) ;
#26113 = ADVANCED_FACE ( 'NONE', ( #19124 ), #33212, .T. ) ;
#26114 = CARTESIAN_POINT ( 'NONE',  ( 754.0944755984390895, -135.6237781080508853, 364.1009440267246760 ) ) ;
#26115 = CARTESIAN_POINT ( 'NONE',  ( 804.9363028652555840, -424.2709662947829088, 338.2165204200192079 ) ) ;
#26116 = EDGE_CURVE ( 'NONE', #28819, #1155, #36892, .T. ) ;
#26117 = CARTESIAN_POINT ( 'NONE',  ( 747.3154664389472828, -163.9874144716871456, 326.4474001241230781 ) ) ;
#26118 = CARTESIAN_POINT ( 'NONE',  ( 804.6798772138708955, -15.72551174932958951, -334.6312213355107019 ) ) ;
#26119 = CARTESIAN_POINT ( 'NONE',  ( 766.7756240680305382, -134.5328690171417350, -361.5560724626415663 ) ) ;
#26120 = CARTESIAN_POINT ( 'NONE',  ( 755.3201227861273992, -123.7255117493292147, -345.3687786644892981 ) ) ;
#26121 = CARTESIAN_POINT ( 'NONE',  ( 792.1044303154645831, -132.4527844766018916, 317.8323909638837677 ) ) ;
#26122 = CARTESIAN_POINT ( 'NONE',  ( 796.7845633553578182, -441.6237781080499190, -358.5707757039688204 ) ) ;
#26124 = CARTESIAN_POINT ( 'NONE',  ( 756.3353852180820240, -269.9073299311469327, 331.1735550268787733 ) ) ;
#26123 = CARTESIAN_POINT ( 'NONE',  ( 767.8955696845333705, -264.4527844766016074, 362.1676090361162323 ) ) ;
#26125 = FACE_OUTER_BOUND ( 'NONE', #21038, .T. ) ;
#26126 = ORIENTED_EDGE ( 'NONE', *, *, #26058, .F. ) ;
#26127 = CARTESIAN_POINT ( 'NONE',  ( 801.3366627262608972, 15.46713098285775878, 353.0897708529566899 ) ) ;
#26128 = CARTESIAN_POINT ( 'NONE',  ( 807.2620300519052989, -264.0090635724253616, -318.0141637701419768 ) ) ;
#26129 = CIRCLE ( 'NONE', #41634, 2.749999999999863665 ) ;
#26130 = ORIENTED_EDGE ( 'NONE', *, *, #14615, .T. ) ;
#26131 = CARTESIAN_POINT ( 'NONE',  ( 0.000000000000000000, 0.000000000000000000, 0.000000000000000000 ) ) ;
#26132 = CIRCLE ( 'NONE', #13617, 30.00000000000008171 ) ;
#26133 = CARTESIAN_POINT ( 'NONE',  ( 777.4774526936600978, -202.2709662947835341, 304.7301800767028226 ) ) ;
#26134 = CARTESIAN_POINT ( 'NONE',  ( 796.9571628226829034, -287.4636090269708575, 321.2382568024804641 ) ) ;
#26135 = CARTESIAN_POINT ( 'NONE',  ( 756.1348686366196716, -401.2601417444137155, 347.5531968255698416 ) ) ;
#26136 = ORIENTED_EDGE ( 'NONE', *, *, #15654, .F. ) ;
#26137 = CARTESIAN_POINT ( 'NONE',  ( 759.0159684113467620, -64.91815448151686496, -325.8855110935213020 ) ) ;
#26138 = CARTESIAN_POINT ( 'NONE',  ( 771.1735550268780344, -273.1800572038742985, -316.3353852180828198 ) ) ;
#26139 = VERTEX_POINT ( 'NONE', #19558 ) ;
#26140 = CARTESIAN_POINT ( 'NONE',  ( 778.2165204200184689, -406.8164208402375266, -364.9363028652563230 ) ) ;
#26141 = CARTESIAN_POINT ( 'NONE',  ( 755.5713283507202505, -53.36187538569310362, -334.6858677611754729 ) ) ;
#26142 = EDGE_CURVE ( 'NONE', #32851, #42899, #43805, .T. ) ;
#26143 = ADVANCED_FACE ( 'NONE', ( #12413 ), #40594, .F. ) ;
#26144 = CARTESIAN_POINT ( 'NONE',  ( 755.8398074228967971, -259.4419599262322436, 333.4516893846970333 ) ) ;
#26145 = CARTESIAN_POINT ( 'NONE',  ( 879.9999999999990905, 479.9999999999998863, 199.9999999999999716 ) ) ;
#26146 = DIRECTION ( 'NONE',  ( -0.7014439490181308967, 0.1263042864341425708, 0.7014439490181749726 ) ) ;
#26147 = EDGE_CURVE ( 'NONE', #20728, #41166, #30185, .T. ) ;
#26148 = CARTESIAN_POINT ( 'NONE',  ( 791.0478386215596629, -21.82724539060792424, -306.7653713866226326 ) ) ;
#26149 = CARTESIAN_POINT ( 'NONE',  ( 911.9749999999993406, 154.9999999999998863, -360.0000000000000000 ) ) ;
#26150 = ORIENTED_EDGE ( 'NONE', *, *, #28627, .F. ) ;
#26151 = CARTESIAN_POINT ( 'NONE',  ( 760.0363995740630116, -298.9181544815161828, -368.7758568127991907 ) ) ;
#26152 = VECTOR ( 'NONE', #39085, 1000.000000000000000 ) ;
#26153 = CARTESIAN_POINT ( 'NONE',  ( 762.1177392798416577, -162.5545181178802352, 309.8865473780659272 ) ) ;
#26154 = CIRCLE ( 'NONE', #10049, 10.00000000000006395 ) ;
#26156 = CARTESIAN_POINT ( 'NONE',  ( 785.3687786644884454, -275.3618753856923149, -315.3201227861279676 ) ) ;
#26155 = DIRECTION ( 'NONE',  ( 0.000000000000000000, 0.000000000000000000, 1.000000000000000000 ) ) ;
#26157 = CARTESIAN_POINT ( 'NONE',  ( 998.9999999999992042, 479.9999999999999432, -199.9999999999999716 ) ) ;
#26158 = CARTESIAN_POINT ( 'NONE',  ( 776.9254006560222479, -164.1908817542438612, -314.8983024940802125 ) ) ;
#26159 = EDGE_CURVE ( 'NONE', #15686, #8608, #16325, .T. ) ;
#26160 = DIRECTION ( 'NONE',  ( -1.000000000000000000, -4.625929269271485914E-16, 0.000000000000000000 ) ) ;
#26161 = CARTESIAN_POINT ( 'NONE',  ( 748.3538107759620743, -16.71468719896031985, -355.8262568251490165 ) ) ;
#26163 = CIRCLE ( 'NONE', #35797, 30.00000000000008171 ) ;
#26162 = CARTESIAN_POINT ( 'NONE',  ( 777.4774526936600978, -346.2709662947830225, -304.7301800767028226 ) ) ;
#26164 = DIRECTION ( 'NONE',  ( 1.000000000000000000, 0.000000000000000000, 0.000000000000000000 ) ) ;
#26165 = CARTESIAN_POINT ( 'NONE',  ( 758.0580252608178853, -30.45278447660226817, 328.0187753319985404 ) ) ;
#26166 = VECTOR ( 'NONE', #45212, 1000.000000000000000 ) ;
#26167 = CARTESIAN_POINT ( 'NONE',  ( 805.6418435158337843, -293.4636090269707438, 363.8556311672236916 ) ) ;
#26168 = CARTESIAN_POINT ( 'NONE',  ( 751.6929314249748586, -270.9982390220561115, 318.8095938919659034 ) ) ;
#26169 = CARTESIAN_POINT ( 'NONE',  ( 792.2312462859673587, 12.09267006885214180, -307.2067596250082602 ) ) ;
#26170 = DIRECTION ( 'NONE',  ( 1.000000000000000000, 0.000000000000000000, 0.000000000000000000 ) ) ;
#26171 = VECTOR ( 'NONE', #6119, 1000.000000000000000 ) ;
#26172 = EDGE_LOOP ( 'NONE', ( #34678, #14684, #40176, #9663 ) ) ;
#26173 = CARTESIAN_POINT ( 'NONE',  ( 764.8639956371174549, -368.0891481129647786, 319.7806653035542013 ) ) ;
#26174 = CARTESIAN_POINT ( 'NONE',  ( 755.5913626894240451, -133.6454272087893571, 346.6156483768012890 ) ) ;
#26175 = CARTESIAN_POINT ( 'NONE',  ( 770.0799878456142551, -13.98741447168760033, -362.9823548866085616 ) ) ;
#26176 = CARTESIAN_POINT ( 'NONE',  ( 949.5497976682736407, 239.9999999999998863, -209.9999999999999716 ) ) ;
#26177 = DIRECTION ( 'NONE',  ( 1.000000000000000000, 0.000000000000000000, 0.000000000000000000 ) ) ;
#26178 = CARTESIAN_POINT ( 'NONE',  ( 803.4237431249931660, -399.1800572038738437, 331.2633955100225194 ) ) ;
#26179 = EDGE_LOOP ( 'NONE', ( #42099, #32972, #29501, #20051, #17966, #11563 ) ) ;
#26180 = CARTESIAN_POINT ( 'NONE',  ( 795.1360043628807261, -44.08914811296584446, -360.2193346964456282 ) ) ;
#26181 = AXIS2_PLACEMENT_3D ( 'NONE', #24980, #25673, #21983 ) ;
#26182 = CARTESIAN_POINT ( 'NONE',  ( 789.9200121543843807, -313.9874144716866908, -317.0176451133914384 ) ) ;
#26183 = CARTESIAN_POINT ( 'NONE',  ( 756.5762568750052424, -147.1800572038746395, 348.7366044899774238 ) ) ;
#26184 = AXIS2_PLACEMENT_3D ( 'NONE', #5779, #19865, #10606 ) ;
#26185 = CARTESIAN_POINT ( 'NONE',  ( 778.7502325331095108, -312.3510508353230080, -304.6391490659818828 ) ) ;
#26186 = CARTESIAN_POINT ( 'NONE',  ( 989.9999999999992042, 249.9999999999998863, 350.0000000000000000 ) ) ;
#26187 = ORIENTED_EDGE ( 'NONE', *, *, #402, .F. ) ;
#26188 = CARTESIAN_POINT ( 'NONE',  ( 759.7806653035534055, -366.9982390220556567, 324.8639956371180801 ) ) ;
#26189 = AXIS2_PLACEMENT_3D ( 'NONE', #42540, #4208, #15286 ) ;
#26190 = VERTEX_POINT ( 'NONE', #34783 ) ;
#26191 = CARTESIAN_POINT ( 'NONE',  ( 767.8955696845333705, -432.4527844766008684, 362.1676090361162323 ) ) ;
#26192 = CARTESIAN_POINT ( 'NONE',  ( 814.5518280994195948, -183.7255117493290015, -332.4837098697145734 ) ) ;
#26193 = CARTESIAN_POINT ( 'NONE',  ( 792.3570229623691148, -69.18005720387488111, 373.1304606946836770 ) ) ;
#26194 = ORIENTED_EDGE ( 'NONE', *, *, #11632, .F. ) ;
#26195 = AXIS2_PLACEMENT_3D ( 'NONE', #21177, #3635, #17722 ) ;
#26196 = CARTESIAN_POINT ( 'NONE',  ( 755.3201227861273992, -171.7255117493290868, -345.3687786644892981 ) ) ;
#26197 = ORIENTED_EDGE ( 'NONE', *, *, #36847, .F. ) ;
#26198 = CARTESIAN_POINT ( 'NONE',  ( 783.0745993439762742, -440.1908817542430370, -365.1016975059196739 ) ) ;
#26199 = VECTOR ( 'NONE', #43557, 1000.000000000000000 ) ;
#26200 = CARTESIAN_POINT ( 'NONE',  ( 801.9419747391806368, 5.547215523397618142, 351.9812246680014027 ) ) ;
#26201 = CARTESIAN_POINT ( 'NONE',  ( 744.7301800767019131, -220.8164208402379529, 337.4774526936615757 ) ) ;
#26202 = CARTESIAN_POINT ( 'NONE',  ( 784.0799538623451781, -155.8055962898689586, 364.6971507214555572 ) ) ;
#26204 = CARTESIAN_POINT ( 'NONE',  ( 799.9999999999993179, -373.0259173205825505, 36.60293108048681887 ) ) ;
#26203 = DIRECTION ( 'NONE',  ( 0.000000000000000000, -0.000000000000000000, -1.000000000000000000 ) ) ;
#26205 = VECTOR ( 'NONE', #25942, 1000.000000000000000 ) ;
#26206 = ORIENTED_EDGE ( 'NONE', *, *, #27246, .F. ) ;
#26207 = CARTESIAN_POINT ( 'NONE',  ( 763.8424801807145741, -426.0090635724247932, -320.5453621957614700 ) ) ;
#26208 = DIRECTION ( 'NONE',  ( -0.000000000000000000, -0.6438296778008192334, -0.7651688349527135946 ) ) ;
#26209 = CARTESIAN_POINT ( 'NONE',  ( 752.7379699480933368, -204.0090635724255606, -361.9858362298580232 ) ) ;
#26210 = CARTESIAN_POINT ( 'NONE',  ( 797.8822607201568644, -54.55451811788054783, 370.1134526219340160 ) ) ;
#26212 = CARTESIAN_POINT ( 'NONE',  ( 754.8072714833581358, -172.8164208402381234, -338.1981804954720587 ) ) ;
#26211 = DIRECTION ( 'NONE',  ( -1.000000000000000000, -0.000000000000000000, -0.000000000000000000 ) ) ;
#26213 = CARTESIAN_POINT ( 'NONE',  ( 761.2382568024794409, -327.6237781080502600, -356.9571628226838129 ) ) ;
#26214 = PLANE ( 'NONE',  #37988 ) ;
#26215 = CARTESIAN_POINT ( 'NONE',  ( 752.7379699480933368, -228.0090635724254753, -361.9858362298580232 ) ) ;
#26216 = DIRECTION ( 'NONE',  ( 1.000000000000000000, 0.000000000000000000, -0.000000000000000000 ) ) ;
#26217 = DIRECTION ( 'NONE',  ( 8.326672684688676025E-16, -1.000000000000000000, 0.000000000000000000 ) ) ;
#26218 = CARTESIAN_POINT ( 'NONE',  ( 779.4763451958990572, -56.73633629969872771, -365.0264073115438919 ) ) ;
#26219 = CARTESIAN_POINT ( 'NONE',  ( 798.5707757039680246, -413.4636090269704027, 356.7845633553585003 ) ) ;
#26220 = AXIS2_PLACEMENT_3D ( 'NONE', #4154, #42482, #39493 ) ;
#26221 = CARTESIAN_POINT ( 'NONE',  ( 782.4968714119720516, -250.8164208402379245, -305.0891759886411023 ) ) ;
#26222 = CARTESIAN_POINT ( 'NONE',  ( 787.5531968255692163, -237.8272453906072599, 316.1348686366205811 ) ) ;
#26223 = CARTESIAN_POINT ( 'NONE',  ( 311.1634899080286232, 240.0000000000000000, -202.7499999999961915 ) ) ;
#26224 = CARTESIAN_POINT ( 'NONE',  ( 788.8264449731200330, 2.819942796124898177, -363.6646147819171233 ) ) ;
#26225 = VECTOR ( 'NONE', #22063, 1000.000000000000000 ) ;
#26226 = CARTESIAN_POINT ( 'NONE',  ( 807.2620300519052989, -168.0090635724256458, 318.0141637701419768 ) ) ;
#26227 = CARTESIAN_POINT ( 'NONE',  ( 758.0141637701419768, -135.0783235625962959, -367.2620300519063790 ) ) ;
#26228 = CARTESIAN_POINT ( 'NONE',  ( 777.5031285880264704, -142.8164208402382656, 374.9108240113588408 ) ) ;
#26229 = CARTESIAN_POINT ( 'NONE',  ( 748.9653473494363425, -362.6346026584194533, -356.9462024416521331 ) ) ;
#26230 = VECTOR ( 'NONE', #42647, 1000.000000000000000 ) ;
#26231 = DIRECTION ( 'NONE',  ( -0.000000000000000000, 1.000000000000000000, -0.000000000000000000 ) ) ;
#26232 = DIRECTION ( 'NONE',  ( 0.000000000000000000, 0.000000000000000000, 1.000000000000000000 ) ) ;
#26233 = CARTESIAN_POINT ( 'NONE',  ( 778.2165204200184689, -238.8164208402379813, 364.9363028652563230 ) ) ;
#26234 = CARTESIAN_POINT ( 'NONE',  ( 758.4439275373578084, -12.55451811788067751, 353.2243759319684386 ) ) ;
#26235 = CARTESIAN_POINT ( 'NONE',  ( 759.7806653035534055, -390.9982390220557136, -324.8639956371180801 ) ) ;
#26236 = VECTOR ( 'NONE', #5372, 1000.000000000000000 ) ;
#26237 = DIRECTION ( 'NONE',  ( 0.000000000000000000, 0.3826834323650836200, 0.9238795325112892920 ) ) ;
#26238 = CARTESIAN_POINT ( 'NONE',  ( 804.7487373415286811, -451.5436935675099903, -364.7487373415288516 ) ) ;
#26239 = CARTESIAN_POINT ( 'NONE',  ( 441.1634899080286232, 239.9999999999999716, -197.2499999999973852 ) ) ;
#26240 = CARTESIAN_POINT ( 'NONE',  ( 780.5290396650775619, -60.35105083532383219, 365.2837595273619513 ) ) ;
#26241 = ORIENTED_EDGE ( 'NONE', *, *, #28951, .T. ) ;
#26242 = AXIS2_PLACEMENT_3D ( 'NONE', #598, #11680, #3616 ) ;
#26243 = CARTESIAN_POINT ( 'NONE',  ( 787.6308680596127942, -227.2601417444141987, -364.1105419155492768 ) ) ;
#26244 = CARTESIAN_POINT ( 'NONE',  ( 759.9864689768902508, -26.08914811296592262, 354.9819416627836404 ) ) ;
#26245 = CARTESIAN_POINT ( 'NONE',  ( 752.4576283171824116, -213.0783235625960401, -317.7880784355627952 ) ) ;
#26246 = CARTESIAN_POINT ( 'NONE',  ( -858.8365100919713768, 260.0000000000002274, -202.7499999999880345 ) ) ;
#26247 = CARTESIAN_POINT ( 'NONE',  ( 813.9316612368132837, -343.4419599262320162, 348.6739635108323228 ) ) ;
#26248 = ORIENTED_EDGE ( 'NONE', *, *, #521, .T. ) ;
#26249 = CARTESIAN_POINT ( 'NONE',  ( 771.1735550268778070, -153.1800572038746395, -316.3353852180827630 ) ) ;
#26250 = CARTESIAN_POINT ( 'NONE',  ( 795.1360043628807261, -332.0891481129649492, 360.2193346964456282 ) ) ;
#26251 = CARTESIAN_POINT ( 'NONE',  ( 812.7932403749906598, -63.18005720387488822, -327.7687537140311633 ) ) ;
#26252 = CARTESIAN_POINT ( 'NONE',  ( 755.3201227861273992, -75.72551174932938522, -345.3687786644892981 ) ) ;
#26253 = ORIENTED_EDGE ( 'NONE', *, *, #6286, .T. ) ;
#26254 = CARTESIAN_POINT ( 'NONE',  ( 757.0176451133909268, -13.09997266333522248, -349.9200121543848354 ) ) ;
#26255 = AXIS2_PLACEMENT_3D ( 'NONE', #9337, #5634, #33149 ) ;
#26256 = ORIENTED_EDGE ( 'NONE', *, *, #40134, .F. ) ;
#26257 = CARTESIAN_POINT ( 'NONE',  ( 786.5483106153019435, -319.6454272087888739, -364.1601925771022366 ) ) ;
#26259 = CARTESIAN_POINT ( 'NONE',  ( 804.4086373105744769, -361.6454272087887603, 333.3843516231986541 ) ) ;
#26258 = CARTESIAN_POINT ( 'NONE',  ( 762.1405469898971887, -73.54369356751118403, 357.8594530101015607 ) ) ;
#26260 = CONICAL_SURFACE ( 'NONE', #41663, 8.024999999999948841, 0.7853981633974337351 ) ;
#26263 = CARTESIAN_POINT ( 'NONE',  ( 788.7631598425961101, -313.4419599262320730, 305.7194118038759143 ) ) ;
#26262 = FACE_OUTER_BOUND ( 'NONE', #42893, .T. ) ;
#26261 = CARTESIAN_POINT ( 'NONE',  ( 810.7187646348534145, -426.4527844766010389, 356.7737145352016341 ) ) ;
#26264 = CARTESIAN_POINT ( 'NONE',  ( 780.5236548040995785, -308.7363362996979390, -314.9735926884559944 ) ) ;
#26265 = CARTESIAN_POINT ( 'NONE',  ( 755.0636971347428243, -316.2709662947832499, -341.7834795799807353 ) ) ;
#26266 = CARTESIAN_POINT ( 'NONE',  ( 805.1927285166397041, -160.8164208402382371, -341.8018195045277707 ) ) ;
#26267 = CARTESIAN_POINT ( 'NONE',  ( 767.7687537140311633, -431.9073299311464211, 372.7932403749916830 ) ) ;
#26268 = VECTOR ( 'NONE', #31121, 1000.000000000000000 ) ;
#26270 = DIRECTION ( 'NONE',  ( -1.000000000000000000, 0.000000000000000000, 0.000000000000000000 ) ) ;
#26269 = DIRECTION ( 'NONE',  ( -1.000000000000000000, 0.000000000000000000, 0.000000000000000000 ) ) ;
#26271 = CARTESIAN_POINT ( 'NONE',  ( 804.1009440267234822, -119.4636090269712554, -314.0944755984392600 ) ) ;
#26272 = CARTESIAN_POINT ( 'NONE',  ( 115.7583438952258774, -600.0000000000000000, -320.0000000000000568 ) ) ;
#26273 = LINE ( 'NONE', #29068, #17157 ) ;
#26274 = VECTOR ( 'NONE', #12680, 1000.000000000000000 ) ;
#26275 = CARTESIAN_POINT ( 'NONE',  ( 790.9844846989617508, -310.3726999360616219, 317.2208543904092721 ) ) ;
#26276 = CARTESIAN_POINT ( 'NONE',  ( 792.1044303154645831, -180.4527844766017211, 317.8323909638837677 ) ) ;
#26277 = ORIENTED_EDGE ( 'NONE', *, *, #24391, .T. ) ;
#26278 = CARTESIAN_POINT ( 'NONE',  ( 787.5162901302840055, -131.3618753856928549, -305.4481719005793252 ) ) ;
#26279 = DIRECTION ( 'NONE',  ( 1.000000000000000000, 0.000000000000000000, 0.000000000000000000 ) ) ;
#26280 = CARTESIAN_POINT ( 'NONE',  ( 810.4231160770870019, -72.55451811788049099, 321.9338519418446936 ) ) ;
#26281 = CARTESIAN_POINT ( 'NONE',  ( 796.9462024416508257, -276.4527844766013800, -308.9653473494370246 ) ) ;
#26282 = CARTESIAN_POINT ( 'NONE',  ( 749.2812353651451076, -438.4527844766009821, -323.2262854647983090 ) ) ;
#26283 = CARTESIAN_POINT ( 'NONE',  ( 803.6646147819161570, -137.9073299311473875, 348.8264449731210561 ) ) ;
#26284 = ORIENTED_EDGE ( 'NONE', *, *, #32600, .F. ) ;
#26285 = CARTESIAN_POINT ( 'NONE',  ( 758.0141637701419768, -351.0783235625955854, -367.2620300519063790 ) ) ;
#26286 = CARTESIAN_POINT ( 'NONE',  ( 748.9653473494363425, -98.63460265842024910, -356.9462024416521331 ) ) ;
#26287 = CARTESIAN_POINT ( 'NONE',  ( 801.5560724626406000, -0.5545181178807169209, 326.7756240680316182 ) ) ;
#26288 = CARTESIAN_POINT ( 'NONE',  ( 758.8095938919642549, -344.0891481129647786, -311.6929314249763365 ) ) ;
#26289 = LINE ( 'NONE', #15895, #38709 ) ;
#26290 = CARTESIAN_POINT ( 'NONE',  ( 786.6156483768007774, -409.4419599262317320, 315.5913626894246136 ) ) ;
#26291 = ORIENTED_EDGE ( 'NONE', *, *, #18756, .F. ) ;
#26292 = AXIS2_PLACEMENT_3D ( 'NONE', #45365, #10027, #7015 ) ;
#26293 = VECTOR ( 'NONE', #661, 1000.000000000000000 ) ;
#26294 = CARTESIAN_POINT ( 'NONE',  ( 795.6651683502461765, -106.7146871989600498, -371.3240766477733814 ) ) ;
#26295 = FACE_BOUND ( 'NONE', #16988, .T. ) ;
#26296 = CARTESIAN_POINT ( 'NONE',  ( 746.7653713866222915, -257.2601417444141134, 351.0478386215610271 ) ) ;
#26297 = CARTESIAN_POINT ( 'NONE',  ( 781.8018195045267476, -46.27096629478403855, 365.1927285166407273 ) ) ;
#26298 = ORIENTED_EDGE ( 'NONE', *, *, #693, .T. ) ;
#26299 = CARTESIAN_POINT ( 'NONE',  ( 804.1601925771018387, -223.4419599262323857, -346.5483106153029098 ) ) ;
#26300 = CARTESIAN_POINT ( 'NONE',  ( 759.7806653035534055, -222.9982390220561399, 324.8639956371180801 ) ) ;
#26301 = VECTOR ( 'NONE', #15872, 1000.000000000000000 ) ;
#26302 = CARTESIAN_POINT ( 'NONE',  ( 766.5853460496234675, -421.9874144716863498, -372.3518521366060554 ) ) ;
#26303 = CARTESIAN_POINT ( 'NONE',  ( 744.9990715423526808, -66.35105083532378956, -341.2370466360926002 ) ) ;
#26304 = FACE_OUTER_BOUND ( 'NONE', #39574, .T. ) ;
#26305 = ADVANCED_FACE ( 'NONE', ( #2700 ), #3146, .F. ) ;
#26306 = ORIENTED_EDGE ( 'NONE', *, *, #12906, .F. ) ;
#26307 = ORIENTED_EDGE ( 'NONE', *, *, #26147, .T. ) ;
#26308 = CARTESIAN_POINT ( 'NONE',  ( 764.1737431748507561, -370.3726999360613377, -371.6461892240376415 ) ) ;
#26309 = CARTESIAN_POINT ( 'NONE',  ( 774.6312213355099630, -239.3618753856924570, -364.6798772138717482 ) ) ;
#26310 = ADVANCED_FACE ( 'NONE', ( #17484 ), #20481, .F. ) ;
#26311 = CARTESIAN_POINT ( 'NONE',  ( 751.6929314249750860, -318.9982390220558841, 318.8095938919659034 ) ) ;
#26312 = CARTESIAN_POINT ( 'NONE',  ( 783.7566961878529810, -24.89650538077847486, 305.1792804349288417 ) ) ;
#26313 = CARTESIAN_POINT ( 'NONE',  ( 773.4516893846965786, -235.6454272087890729, -315.8398074228977066 ) ) ;
#26314 = CARTESIAN_POINT ( 'NONE',  ( 755.3201227861273992, -195.7255117493289731, -345.3687786644892981 ) ) ;
#26315 = CARTESIAN_POINT ( 'NONE',  ( 804.6798772138710092, -375.7255117493284047, -334.6312213355106451 ) ) ;
#26316 = ORIENTED_EDGE ( 'NONE', *, *, #45039, .F. ) ;
#26317 = CARTESIAN_POINT ( 'NONE',  ( 803.4237431249931660, -207.1800572038744406, 331.2633955100225194 ) ) ;
#26318 = CARTESIAN_POINT ( 'NONE',  ( 804.4286716492782716, -113.3618753856929260, -345.3141322388244703 ) ) ;
#26319 = ORIENTED_EDGE ( 'NONE', *, *, #42226, .F. ) ;
#26320 = VECTOR ( 'NONE', #37460, 1000.000000000000000 ) ;
#26321 = CARTESIAN_POINT ( 'NONE',  ( 747.2067596250078623, -339.1800572038740142, 352.2312462859687230 ) ) ;
#26322 = CARTESIAN_POINT ( 'NONE',  ( 799.9999999999993179, -512.9681489794448908, 350.0000000000000000 ) ) ;
#26323 = CARTESIAN_POINT ( 'NONE',  ( 799.9999999999993179, 197.3292319334027241, -273.4704985657796783 ) ) ;
#26324 = CARTESIAN_POINT ( 'NONE',  ( 571.1634899080285095, 258.0939999999999372, -199.9999999999981526 ) ) ;
#26325 = CARTESIAN_POINT ( 'NONE',  ( 763.8424801807145741, -186.0090635724255890, 320.5453621957614700 ) ) ;
#26326 = CARTESIAN_POINT ( 'NONE',  ( 762.1405469898971887, -73.54369356751118403, 357.8594530101015607 ) ) ;
#26327 = ORIENTED_EDGE ( 'NONE', *, *, #35742, .F. ) ;
#26328 = CARTESIAN_POINT ( 'NONE',  ( 763.8424801807145741, 5.990936427573807954, -320.5453621957614700 ) ) ;
#26329 = CARTESIAN_POINT ( 'NONE',  ( 772.4837098697145166, -47.36187538569312494, -374.5518280994205611 ) ) ;
#26330 = CARTESIAN_POINT ( 'NONE',  ( 763.2154366446407039, -261.6237781080504305, 321.4292242960311228 ) ) ;
#26331 = AXIS2_PLACEMENT_3D ( 'NONE', #11388, #7698, #21327 ) ;
#26332 = CARTESIAN_POINT ( 'NONE',  ( 756.3353852180819104, -413.9073299311465348, -331.1735550268788302 ) ) ;
#26333 = CARTESIAN_POINT ( 'NONE',  ( 765.0180583372156207, -24.99823902205683268, -360.0135310231089534 ) ) ;
#26334 = CARTESIAN_POINT ( 'NONE',  ( 782.5225473063381969, -430.2709662947827383, 375.2698199232970637 ) ) ;
#26335 = DIRECTION ( 'NONE',  ( -0.000000000000000000, 1.000000000000000000, -0.000000000000000000 ) ) ;
#26336 = CARTESIAN_POINT ( 'NONE',  ( 800.9840315886518738, -268.9181544815162397, -354.1144889064786412 ) ) ;
#26337 = CARTESIAN_POINT ( 'NONE',  ( 745.0891759886404770, -172.2709662947836478, -342.4968714119734159 ) ) ;
#26338 = AXIS2_PLACEMENT_3D ( 'NONE', #14474, #14707, #11007 ) ;
#26339 = CARTESIAN_POINT ( 'NONE',  ( 814.5518280994195948, -39.72551174932951312, 332.4837098697145734 ) ) ;
#26340 = CARTESIAN_POINT ( 'NONE',  ( 772.5602148656447525, -153.7255117493291721, 305.7998596910095443 ) ) ;
#26341 = CARTESIAN_POINT ( 'NONE',  ( 939.9999999999992042, 240.0000000000000568, 210.0000000000000000 ) ) ;
#26342 = CARTESIAN_POINT ( 'NONE',  ( 799.9999999999993179, -365.3551492539851893, -8.132432514707076621 ) ) ;
#26343 = CARTESIAN_POINT ( 'NONE',  ( 744.7301800767019131, -364.8164208402374697, 337.4774526936615757 ) ) ;
#26344 = CARTESIAN_POINT ( 'NONE',  ( 755.5713283507202505, -317.3618753856922581, -334.6858677611754729 ) ) ;
#26345 = CARTESIAN_POINT ( 'NONE',  ( 804.6798772138708955, -447.7255117493280636, 334.6312213355107019 ) ) ;
#26346 = CARTESIAN_POINT ( 'NONE',  ( 766.4474001241216001, -91.09997266333496668, -307.3154664389482491 ) ) ;
#26347 = CARTESIAN_POINT ( 'NONE',  ( 757.2208543904082489, -112.7146871989600356, -350.9844846989624330 ) ) ;
#26348 = CARTESIAN_POINT ( 'NONE',  ( 786.2056067578752163, -131.8055962898690439, 374.4686193811670023 ) ) ;
#26349 = CARTESIAN_POINT ( 'NONE',  ( 771.1735550268780344, -441.1800572038736163, 316.3353852180828198 ) ) ;
#26350 = AXIS2_PLACEMENT_3D ( 'NONE', #12808, #37526, #37756 ) ;
#26351 = CARTESIAN_POINT ( 'NONE',  ( 804.4286716492782716, -17.36187538569322086, -345.3141322388244703 ) ) ;
#26352 = CARTESIAN_POINT ( 'NONE',  ( 757.2208543904082489, -136.7146871989600072, -350.9844846989624330 ) ) ;
#26353 = CARTESIAN_POINT ( 'NONE',  ( 781.8018195045266339, -118.2709662947837899, -365.1927285166406705 ) ) ;
#26354 = CARTESIAN_POINT ( 'NONE',  ( 794.9819416627830151, -132.9982390220564810, 319.9864689768909898 ) ) ;
#26355 = EDGE_CURVE ( 'NONE', #35219, #39264, #39623, .T. ) ;
#26356 = CARTESIAN_POINT ( 'NONE',  ( 772.3691319403857278, -431.2601417444136018, -315.8894580844506663 ) ) ;
#26358 = CARTESIAN_POINT ( 'NONE',  ( 755.5713283507202505, -245.3618753856925139, 334.6858677611754729 ) ) ;
#26357 = CARTESIAN_POINT ( 'NONE',  ( 781.7834795799800531, -274.8164208402378108, 315.0636971347436202 ) ) ;
#26359 = DIRECTION ( 'NONE',  ( 0.000000000000000000, 0.000000000000000000, 1.000000000000000000 ) ) ;
#26360 = VERTEX_POINT ( 'NONE', #10088 ) ;
#26361 = CARTESIAN_POINT ( 'NONE',  ( 800.0135310231082713, -446.0891481129646081, 325.0180583372163028 ) ) ;
#26362 = CARTESIAN_POINT ( 'NONE',  ( 762.1177392798416577, -258.5545181178799226, -309.8865473780659272 ) ) ;
#26363 = AXIS2_PLACEMENT_3D ( 'NONE', #12553, #30106, #33340 ) ;
#26364 = VERTEX_POINT ( 'NONE', #2927 ) ;
#26365 = CARTESIAN_POINT ( 'NONE',  ( 0.000000000000000000, 0.000000000000000000, 0.000000000000000000 ) ) ;
#26366 = ADVANCED_FACE ( 'NONE', ( #41499 ), #38271, .F. ) ;
#26367 = CARTESIAN_POINT ( 'NONE',  ( 813.1304606946831655, -233.9073299311470464, 352.3570229623691716 ) ) ;
#26368 = CARTESIAN_POINT ( 'NONE',  ( 804.4086373105744769, -289.6454272087889308, 333.3843516231986541 ) ) ;
#26369 = CARTESIAN_POINT ( 'NONE',  ( 761.2382568024794409, -399.6237781080500326, 356.9571628226838129 ) ) ;
#26370 = ORIENTED_EDGE ( 'NONE', *, *, #12353, .T. ) ;
#26371 = CARTESIAN_POINT ( 'NONE',  ( 772.4468031744293057, -129.8272453906075725, -363.8651313633793620 ) ) ;
#26372 = CARTESIAN_POINT ( 'NONE',  ( 771.1735550268780344, -297.1800572038741279, -316.3353852180828198 ) ) ;
#26373 = ORIENTED_EDGE ( 'NONE', *, *, #29702, .T. ) ;
#26374 = CARTESIAN_POINT ( 'NONE',  ( 759.7806653035534055, -414.9982390220555430, -324.8639956371180801 ) ) ;
#26375 = CARTESIAN_POINT ( 'NONE',  ( 803.4237431249931660, -87.18005720387481006, -331.2633955100225194 ) ) ;
#26376 = CARTESIAN_POINT ( 'NONE',  ( 794.1144889064781864, -250.1692326535050199, 360.9840315886528401 ) ) ;
#26377 = CARTESIAN_POINT ( 'NONE',  ( 190.7583438952258916, 294.6698570112193920, -224.9999999999999716 ) ) ;
#26378 = CARTESIAN_POINT ( 'NONE',  ( 758.7867965644027208, 16.45630643248849267, 318.7867965644036872 ) ) ;
#26379 = CARTESIAN_POINT ( 'NONE',  ( 814.8207195650702488, -2.190881754244347945, -336.2433038121456548 ) ) ;
#26380 = PLANE ( 'NONE',  #24835 ) ;
#26381 = ORIENTED_EDGE ( 'NONE', *, *, #36022, .F. ) ;
#26382 = CARTESIAN_POINT ( 'NONE',  ( 745.1792804349281596, -302.1908817542433781, -343.7566961878542884 ) ) ;
#26383 = ADVANCED_FACE ( 'NONE', ( #21165 ), #3392, .F. ) ;
#26384 = CARTESIAN_POINT ( 'NONE',  ( 812.3518521366052028, -193.0999726633346256, 326.5853460496235243 ) ) ;
#26386 = CARTESIAN_POINT ( 'NONE',  ( 765.0180583372156207, -288.9982390220559978, -360.0135310231089534 ) ) ;
#26385 = CARTESIAN_POINT ( 'NONE',  ( 879.9999999999992042, 99.99999999999984368, 360.0000000000000000 ) ) ;
#26387 = EDGE_CURVE ( 'NONE', #14052, #33479, #35013, .T. ) ;
#26388 = CARTESIAN_POINT ( 'NONE',  ( 701.1634899080286232, 239.9999999999999432, -199.9999999999990337 ) ) ;
#26389 = CARTESIAN_POINT ( 'NONE',  ( 758.4439275373578084, -156.5545181178802636, -353.2243759319684386 ) ) ;
#26390 = CARTESIAN_POINT ( 'NONE',  ( 754.9967657858570647, -49.54369356751129061, 365.0032342141425374 ) ) ;
#26391 = LINE ( 'NONE', #36568, #42489 ) ;
#26392 = CARTESIAN_POINT ( 'NONE',  ( 800.9747183278959710, -348.9982390220558273, -311.9810565676471583 ) ) ;
#26393 = CARTESIAN_POINT ( 'NONE',  ( 799.9999999999993179, 205.0000000000000568, -265.0000000000000000 ) ) ;
#26394 = CARTESIAN_POINT ( 'NONE',  ( 778.1981804954714335, -34.27096629478407408, 314.8072714833589885 ) ) ;
#26395 = AXIS2_PLACEMENT_3D ( 'NONE', #42568, #10929, #21998 ) ;
#26396 = CARTESIAN_POINT ( 'NONE',  ( 744.6391490659812007, -278.7363362996980527, 338.7502325331110455 ) ) ;
#26397 = CARTESIAN_POINT ( 'NONE',  ( 800.9747183278959710, -252.9982390220560831, 311.9810565676471583 ) ) ;
#26398 = CARTESIAN_POINT ( 'NONE',  ( 787.5162901302840055, 12.63812461430668321, -305.4481719005792684 ) ) ;
#26399 = FACE_BOUND ( 'NONE', #26009, .T. ) ;
#26400 = DIRECTION ( 'NONE',  ( 1.000000000000000000, 0.000000000000000000, 0.000000000000000000 ) ) ;
#26401 = CARTESIAN_POINT ( 'NONE',  ( 804.9363028652555840, -352.2709662947830225, 338.2165204200192079 ) ) ;
#26402 = CARTESIAN_POINT ( 'NONE',  ( 755.3028492785439312, -111.2817908451530968, 335.9200461376539693 ) ) ;
#26403 = CARTESIAN_POINT ( 'NONE',  ( 794.1144889064781864, -10.16923265350579442, -360.9840315886528401 ) ) ;
#26404 = CARTESIAN_POINT ( 'NONE',  ( 939.9999999999992042, 74.99999999999984368, -360.0000000000000000 ) ) ;
#26405 = EDGE_CURVE ( 'NONE', #41138, #26699, #16716, .T. ) ;
#26406 = DIRECTION ( 'NONE',  ( -1.084653538143406060E-16, 0.6594541114781790059, 0.7517448203044204691 ) ) ;
#26407 = CARTESIAN_POINT ( 'NONE',  ( 800.2193346964447755, -402.9982390220555430, 355.1360043628815788 ) ) ;
#26408 = ORIENTED_EDGE ( 'NONE', *, *, #42804, .T. ) ;
#26409 = ADVANCED_FACE ( 'NONE', ( #20242 ), #38123, .F. ) ;
#26410 = CARTESIAN_POINT ( 'NONE',  ( 803.8651313633788504, -317.2601417444139429, -332.4468031744301015 ) ) ;
#26412 = CARTESIAN_POINT ( 'NONE',  ( 762.1405469898973024, -169.5436935675108998, 357.8594530101016176 ) ) ;
#26411 = CARTESIAN_POINT ( 'NONE',  ( 778.2165204200184689, -166.8164208402382087, 364.9363028652563230 ) ) ;
#26413 = CARTESIAN_POINT ( 'NONE',  ( 747.3154664389472828, -331.9874144716865203, -326.4474001241230781 ) ) ;
#26414 = CARTESIAN_POINT ( 'NONE',  ( 759.9999999999992042, -462.9681489794448339, -370.0000000000000568 ) ) ;
#26415 = ORIENTED_EDGE ( 'NONE', *, *, #33987, .F. ) ;
#26416 = CARTESIAN_POINT ( 'NONE',  ( 762.3223304703356007, -343.5436935675103314, 322.3223304703362828 ) ) ;
#26417 = ORIENTED_EDGE ( 'NONE', *, *, #14833, .T. ) ;
#26418 = DIRECTION ( 'NONE',  ( -0.000000000000000000, -0.000000000000000000, 1.000000000000000000 ) ) ;
#26419 = EDGE_CURVE ( 'NONE', #36186, #26697, #31563, .T. ) ;
#26420 = EDGE_CURVE ( 'NONE', #17231, #16198, #9444, .T. ) ;
#26421 = CARTESIAN_POINT ( 'NONE',  ( 759.0252816721024374, -168.9982390220563673, -368.0189434323527280 ) ) ;
#26422 = CARTESIAN_POINT ( 'NONE',  ( 801.1904061080338124, -68.08914811296577341, 368.3070685750236066 ) ) ;
#26423 = ORIENTED_EDGE ( 'NONE', *, *, #8949, .T. ) ;
#26424 = CARTESIAN_POINT ( 'NONE',  ( 788.7366044899766848, -179.9073299311472454, -316.5762568750059813 ) ) ;
#26425 = ORIENTED_EDGE ( 'NONE', *, *, #4111, .T. ) ;
#26426 = VECTOR ( 'NONE', #7556, 1000.000000000000000 ) ;
#26427 = CARTESIAN_POINT ( 'NONE',  ( 801.5560724626406000, -456.5545181178792404, -326.7756240680316182 ) ) ;
#26428 = CARTESIAN_POINT ( 'NONE',  ( 751.9810565676468741, -266.0891481129651197, 360.9747183278973921 ) ) ;
#26429 = CARTESIAN_POINT ( 'NONE',  ( 802.7791456095903868, -172.7146871989598083, 329.0155153010375102 ) ) ;
#26432 = CARTESIAN_POINT ( 'NONE',  ( 814.8230680027162407, -413.8055962898681059, 333.7305795820267917 ) ) ;
#26431 = CARTESIAN_POINT ( 'NONE',  ( -66.63011601220125613, -365.3551492539851893, -8.132432514707076621 ) ) ;
#26430 = FACE_OUTER_BOUND ( 'NONE', #6877, .T. ) ;
#26433 = EDGE_LOOP ( 'NONE', ( #12570, #31079, #22990, #44661 ) ) ;
#26434 = CARTESIAN_POINT ( 'NONE',  ( 763.0428371773158460, -443.4636090269702322, -358.7617431975195359 ) ) ;
#26435 = FACE_OUTER_BOUND ( 'NONE', #23795, .T. ) ;
#26436 = ORIENTED_EDGE ( 'NONE', *, *, #44243, .F. ) ;
#26437 = CARTESIAN_POINT ( 'NONE',  ( 773.7305795820266212, -201.2817908451528126, -374.8230680027170365 ) ) ;
#26438 = CARTESIAN_POINT ( 'NONE',  ( 757.7880784355613741, -90.00906357242590161, 312.4576283171834916 ) ) ;
#26440 = CARTESIAN_POINT ( 'NONE',  ( 791.9812246680005501, -188.6346026584199365, -361.9419747391813189 ) ) ;
#26439 = CARTESIAN_POINT ( 'NONE',  ( 779.9999999999992042, 126.4563064324884465, -350.0000000000000000 ) ) ;
#26441 = CARTESIAN_POINT ( 'NONE',  ( 773.3843516231979720, -349.4419599262320162, -364.4086373105754433 ) ) ;
#26442 = DIRECTION ( 'NONE',  ( 0.000000000000000000, -1.000000000000000000, 0.000000000000000000 ) ) ;
#26443 = CARTESIAN_POINT ( 'NONE',  ( 745.5313806188320314, -207.2817908451527842, -333.7943932421247268 ) ) ;
#26444 = CARTESIAN_POINT ( 'NONE',  ( 879.9999999999992042, 469.9999999999998863, -360.0000000000000000 ) ) ;
#26445 = DIRECTION ( 'NONE',  ( 0.000000000000000000, 0.000000000000000000, 1.000000000000000000 ) ) ;
#26446 = CARTESIAN_POINT ( 'NONE',  ( 758.4439275373578084, -36.55451811788061178, -353.2243759319684386 ) ) ;
#26447 = CARTESIAN_POINT ( 'NONE',  ( 790.0220218866281812, -391.0999726633340288, 363.2186876482849129 ) ) ;
#26448 = CARTESIAN_POINT ( 'NONE',  ( 800.9747183278959710, -228.9982390220561683, -311.9810565676471583 ) ) ;
#26449 = CARTESIAN_POINT ( 'NONE',  ( 804.8461984189677878, -242.1908817542435770, 336.9566956441385628 ) ) ;
#26450 = CARTESIAN_POINT ( 'NONE',  ( 989.9999999999992042, 50.81038600091411439, 210.0000000000000000 ) ) ;
#26451 = CARTESIAN_POINT ( 'NONE',  ( 989.9999999999992042, 62.85347435602256638, 357.4246812887967053 ) ) ;
#26452 = CARTESIAN_POINT ( 'NONE',  ( 755.5713283507202505, -53.36187538569310362, -334.6858677611754729 ) ) ;
#26453 = CARTESIAN_POINT ( 'NONE',  ( 745.5313806188320314, -183.2817908451528695, 333.7943932421247268 ) ) ;
#26454 = CARTESIAN_POINT ( 'NONE',  ( 746.0683387631852383, -139.4419599262326699, -331.3260364891676204 ) ) ;
#26455 = CARTESIAN_POINT ( 'NONE',  ( 787.5162901302840055, -155.3618753856927128, 305.4481719005792684 ) ) ;
#26456 = CARTESIAN_POINT ( 'NONE',  ( 808.0189434323515343, -374.0891481129647786, -319.0252816721025511 ) ) ;
#26457 = PLANE ( 'NONE',  #34231 ) ;
#26458 = CARTESIAN_POINT ( 'NONE',  ( 797.6776695296629214, -259.5436935675106156, 357.6776695296636603 ) ) ;
#26459 = CARTESIAN_POINT ( 'NONE',  ( 779.4763451958990572, -32.73633629969879877, 365.0264073115438919 ) ) ;
#26460 = CARTESIAN_POINT ( 'NONE',  ( 774.6858677611749044, -393.7255117493283478, -315.5713283507209894 ) ) ;
#26461 = DIRECTION ( 'NONE',  ( -0.000000000000000000, -0.000000000000000000, -1.000000000000000000 ) ) ;
#26462 = EDGE_CURVE ( 'NONE', #2273, #22437, #45512, .T. ) ;
#26463 = CARTESIAN_POINT ( 'NONE',  ( 800.9747183278959710, -444.9982390220554862, -311.9810565676471583 ) ) ;
#26464 = FACE_OUTER_BOUND ( 'NONE', #45343, .T. ) ;
#26466 = CARTESIAN_POINT ( 'NONE',  ( 804.9363028652555840, -304.2709662947832499, 338.2165204200192079 ) ) ;
#26465 = CARTESIAN_POINT ( 'NONE',  ( 754.9735926884551418, -90.35105083532373271, 340.5236548041000333 ) ) ;
#26467 = ORIENTED_EDGE ( 'NONE', *, *, #15993, .F. ) ;
#26468 = CARTESIAN_POINT ( 'NONE',  ( 805.0264073115434940, -222.3510508353233206, -339.4763451958999099 ) ) ;
#26469 = CARTESIAN_POINT ( 'NONE',  ( 767.8955696845333705, -72.45278447660213317, 362.1676090361162323 ) ) ;
#26470 = CARTESIAN_POINT ( 'NONE',  ( 744.9990715423526808, -234.3510508353232638, -341.2370466360926002 ) ) ;
#26471 = CARTESIAN_POINT ( 'NONE',  ( 181.9156952255813735, 290.0000000000001137, -244.9999999999999716 ) ) ;
#26472 = CARTESIAN_POINT ( 'NONE',  ( 747.3154664389472828, -355.9874144716865203, 326.4474001241230781 ) ) ;
#26473 = ORIENTED_EDGE ( 'NONE', *, *, #30371, .F. ) ;
#26474 = CARTESIAN_POINT ( 'NONE',  ( 768.8385539511368734, -431.2601417444136018, 306.4236121716840557 ) ) ;
#26475 = CARTESIAN_POINT ( 'NONE',  ( 774.6858677611749044, -369.7255117493284615, 315.5713283507209894 ) ) ;
#26476 = CARTESIAN_POINT ( 'NONE',  ( 787.4397851343537695, -69.72551174932942786, -374.2001403089903988 ) ) ;
#26477 = CARTESIAN_POINT ( 'NONE',  ( 762.3223304703356007, -79.54369356751119824, -322.3223304703362828 ) ) ;
#26478 = EDGE_LOOP ( 'NONE', ( #12335, #6755, #472, #37362 ) ) ;
#26479 = CARTESIAN_POINT ( 'NONE',  ( 787.5531968255692163, -21.82724539060792424, -316.1348686366205811 ) ) ;
#26480 = VERTEX_POINT ( 'NONE', #24381 ) ;
#26481 = CARTESIAN_POINT ( 'NONE',  ( 793.9708237608222134, -334.9181544815160692, -319.2295555964448681 ) ) ;
#26482 = CONTEXT_DEPENDENT_SHAPE_REPRESENTATION ( #14033, #27342 ) ;
#26484 = CARTESIAN_POINT ( 'NONE',  ( 804.8461984189677878, -410.1908817542430370, 336.9566956441385628 ) ) ;
#26483 = CARTESIAN_POINT ( 'NONE',  ( 768.0187753319979720, -80.63460265842029173, 318.0580252608186242 ) ) ;
#26487 = CARTESIAN_POINT ( 'NONE',  ( 747.3154664389472828, -331.9874144716865203, 326.4474001241230781 ) ) ;
#26486 = DIRECTION ( 'NONE',  ( 0.000000000000000000, 0.000000000000000000, -1.000000000000000000 ) ) ;
#26485 = CARTESIAN_POINT ( 'NONE',  ( 792.2312462859673587, -443.9073299311464780, 307.2067596250082602 ) ) ;
#26488 = CARTESIAN_POINT ( 'NONE',  ( 761.9338519418445230, -110.5328690171418629, 370.4231160770881957 ) ) ;
#26489 = CARTESIAN_POINT ( 'NONE',  ( 790.0220218866281812, -319.0999726633342561, -363.2186876482849129 ) ) ;
#26490 = CARTESIAN_POINT ( 'NONE',  ( 797.8594530101008786, -325.5436935675105019, -322.1405469898980982 ) ) ;
#26491 = CARTESIAN_POINT ( 'NONE',  ( 794.9819416627830151, -156.9982390220564241, -319.9864689768909898 ) ) ;
#26492 = CARTESIAN_POINT ( 'NONE',  ( 808.0189434323515343, -422.0891481129647218, 319.0252816721025511 ) ) ;
#26494 = CYLINDRICAL_SURFACE ( 'NONE', #16745, 2.749999999999863665 ) ;
#26493 = CARTESIAN_POINT ( 'NONE',  ( 959.5497976682736407, 120.6654763175833693, 339.9999999999998863 ) ) ;
#26495 = CARTESIAN_POINT ( 'NONE',  ( 758.6633372737375112, -260.5328690171413086, -326.9102291470432533 ) ) ;
#26496 = CARTESIAN_POINT ( 'NONE',  ( 754.3581564841646241, -113.4636090269712554, -316.1443688327762516 ) ) ;
#26497 = CYLINDRICAL_SURFACE ( 'NONE', #4228, 2.749999999999863665 ) ;
#26498 = CARTESIAN_POINT ( 'NONE',  ( -786.4999999999993179, -512.9681489794448908, -327.9999999999999432 ) ) ;
#26499 = CARTESIAN_POINT ( 'NONE',  ( 804.8461984189677878, -314.1908817542433781, 336.9566956441385628 ) ) ;
#26500 = ORIENTED_EDGE ( 'NONE', *, *, #32641, .F. ) ;
#26501 = CARTESIAN_POINT ( 'NONE',  ( 745.7998596910086917, -149.3618753856928265, -332.5602148656461168 ) ) ;
#26502 = CARTESIAN_POINT ( 'NONE',  ( 701.1634899080286232, 239.9999999999999147, -199.9999999999990337 ) ) ;
#26503 = CARTESIAN_POINT ( 'NONE',  ( 766.4474001241216001, -91.09997266333496668, 307.3154664389482491 ) ) ;
#26504 = CARTESIAN_POINT ( 'NONE',  ( 777.5031285880264704, -262.8164208402379245, -374.9108240113588408 ) ) ;
#26505 = CARTESIAN_POINT ( 'NONE',  ( -769.9999999999992042, 205.0000000000000568, -339.9999999999999432 ) ) ;
#26506 = CARTESIAN_POINT ( 'NONE',  ( 774.6858677611749044, -153.7255117493291721, 315.5713283507209894 ) ) ;
#26507 = ORIENTED_EDGE ( 'NONE', *, *, #138, .F. ) ;
#26508 = CARTESIAN_POINT ( 'NONE',  ( 748.3538107759620743, -352.7146871989593251, -355.8262568251490165 ) ) ;
#26509 = CARTESIAN_POINT ( 'NONE',  ( 745.0891759886404770, -76.27096629478394618, -342.4968714119734159 ) ) ;
#26510 = CARTESIAN_POINT ( 'NONE',  ( 759.0159684113467620, -16.91815448151702839, 325.8855110935213020 ) ) ;
#26511 = CARTESIAN_POINT ( 'NONE',  ( 800.9747183278959710, -348.9982390220558273, -311.9810565676471583 ) ) ;
#26512 = DIRECTION ( 'NONE',  ( -0.000000000000000000, 1.000000000000000000, -0.000000000000000000 ) ) ;
#26513 = CARTESIAN_POINT ( 'NONE',  ( 773.3843516231979720, -397.4419599262317320, 364.4086373105754433 ) ) ;
#26514 = EDGE_LOOP ( 'NONE', ( #33803, #12294, #16027, #45461 ) ) ;
#26515 = CARTESIAN_POINT ( 'NONE',  ( 767.8955696845333705, -216.4527844766016926, -362.1676090361162323 ) ) ;
#26516 = ADVANCED_FACE ( 'NONE', ( #45430 ), #31773, .T. ) ;
#26517 = CARTESIAN_POINT ( 'NONE',  ( 761.9338519418445230, -134.5328690171417350, -370.4231160770881957 ) ) ;
#26518 = DIRECTION ( 'NONE',  ( -0.000000000000000000, 1.000000000000000000, -0.000000000000000000 ) ) ;
#26519 = CARTESIAN_POINT ( 'NONE',  ( 791.1614460488616487, -251.2601417444141134, 373.5763878283158874 ) ) ;
#26520 = CARTESIAN_POINT ( 'NONE',  ( 778.2165204200184689, -70.81642084023850714, 364.9363028652563230 ) ) ;
#26521 = AXIS2_PLACEMENT_3D ( 'NONE', #13488, #45362, #28020 ) ;
#26522 = VERTEX_POINT ( 'NONE', #13793 ) ;
#26523 = CARTESIAN_POINT ( 'NONE',  ( 787.6308680596127942, -11.26014174441488258, -364.1105419155492768 ) ) ;
#26524 = CARTESIAN_POINT ( 'NONE',  ( 804.9363028652555840, -232.2709662947834488, 338.2165204200192079 ) ) ;
#26525 = CARTESIAN_POINT ( 'NONE',  ( 749.8865473780648472, -428.5328690171409107, -322.1177392798429082 ) ) ;
#26526 = CARTESIAN_POINT ( 'NONE',  ( 187.1337867209877857, -184.9457194955397199, 62.92409052808242365 ) ) ;
#26527 = ORIENTED_EDGE ( 'NONE', *, *, #33765, .T. ) ;
#26528 = EDGE_LOOP ( 'NONE', ( #40145, #27654 ) ) ;
#26529 = CARTESIAN_POINT ( 'NONE',  ( 754.3581564841646241, -377.4636090269704596, -316.1443688327762516 ) ) ;
#26530 = CARTESIAN_POINT ( 'NONE',  ( 765.0180583372156207, -240.9982390220561683, -360.0135310231089534 ) ) ;
#26531 = CARTESIAN_POINT ( 'NONE',  ( 792.3570229623691148, -309.1800572038740711, 373.1304606946836770 ) ) ;
#26532 = CARTESIAN_POINT ( 'NONE',  ( 745.1769319972822814, -41.80559628986934229, 346.2694204179732083 ) ) ;
#26533 = CARTESIAN_POINT ( 'NONE',  ( 769.9779781133707957, -211.0999726633346540, -316.7813123517150871 ) ) ;
#26534 = CARTESIAN_POINT ( 'NONE',  ( 801.9419747391806368, -210.4527844766016926, -351.9812246680014027 ) ) ;
#26535 = CARTESIAN_POINT ( 'NONE',  ( 762.3223304703356007, -391.5436935675101608, -322.3223304703362828 ) ) ;
#26536 = ORIENTED_EDGE ( 'NONE', *, *, #17279, .F. ) ;
#26537 = CARTESIAN_POINT ( 'NONE',  ( 756.3353852180819104, -197.9073299311472169, 331.1735550268788302 ) ) ;
#26538 = CARTESIAN_POINT ( 'NONE',  ( 801.9419747391806368, -114.4527844766020053, -351.9812246680014027 ) ) ;
#26539 = ORIENTED_EDGE ( 'NONE', *, *, #21860, .F. ) ;
#26540 = CARTESIAN_POINT ( 'NONE',  ( 772.4837098697144029, -335.3618753856920307, 374.5518280994205611 ) ) ;
#26541 = DIRECTION ( 'NONE',  ( 0.000000000000000000, 0.000000000000000000, -1.000000000000000000 ) ) ;
#26542 = CARTESIAN_POINT ( 'NONE',  ( 779.9999999999992042, -462.9681489794448339, 339.9999999999999432 ) ) ;
#26543 = DIRECTION ( 'NONE',  ( 0.000000000000000000, -0.7651688349527138167, -0.6438296778008192334 ) ) ;
#26544 = CARTESIAN_POINT ( 'NONE',  ( 755.1538015810308480, -206.1908817542437191, 343.0433043558613804 ) ) ;
#26545 = CARTESIAN_POINT ( 'NONE',  ( 792.1044303154645831, -84.45278447660206211, 317.8323909638837677 ) ) ;
#26546 = ORIENTED_EDGE ( 'NONE', *, *, #21883, .T. ) ;
#26547 = CARTESIAN_POINT ( 'NONE',  ( 745.7194118038753459, -445.6454272087883055, -348.7631598425976449 ) ) ;
#26548 = CARTESIAN_POINT ( 'NONE',  ( 787.5162901302840055, -35.36187538569316047, -305.4481719005793252 ) ) ;
#26549 = CARTESIAN_POINT ( 'NONE',  ( 800.7704444035546203, -268.1692326535049347, 326.0291762391768771 ) ) ;
#26550 = CARTESIAN_POINT ( 'NONE',  ( 785.3141322388236176, -381.7255117493284615, -364.4286716492789537 ) ) ;
#26551 = CARTESIAN_POINT ( 'NONE',  ( 797.8594530101009923, -13.54369356751140963, -322.1405469898982119 ) ) ;
#26552 = CARTESIAN_POINT ( 'NONE',  ( 800.9747183278959710, -444.9982390220554862, 311.9810565676471583 ) ) ;
#26553 = DIRECTION ( 'NONE',  ( -1.000000000000000000, -0.000000000000000000, -0.000000000000000000 ) ) ;
#26554 = CARTESIAN_POINT ( 'NONE',  ( 761.4292242960306112, -281.4636090269706870, -323.2154366446414429 ) ) ;
#26555 = CARTESIAN_POINT ( 'NONE',  ( 758.8095938919642549, -152.0891481129655460, -311.6929314249763365 ) ) ;
#26556 = CARTESIAN_POINT ( 'NONE',  ( 814.9108240113580450, -88.27096629478390355, 337.5031285880265273 ) ) ;
#26557 = CARTESIAN_POINT ( 'NONE',  ( 808.0189434323515343, -134.0891481129655745, 319.0252816721025511 ) ) ;
#26558 = DIRECTION ( 'NONE',  ( 1.337618101958019798E-16, -1.000000000000000000, 0.000000000000000000 ) ) ;
#26559 =( NAMED_UNIT ( * ) PLANE_ANGLE_UNIT ( ) SI_UNIT ( $, .RADIAN. ) );
#26560 = DIRECTION ( 'NONE',  ( 0.000000000000000000, 1.000000000000000000, 0.000000000000000000 ) ) ;
#26561 = CARTESIAN_POINT ( 'NONE',  ( 813.1304606946830518, -353.9073299311467053, 352.3570229623690580 ) ) ;
#26562 = CARTESIAN_POINT ( 'NONE',  ( 754.8072714833581358, -364.8164208402374697, -338.1981804954720587 ) ) ;
#26563 = CARTESIAN_POINT ( 'NONE',  ( 763.2154366446407039, 26.37622189194863509, 321.4292242960311228 ) ) ;
#26564 = CARTESIAN_POINT ( 'NONE',  ( 788.6739635108323228, -103.6454272087894850, -373.9316612368139090 ) ) ;
#26565 = CARTESIAN_POINT ( 'NONE',  ( 759.2295555964440155, -112.1692326535054889, -353.9708237608231229 ) ) ;
#26566 = CARTESIAN_POINT ( 'NONE',  ( 768.8385539511368734, -119.2601417444145397, 306.4236121716840557 ) ) ;
#26567 = CARTESIAN_POINT ( 'NONE',  ( 779.9999999999992042, -452.9681489794448339, 339.9999999999999432 ) ) ;
#26568 = CARTESIAN_POINT ( 'NONE',  ( 762.1405469898971887, -25.54369356751136877, -357.8594530101015607 ) ) ;
#26569 = CARTESIAN_POINT ( 'NONE',  ( 766.7756240680305382, -182.5328690171416497, -361.5560724626415663 ) ) ;
#26570 = CARTESIAN_POINT ( 'NONE',  ( 801.9419747391806368, -138.4527844766019200, -351.9812246680014027 ) ) ;
#26571 = CARTESIAN_POINT ( 'NONE',  ( 803.6646147819161570, -113.9073299311474301, 348.8264449731210561 ) ) ;
#26572 = CARTESIAN_POINT ( 'NONE',  ( 799.4546378042377910, -417.0783235625954148, -356.1575198192848006 ) ) ;
#26574 = CARTESIAN_POINT ( 'NONE',  ( 781.7834795799800531, -274.8164208402378108, 315.0636971347436202 ) ) ;
#26573 = CARTESIAN_POINT ( 'NONE',  ( 781.7834795799800531, -298.8164208402377540, 315.0636971347436202 ) ) ;
#26575 = LINE ( 'NONE', #37441, #19737 ) ;
#26576 = ORIENTED_EDGE ( 'NONE', *, *, #30897, .T. ) ;
#26577 = CARTESIAN_POINT ( 'NONE',  ( 804.6798772138708955, -447.7255117493280636, 334.6312213355107019 ) ) ;
#26578 = CARTESIAN_POINT ( 'NONE',  ( 797.8822607201568644, -270.5545181178798657, -370.1134526219340160 ) ) ;
#26579 = VERTEX_POINT ( 'NONE', #41735 ) ;
#26580 = DIRECTION ( 'NONE',  ( 1.000000000000000000, 0.000000000000000000, 0.000000000000000000 ) ) ;
#26581 = CARTESIAN_POINT ( 'NONE',  ( 808.3070685750232087, -210.9982390220562252, 361.1904061080339829 ) ) ;
#26582 = CARTESIAN_POINT ( 'NONE',  ( 804.4086373105744769, -313.6454272087888171, 333.3843516231986541 ) ) ;
#26583 = CARTESIAN_POINT ( 'NONE',  ( 764.0069404352550464, -399.0783235625955285, 359.2566176426627180 ) ) ;
#26584 = EDGE_LOOP ( 'NONE', ( #14633, #36708, #23802, #43980 ) ) ;
#26585 = CARTESIAN_POINT ( 'NONE',  ( 790.0220218866281812, -127.0999726633348672, -363.2186876482849129 ) ) ;
#26586 = CARTESIAN_POINT ( 'NONE',  ( 765.0180583372156207, -96.99823902205660886, -360.0135310231089534 ) ) ;
#26587 = CARTESIAN_POINT ( 'NONE',  ( 778.1981804954715471, -298.2709662947831930, -314.8072714833591021 ) ) ;
#26588 = ORIENTED_EDGE ( 'NONE', *, *, #30911, .F. ) ;
#26589 = CARTESIAN_POINT ( 'NONE',  ( 785.3141322388236176, -429.7255117493282910, -364.4286716492789537 ) ) ;
#26590 = CARTESIAN_POINT ( 'NONE',  ( 781.8018195045266339, -70.27096629478397460, -365.1927285166406705 ) ) ;
#26591 = CARTESIAN_POINT ( 'NONE',  ( 794.1144889064781864, -298.1692326535049347, 360.9840315886528401 ) ) ;
#26592 = PLANE ( 'NONE',  #43273 ) ;
#26593 = DIRECTION ( 'NONE',  ( 0.000000000000000000, 1.000000000000000000, 0.000000000000000000 ) ) ;
#26594 = CARTESIAN_POINT ( 'NONE',  ( 762.3223304703356007, 16.45630643248849267, 322.3223304703362828 ) ) ;
#26595 = VERTEX_POINT ( 'NONE', #23692 ) ;
#26596 = CARTESIAN_POINT ( 'NONE',  ( 750.9282345327678740, -352.9181544815159555, -319.8311093483690115 ) ) ;
#26597 = CARTESIAN_POINT ( 'NONE',  ( 810.4231160770870019, -192.5545181178801215, 321.9338519418446936 ) ) ;
#26599 = CARTESIAN_POINT ( 'NONE',  ( 781.8018195045266339, -286.2709662947833635, -365.1927285166406705 ) ) ;
#26598 = CARTESIAN_POINT ( 'NONE',  ( -784.4999999999993179, -513.1383975375929367, -349.9999999999999432 ) ) ;
#26600 = DIRECTION ( 'NONE',  ( 1.000000000000000000, 0.000000000000000000, -0.000000000000000000 ) ) ;
#26601 = CARTESIAN_POINT ( 'NONE',  ( 775.8780910478218402, -201.2817908451528126, -364.9511171171680530 ) ) ;
#26602 = EDGE_CURVE ( 'NONE', #22122, #30282, #28561, .T. ) ;
#26603 = CARTESIAN_POINT ( 'NONE',  ( 751.6929314249748586, -30.99823902205680071, 318.8095938919659034 ) ) ;
#26604 = FACE_OUTER_BOUND ( 'NONE', #32726, .T. ) ;
#26605 = CARTESIAN_POINT ( 'NONE',  ( 745.4481719005789273, -387.7255117493284047, -347.5162901302853697 ) ) ;
#26606 = DIRECTION ( 'NONE',  ( -0.000000000000000000, -0.000000000000000000, -1.000000000000000000 ) ) ;
#26607 = CARTESIAN_POINT ( 'NONE',  ( 781.7834795799800531, -58.81642084023854267, 315.0636971347436202 ) ) ;
#26608 = CARTESIAN_POINT ( 'NONE',  ( 812.3518521366052028, -313.0999726633342561, 326.5853460496235243 ) ) ;
#26609 = CARTESIAN_POINT ( 'NONE',  ( 805.0032342141412300, -253.5436935675104735, 314.9967657858571783 ) ) ;
#26610 = CARTESIAN_POINT ( 'NONE',  ( 800.9747183278959710, -12.99823902205686821, -311.9810565676471583 ) ) ;
#26611 = EDGE_CURVE ( 'NONE', #8154, #15790, #19709, .T. ) ;
#26612 = CARTESIAN_POINT ( 'NONE',  ( 778.2165204200184689, -238.8164208402379813, -364.9363028652563230 ) ) ;
#26613 = CARTESIAN_POINT ( 'NONE',  ( 799.9999999999993179, 205.0000000000000568, -319.9999999999999432 ) ) ;
#26614 = CARTESIAN_POINT ( 'NONE',  ( 804.6798772138708955, -351.7255117493284047, 334.6312213355107019 ) ) ;
#26615 = AXIS2_PLACEMENT_3D ( 'NONE', #26388, #8627, #12742 ) ;
#26616 = CARTESIAN_POINT ( 'NONE',  ( 759.0159684113467620, -112.9181544815167229, 325.8855110935213020 ) ) ;
#26617 = CARTESIAN_POINT ( 'NONE',  ( 773.3843516231979720, -13.44195992623305713, -364.4086373105754433 ) ) ;
#26618 = CARTESIAN_POINT ( 'NONE',  ( 989.9999999999992042, -185.0721577059061929, -75.19946970736501157 ) ) ;
#26619 = DIRECTION ( 'NONE',  ( 0.000000000000000000, 0.000000000000000000, 1.000000000000000000 ) ) ;
#26620 = CARTESIAN_POINT ( 'NONE',  ( 771.2368401574024119, -133.4419599262326699, 374.2805881961240857 ) ) ;
#26621 = CARTESIAN_POINT ( 'NONE',  ( 781.8018195045266339, -382.2709662947828519, 365.1927285166406705 ) ) ;
#26622 = EDGE_LOOP ( 'NONE', ( #19619, #34109, #29503, #40045 ) ) ;
#26623 = CARTESIAN_POINT ( 'NONE',  ( 769.1273215169530886, -334.7146871989593251, -317.4527132478988847 ) ) ;
#26625 = CARTESIAN_POINT ( 'NONE',  ( 771.2633955100217236, -143.9073299311473590, 363.4237431249939618 ) ) ;
#26624 = CARTESIAN_POINT ( 'NONE',  ( 768.0187753319979720, -176.6346026584199933, 318.0580252608186242 ) ) ;
#26626 = CARTESIAN_POINT ( 'NONE',  ( 746.7653713866222915, -377.2601417444137724, -351.0478386215610271 ) ) ;
#26627 = CARTESIAN_POINT ( 'NONE',  ( 799.9999999999993179, 205.0000000000000568, 339.9999999999999432 ) ) ;
#26628 = EDGE_CURVE ( 'NONE', #15565, #5169, #11615, .T. ) ;
#26629 = ORIENTED_EDGE ( 'NONE', *, *, #14281, .T. ) ;
#26630 = CARTESIAN_POINT ( 'NONE',  ( 756.3353852180819104, -341.9073299311465917, 331.1735550268788302 ) ) ;
#26631 = ADVANCED_FACE ( 'NONE', ( #7538 ), #4523, .F. ) ;
#26632 = ORIENTED_EDGE ( 'NONE', *, *, #7420, .T. ) ;
#26633 = FACE_OUTER_BOUND ( 'NONE', #1127, .T. ) ;
#26634 = CARTESIAN_POINT ( 'NONE',  ( 748.9653473494363425, -194.6346026584198796, -356.9462024416521331 ) ) ;
#26635 = CARTESIAN_POINT ( 'NONE',  ( 746.8695393053151292, -101.9073299311474869, 327.6429770376306578 ) ) ;
#26636 = EDGE_CURVE ( 'NONE', #15138, #27605, #18171, .T. ) ;
#26637 = ORIENTED_EDGE ( 'NONE', *, *, #8659, .F. ) ;
#26638 = CARTESIAN_POINT ( 'NONE',  ( 803.6646147819162707, -161.9073299311472738, -348.8264449731211130 ) ) ;
#26639 = ORIENTED_EDGE ( 'NONE', *, *, #43810, .F. ) ;
#26640 = CARTESIAN_POINT ( 'NONE',  ( 760.7433823573367135, -444.0090635724249069, -355.9930595647440441 ) ) ;
#26641 = CARTESIAN_POINT ( 'NONE',  ( 745.4481719005789273, -243.7255117493287742, 347.5162901302853129 ) ) ;
#26642 = CARTESIAN_POINT ( 'NONE',  ( 764.0069404352550464, -207.0783235625960685, 359.2566176426627180 ) ) ;
#26644 = CYLINDRICAL_SURFACE ( 'NONE', #15937, 10.00000000000000888 ) ;
#26643 = FACE_OUTER_BOUND ( 'NONE', #29219, .T. ) ;
#26645 = ORIENTED_EDGE ( 'NONE', *, *, #11519, .T. ) ;
#26646 = CARTESIAN_POINT ( 'NONE',  ( 760.7433823573367135, -420.0090635724249069, -355.9930595647440441 ) ) ;
#26647 = CARTESIAN_POINT ( 'NONE',  ( 939.9999999999993179, -600.0000000000001137, -360.0000000000000000 ) ) ;
#26648 = CARTESIAN_POINT ( 'NONE',  ( 768.9521613784389729, -249.8272453906072315, -373.2346286133773106 ) ) ;
#26649 = AXIS2_PLACEMENT_3D ( 'NONE', #12526, #5591, #1661 ) ;
#26650 = CARTESIAN_POINT ( 'NONE',  ( 744.6391490659812007, -86.73633629969862113, 338.7502325331110455 ) ) ;
#26652 = CARTESIAN_POINT ( 'NONE',  ( 801.9419747391806368, -186.4527844766017779, -351.9812246680014027 ) ) ;
#26651 = DIRECTION ( 'NONE',  ( -0.000000000000000000, 1.000000000000000000, -0.000000000000000000 ) ) ;
#26653 = ADVANCED_FACE ( 'NONE', ( #18396 ), #3840, .F. ) ;
#26654 = CARTESIAN_POINT ( 'NONE',  ( 784.0799538623451781, -347.8055962898683333, -364.6971507214555572 ) ) ;
#26655 = DIRECTION ( 'NONE',  ( -0.000000000000000000, 1.000000000000000000, -0.000000000000000000 ) ) ;
#26656 = CARTESIAN_POINT ( 'NONE',  ( 795.8262568251477660, -238.3726999360617640, -308.3538107759623585 ) ) ;
#26657 = DIRECTION ( 'NONE',  ( 0.000000000000000000, -1.000000000000000000, 0.000000000000000000 ) ) ;
#26658 = DIRECTION ( 'NONE',  ( 0.000000000000000000, 1.000000000000000000, -0.000000000000000000 ) ) ;
#26659 = CARTESIAN_POINT ( 'NONE',  ( 786.5483106153019435, -31.64542720878970883, -364.1601925771022366 ) ) ;
#26660 = CARTESIAN_POINT ( 'NONE',  ( 769.9779781133707957, -451.0999726633339151, 316.7813123517150871 ) ) ;
#26661 = EDGE_CURVE ( 'NONE', #27491, #14210, #44034, .T. ) ;
#26662 = CARTESIAN_POINT ( 'NONE',  ( 879.9999999999990905, 479.9999999999998863, 360.0000000000000000 ) ) ;
#26663 = CARTESIAN_POINT ( 'NONE',  ( 755.0488828828309806, -425.8055962898680491, -344.1219089521771934 ) ) ;
#26664 = CARTESIAN_POINT ( 'NONE',  ( 801.1904061080338124, -284.0891481129651197, -368.3070685750236066 ) ) ;
#26665 = CARTESIAN_POINT ( 'NONE',  ( 802.9823548866075953, -241.0999726633345119, 330.0799878456151077 ) ) ;
#26666 = DIRECTION ( 'NONE',  ( -1.000000000000000000, -0.000000000000000000, -0.000000000000000000 ) ) ;
#26667 = DIRECTION ( 'NONE',  ( 0.000000000000000000, 0.000000000000000000, -1.000000000000000000 ) ) ;
#26668 = CARTESIAN_POINT ( 'NONE',  ( 800.0135310231082713, -62.08914811296580183, -325.0180583372163028 ) ) ;
#26669 = CARTESIAN_POINT ( 'NONE',  ( 802.2119215644370342, -198.0090635724255606, 367.5423716828165084 ) ) ;
#26670 = CARTESIAN_POINT ( 'NONE',  ( 788.7631598425961101, -121.4419599262327267, -305.7194118038759143 ) ) ;
#26671 = CARTESIAN_POINT ( 'NONE',  ( 814.5518280994195948, -159.7255117493291436, 332.4837098697145734 ) ) ;
#26672 = CARTESIAN_POINT ( 'NONE',  ( 772.5602148656447525, -393.7255117493283478, -305.7998596910095443 ) ) ;
#26673 = ADVANCED_FACE ( 'NONE', ( #24849 ), #14925, .F. ) ;
#26674 = EDGE_CURVE ( 'NONE', #11542, #13265, #7765, .T. ) ;
#26675 = CARTESIAN_POINT ( 'NONE',  ( -784.4999999999993179, -365.3551492539851893, -8.132432514707076621 ) ) ;
#26676 = CARTESIAN_POINT ( 'NONE',  ( 765.0180583372156207, -240.9982390220561683, 360.0135310231089534 ) ) ;
#26677 = CARTESIAN_POINT ( 'NONE',  ( 779.4763451958990572, -8.736336299698871599, 365.0264073115438919 ) ) ;
#26678 = CARTESIAN_POINT ( 'NONE',  ( 804.6798772138708955, -399.7255117493283478, -334.6312213355107019 ) ) ;
#26679 = DIRECTION ( 'NONE',  ( -1.337618101958019798E-16, 1.000000000000000000, 1.672022627447524747E-16 ) ) ;
#26680 = CARTESIAN_POINT ( 'NONE',  ( 748.6759233522253680, -40.37269993606240348, -324.3348316497537098 ) ) ;
#26681 = LINE ( 'NONE', #19763, #26199 ) ;
#26682 = CARTESIAN_POINT ( 'NONE',  ( 795.9930595647434757, -99.07832356259642381, 320.7433823573372820 ) ) ;
#26683 = EDGE_LOOP ( 'NONE', ( #6207, #24843, #3995, #35612 ) ) ;
#26684 = CARTESIAN_POINT ( 'NONE',  ( 804.1601925771018387, -223.4419599262323857, -346.5483106153029098 ) ) ;
#26685 = CARTESIAN_POINT ( 'NONE',  ( 774.6858677611749044, -129.7255117493292289, -315.5713283507209894 ) ) ;
#26686 = CARTESIAN_POINT ( 'NONE',  ( 774.6858677611749044, -57.72551174932945628, 315.5713283507209894 ) ) ;
#26687 = AXIS2_PLACEMENT_3D ( 'NONE', #11584, #18514, #42534 ) ;
#26688 = CARTESIAN_POINT ( 'NONE',  ( 744.9990715423526808, -210.3510508353233490, -341.2370466360926002 ) ) ;
#26689 = CARTESIAN_POINT ( 'NONE',  ( 815.1787889125755555, -390.8965053807772279, 343.7953271457877804 ) ) ;
#26690 = ORIENTED_EDGE ( 'NONE', *, *, #17347, .T. ) ;
#26691 = CARTESIAN_POINT ( 'NONE',  ( 744.7301800767019131, -4.816420840238714085, 337.4774526936615757 ) ) ;
#26692 = ADVANCED_FACE ( 'NONE', ( #28783 ), #35696, .F. ) ;
#26693 = CARTESIAN_POINT ( 'NONE',  ( 771.2633955100217236, -167.9073299311473022, -363.4237431249939618 ) ) ;
#26694 = CARTESIAN_POINT ( 'NONE',  ( 805.1927285166397041, -376.8164208402375834, 341.8018195045277707 ) ) ;
#26695 = CARTESIAN_POINT ( 'NONE',  ( 787.5162901302840055, -83.36187538569296862, -305.4481719005792684 ) ) ;
#26696 = CARTESIAN_POINT ( 'NONE',  ( 764.8639956371174549, -80.08914811296574499, -319.7806653035542581 ) ) ;
#26697 = VERTEX_POINT ( 'NONE', #29244 ) ;
#26698 = CARTESIAN_POINT ( 'NONE',  ( 775.8780910478218402, -9.281790845153418346, -364.9511171171680530 ) ) ;
#26699 = VERTEX_POINT ( 'NONE', #21394 ) ;
#26700 = CARTESIAN_POINT ( 'NONE',  ( 796.1575198192839480, -366.0090635724250774, -359.4546378042384163 ) ) ;
#26702 = CARTESIAN_POINT ( 'NONE',  ( 755.5913626894240451, -397.6454272087885329, 346.6156483768012890 ) ) ;
#26701 = CARTESIAN_POINT ( 'NONE',  ( 758.0580252608178853, -78.45278447660211896, 328.0187753319985404 ) ) ;
#26705 = CARTESIAN_POINT ( 'NONE',  ( 778.7502325331095108, -312.3510508353230080, 304.6391490659818828 ) ) ;
#26704 = DIRECTION ( 'NONE',  ( -0.000000000000000000, -0.000000000000000000, 1.000000000000000000 ) ) ;
#26703 = CARTESIAN_POINT ( 'NONE',  ( 744.7301800767020268, -436.8164208402372992, 337.4774526936615189 ) ) ;
#26706 = CARTESIAN_POINT ( 'NONE',  ( 804.6971507214547046, -315.2817908451525000, -344.0799538623459739 ) ) ;
#26707 = CARTESIAN_POINT ( 'NONE',  ( 794.9819416627830151, -324.9982390220559409, -319.9864689768909898 ) ) ;
#26708 = CARTESIAN_POINT ( 'NONE',  ( 812.3518521366052028, -145.0999726633347677, -326.5853460496235243 ) ) ;
#26709 = CARTESIAN_POINT ( 'NONE',  ( 795.8262568251477660, 1.627300063937458408, 308.3538107759623585 ) ) ;
#26711 = CARTESIAN_POINT ( 'NONE',  ( -39.63011601220123481, -512.9681489794448908, -339.9999999999999432 ) ) ;
#26710 = CARTESIAN_POINT ( 'NONE',  ( 879.9999999999992042, 99.99999999999984368, -360.0000000000000000 ) ) ;
#26712 = EDGE_CURVE ( 'NONE', #22938, #2122, #42646, .T. ) ;
#26713 = CARTESIAN_POINT ( 'NONE',  ( 756.1348686366196716, -257.2601417444141134, -347.5531968255698416 ) ) ;
#26714 = CARTESIAN_POINT ( 'NONE',  ( 747.6481478633932056, -133.0999726633348246, -353.4146539503763620 ) ) ;
#26715 = DIRECTION ( 'NONE',  ( 0.000000000000000000, 0.3826834323650836756, 0.9238795325112892920 ) ) ;
#26716 = DIRECTION ( 'NONE',  ( 0.000000000000000000, 0.000000000000000000, -1.000000000000000000 ) ) ;
#26717 = CARTESIAN_POINT ( 'NONE',  ( 758.4439275373578084, -324.5545181178796952, 353.2243759319684386 ) ) ;
#26718 = ADVANCED_FACE ( 'NONE', ( #11456 ), #25540, .F. ) ;
#26719 = ORIENTED_EDGE ( 'NONE', *, *, #431, .T. ) ;
#26720 = CARTESIAN_POINT ( 'NONE',  ( 746.4236121716829757, -303.8272453906071178, 328.8385539511384650 ) ) ;
#26721 = CIRCLE ( 'NONE', #28950, 10.00000000000000888 ) ;
#26722 = CARTESIAN_POINT ( 'NONE',  ( 758.8095938919644823, -152.0891481129655460, -311.6929314249762797 ) ) ;
#26723 = CARTESIAN_POINT ( 'NONE',  ( 749.5768839229115201, -84.55451811788046257, 358.0661480581553064 ) ) ;
#26724 = CARTESIAN_POINT ( 'NONE',  ( 792.3570229623688874, -261.1800572038741848, -373.1304606946836202 ) ) ;
#26725 = CARTESIAN_POINT ( 'NONE',  ( 777.4774526936600978, -442.2709662947827383, -304.7301800767028226 ) ) ;
#26726 = CARTESIAN_POINT ( 'NONE',  ( 774.6312213355099630, -143.3618753856927697, 364.6798772138717482 ) ) ;
#26727 = EDGE_LOOP ( 'NONE', ( #28147, #40293, #45415, #19312, #31689, #28170, #8718, #23270, #13934, #18842, #4607 ) ) ;
#26728 = CARTESIAN_POINT ( 'NONE',  ( 752.4576283171824116, -357.0783235625956422, -317.7880784355627952 ) ) ;
#26729 = CARTESIAN_POINT ( 'NONE',  ( 777.5031285880264704, -94.81642084023843609, -374.9108240113588408 ) ) ;
#26730 = CARTESIAN_POINT ( 'NONE',  ( 801.5560724626406000, -48.55451811788057626, 326.7756240680316182 ) ) ;
#26731 = CARTESIAN_POINT ( 'NONE',  ( 751.6929314249748586, -342.9982390220557136, -318.8095938919659034 ) ) ;
#26732 = DIRECTION ( 'NONE',  ( -0.000000000000000000, 1.000000000000000000, -0.000000000000000000 ) ) ;
#26733 = CARTESIAN_POINT ( 'NONE',  ( 793.2243759319678702, -434.5328690171407970, 318.4439275373583200 ) ) ;
#26734 = VERTEX_POINT ( 'NONE', #15382 ) ;
#26735 = CONICAL_SURFACE ( 'NONE', #14197, 8.024999999999948841, 0.7853981633974337351 ) ;
#26736 = CARTESIAN_POINT ( 'NONE',  ( 748.3538107759620743, -112.7146871989600356, -355.8262568251490165 ) ) ;
#26737 = CARTESIAN_POINT ( 'NONE',  ( 311.1634899080286232, 240.0000000000000000, -197.2499999999964473 ) ) ;
#26738 = CARTESIAN_POINT ( 'NONE',  ( 756.1443688327750579, -261.6237781080504305, 314.3581564841659315 ) ) ;
#26739 = CARTESIAN_POINT ( 'NONE',  ( 774.6312213355098493, -95.36187538569296862, 364.6798772138717482 ) ) ;
#26740 = ORIENTED_EDGE ( 'NONE', *, *, #38540, .F. ) ;
#26741 = CARTESIAN_POINT ( 'NONE',  ( 790.8726784830453198, -10.71468719896033761, -362.5472867521010585 ) ) ;
#26742 = CARTESIAN_POINT ( 'NONE',  ( 791.9812246680005501, -284.6346026584196807, 361.9419747391813189 ) ) ;
#26743 = CARTESIAN_POINT ( 'NONE',  ( 808.7758568127978833, -436.1692326535044231, -320.0363995740631822 ) ) ;
#26744 = AXIS2_PLACEMENT_3D ( 'NONE', #14181, #31721, #42348 ) ;
#26745 = DIRECTION ( 'NONE',  ( 0.000000000000000000, 0.000000000000000000, -1.000000000000000000 ) ) ;
#26746 = ORIENTED_EDGE ( 'NONE', *, *, #37612, .F. ) ;
#26747 = EDGE_LOOP ( 'NONE', ( #488, #5217, #15129, #9375 ) ) ;
#26748 = CARTESIAN_POINT ( 'NONE',  ( 791.0478386215596629, -381.8272453906068336, -306.7653713866226326 ) ) ;
#26750 = CARTESIAN_POINT ( 'NONE',  ( 761.9338519418445230, -230.5328690171415076, 370.4231160770881957 ) ) ;
#26749 = CARTESIAN_POINT ( 'NONE',  ( 811.0346526505617248, -326.6346026584194533, 323.0537975583478101 ) ) ;
#26751 = CARTESIAN_POINT ( 'NONE',  ( 752.4576283171824116, -45.07832356259660145, 317.7880784355627952 ) ) ;
#26752 = CARTESIAN_POINT ( 'NONE',  ( 754.7162404726377645, -206.7363362996982801, -339.4709603349214717 ) ) ;
#26753 = CARTESIAN_POINT ( 'NONE',  ( 805.1927285166397041, -232.8164208402379245, -341.8018195045277707 ) ) ;
#26754 = CARTESIAN_POINT ( 'NONE',  ( 801.9419747391806368, -426.4527844766010389, -351.9812246680014027 ) ) ;
#26755 = ORIENTED_EDGE ( 'NONE', *, *, #25004, .F. ) ;
#26756 = CARTESIAN_POINT ( 'NONE',  ( 765.0180583372156207, -216.9982390220562252, 360.0135310231089534 ) ) ;
#26757 = CARTESIAN_POINT ( 'NONE',  ( 754.8072714833581358, -100.8164208402383792, -338.1981804954720587 ) ) ;
#26758 = ORIENTED_EDGE ( 'NONE', *, *, #12516, .T. ) ;
#26759 = DIRECTION ( 'NONE',  ( 1.000000000000000000, -1.880165489482579047E-16, 0.000000000000000000 ) ) ;
#26760 = CARTESIAN_POINT ( 'NONE',  ( 780.7518514355283514, 16.45630643248848912, 313.9393219192966740 ) ) ;
#26761 = CARTESIAN_POINT ( 'NONE',  ( -26.63011601220122060, -512.9681489794448908, -327.9999999999999432 ) ) ;
#26762 = CARTESIAN_POINT ( 'NONE',  ( 786.5483106153019435, -175.6454272087892718, 364.1601925771022366 ) ) ;
#26763 = CARTESIAN_POINT ( 'NONE',  ( 764.8639956371174549, -80.08914811296574499, 319.7806653035542013 ) ) ;
#26764 = ORIENTED_EDGE ( 'NONE', *, *, #28389, .F. ) ;
#26765 = CARTESIAN_POINT ( 'NONE',  ( 812.3518521366052028, -457.0999726633339151, -326.5853460496235243 ) ) ;
#26766 = VECTOR ( 'NONE', #23182, 1000.000000000000000 ) ;
#26767 = CARTESIAN_POINT ( 'NONE',  ( 801.1904061080338124, -44.08914811296585157, -368.3070685750236066 ) ) ;
#26768 = CARTESIAN_POINT ( 'NONE',  ( 802.7791456095903868, -268.7146871989595525, 329.0155153010375102 ) ) ;
#26769 = CARTESIAN_POINT ( 'NONE',  ( 791.9812246680005501, -404.6346026584193396, -361.9419747391813189 ) ) ;
#26770 = CARTESIAN_POINT ( 'NONE',  ( 788.8264449731201466, -21.18005720387502322, -363.6646147819170665 ) ) ;
#26771 = CARTESIAN_POINT ( 'NONE',  ( 805.0032342141412300, -445.5436935675098766, 314.9967657858571783 ) ) ;
#26772 = PLANE ( 'NONE',  #11481 ) ;
#26773 = CARTESIAN_POINT ( 'NONE',  ( 757.4527132478984868, -280.3726999360616787, -329.1273215169538844 ) ) ;
#26774 = CARTESIAN_POINT ( 'NONE',  ( 744.7301800767019131, -172.8164208402381234, -337.4774526936615757 ) ) ;
#26775 = CARTESIAN_POINT ( 'NONE',  ( 772.5602148656447525, -81.72551174932937101, 305.7998596910095443 ) ) ;
#26776 = CARTESIAN_POINT ( 'NONE',  ( 777.4774526936600978, -154.2709662947836478, 304.7301800767027657 ) ) ;
#26777 = CARTESIAN_POINT ( 'NONE',  ( 764.4978033197144214, 16.45630643248849267, -320.3127214678681867 ) ) ;
#26778 = DIRECTION ( 'NONE',  ( 0.000000000000000000, 0.000000000000000000, 1.000000000000000000 ) ) ;
#26779 = CARTESIAN_POINT ( 'NONE',  ( 758.0141637701419768, -231.0783235625960401, -367.2620300519063790 ) ) ;
#26780 = AXIS2_PLACEMENT_3D ( 'NONE', #22544, #39685, #36412 ) ;
#26781 = DIRECTION ( 'NONE',  ( 0.000000000000000000, 0.000000000000000000, 1.000000000000000000 ) ) ;
#26782 = CARTESIAN_POINT ( 'NONE',  ( 808.0189434323515343, -398.0891481129647218, 319.0252816721025511 ) ) ;
#26783 = CARTESIAN_POINT ( 'NONE',  ( 813.1304606946831655, -17.90732993114776406, 352.3570229623691716 ) ) ;
#26784 = CARTESIAN_POINT ( 'NONE',  ( 791.9812246680005501, -356.6346026584193964, -361.9419747391813189 ) ) ;
#26785 = CARTESIAN_POINT ( 'NONE',  ( 757.2208543904082489, 7.285312801039605546, 350.9844846989624330 ) ) ;
#26786 = CARTESIAN_POINT ( 'NONE',  ( 786.2694204179717872, -93.28179084515315367, -305.1769319972829067 ) ) ;
#26787 = CARTESIAN_POINT ( 'NONE',  ( 756.7813123517142913, -163.9874144716871456, -329.9779781133712504 ) ) ;
#26788 = CARTESIAN_POINT ( 'NONE',  ( 801.9858362298568863, -123.0783235625963385, 312.7379699480935642 ) ) ;
#26789 = DIRECTION ( 'NONE',  ( -1.000000000000000000, -0.000000000000000000, 0.000000000000000000 ) ) ;
#26790 = CARTESIAN_POINT ( 'NONE',  ( 803.6646147819161570, -65.90732993114758642, -348.8264449731210561 ) ) ;
#26791 = CARTESIAN_POINT ( 'NONE',  ( 793.2243759319678702, -170.5328690171416781, -318.4439275373583200 ) ) ;
#26792 = CARTESIAN_POINT ( 'NONE',  ( 788.8264449731200330, -117.1800572038746964, -363.6646147819171233 ) ) ;
#26793 = CARTESIAN_POINT ( 'NONE',  ( 804.6798772138708955, -159.7255117493291436, 334.6312213355107019 ) ) ;
#26794 = CARTESIAN_POINT ( 'NONE',  ( 752.4576283171824116, 2.921676437403253779, -317.7880784355627952 ) ) ;
#26795 = CARTESIAN_POINT ( 'NONE',  ( 762.1405469898973024, -289.5436935675105019, 357.8594530101016176 ) ) ;
#26796 = AXIS2_PLACEMENT_3D ( 'NONE', #39543, #10478, #13737 ) ;
#26797 = DIRECTION ( 'NONE',  ( -1.084653538143406060E-16, 0.6594541114781790059, -0.7517448203044204691 ) ) ;
#26798 = ORIENTED_EDGE ( 'NONE', *, *, #43362, .F. ) ;
#26799 = CARTESIAN_POINT ( 'NONE',  ( 799.4546378042377910, -33.07832356259662987, 356.1575198192848006 ) ) ;
#26800 = AXIS2_PLACEMENT_3D ( 'NONE', #4623, #11795, #15269 ) ;
#26801 = CARTESIAN_POINT ( 'NONE',  ( 754.3581564841646241, -257.4636090269708575, -316.1443688327762516 ) ) ;
#26802 = ORIENTED_EDGE ( 'NONE', *, *, #11170, .T. ) ;
#26803 = CARTESIAN_POINT ( 'NONE',  ( 811.0346526505617248, -230.6346026584197944, 323.0537975583478101 ) ) ;
#26804 = CARTESIAN_POINT ( 'NONE',  ( 755.3028492785439312, -303.2817908451525000, 335.9200461376539693 ) ) ;
#26805 = CARTESIAN_POINT ( 'NONE',  ( 795.9930595647434757, -411.0783235625954717, 320.7433823573372820 ) ) ;
#26806 = EDGE_LOOP ( 'NONE', ( #22441, #10366, #3132, #33771 ) ) ;
#26807 = CARTESIAN_POINT ( 'NONE',  ( 786.5483106153019435, -127.6454272087894140, -364.1601925771022366 ) ) ;
#26808 = CARTESIAN_POINT ( 'NONE',  ( 804.6798772138708955, -111.7255117493293000, -334.6312213355107019 ) ) ;
#26809 = CARTESIAN_POINT ( 'NONE',  ( 764.8639956371174549, -320.0891481129648923, -319.7806653035542581 ) ) ;
#26810 = ORIENTED_EDGE ( 'NONE', *, *, #33110, .T. ) ;
#26811 = CARTESIAN_POINT ( 'NONE',  ( 764.8639956371174549, -416.0891481129645513, -319.7806653035542013 ) ) ;
#26812 = CARTESIAN_POINT ( 'NONE',  ( 778.1981804954714335, -82.27096629478388934, -314.8072714833589885 ) ) ;
#26813 = AXIS2_PLACEMENT_3D ( 'NONE', #25161, #24937, #36473 ) ;
#26814 = CARTESIAN_POINT ( 'NONE',  ( 801.3366627262608972, -296.5328690171411949, 353.0897708529566899 ) ) ;
#26815 = DIRECTION ( 'NONE',  ( 0.000000000000000000, 1.000000000000000000, 1.110223024625155554E-15 ) ) ;
#26816 = CARTESIAN_POINT ( 'NONE',  ( -265.7583438952258916, -600.0000000000000000, -320.0000000000000000 ) ) ;
#26817 = CARTESIAN_POINT ( 'NONE',  ( -858.8365100919713768, 260.0000000000002274, -199.9999999999881481 ) ) ;
#26818 = ORIENTED_EDGE ( 'NONE', *, *, #24177, .F. ) ;
#26819 = CARTESIAN_POINT ( 'NONE',  ( 745.5313806188320314, -351.2817908451523294, -333.7943932421247268 ) ) ;
#26820 = CARTESIAN_POINT ( 'NONE',  ( 805.6418435158337843, -197.4636090269709996, 363.8556311672236916 ) ) ;
#26821 = CARTESIAN_POINT ( 'NONE',  ( 764.8639956371174549, -296.0891481129650629, -319.7806653035542013 ) ) ;
#26822 = CARTESIAN_POINT ( 'NONE',  ( -858.8365100919713768, 240.0000000000002274, -199.9999999999881481 ) ) ;
#26823 = CARTESIAN_POINT ( 'NONE',  ( 763.0428371773158460, -179.4636090269710849, -358.7617431975195359 ) ) ;
#26824 = CARTESIAN_POINT ( 'NONE',  ( 814.9108240113580450, -40.27096629478405987, 337.5031285880265273 ) ) ;
#26825 = DIRECTION ( 'NONE',  ( 0.000000000000000000, 0.000000000000000000, 1.000000000000000000 ) ) ;
#26826 = CARTESIAN_POINT ( 'NONE',  ( 813.1304606946831655, -377.9073299311465917, -352.3570229623691716 ) ) ;
#26827 = AXIS2_PLACEMENT_3D ( 'NONE', #22463, #4695, #36571 ) ;
#26828 = CARTESIAN_POINT ( 'NONE',  ( 927.9999999999992042, 219.9999999999998863, -350.0000000000000000 ) ) ;
#26829 = CARTESIAN_POINT ( 'NONE',  ( 774.6858677611749044, -57.72551174932945628, 315.5713283507209894 ) ) ;
#26830 = CARTESIAN_POINT ( 'NONE',  ( 781.2370466360911223, -308.7363362996979390, 304.9990715423533629 ) ) ;
#26831 = CARTESIAN_POINT ( 'NONE',  ( 815.2698199232961542, -280.8164208402378677, 342.5225473063383106 ) ) ;
#26832 = CARTESIAN_POINT ( 'NONE',  ( 767.6429770376289525, -33.18005720387498769, -306.8695393053162093 ) ) ;
#26833 = CARTESIAN_POINT ( 'NONE',  ( 781.7834795799800531, -250.8164208402379245, -315.0636971347436202 ) ) ;
#26834 = CARTESIAN_POINT ( 'NONE',  ( -190.7583438952259485, 394.6698570112193920, -274.9999999999999432 ) ) ;
#26835 = CARTESIAN_POINT ( 'NONE',  ( 758.0580252608178853, -366.4527844766012095, 328.0187753319985404 ) ) ;
#26836 = CARTESIAN_POINT ( 'NONE',  ( 805.2837595273609850, -122.7363362996985074, 340.5290396650784714 ) ) ;
#26837 = CARTESIAN_POINT ( 'NONE',  ( 796.7845633553578182, -33.62377810805116951, -358.5707757039688204 ) ) ;
#26838 = CARTESIAN_POINT ( 'NONE',  ( 748.3538107759620743, -40.71468719896024879, 355.8262568251490165 ) ) ;
#26839 = CARTESIAN_POINT ( 'NONE',  ( 785.3141322388236176, -357.7255117493285184, 364.4286716492789537 ) ) ;
#26840 = CARTESIAN_POINT ( 'NONE',  ( 187.1337867209877857, 50.81038600091411439, -193.6948738798775764 ) ) ;
#26841 = DIRECTION ( 'NONE',  ( 0.000000000000000000, 0.000000000000000000, -1.000000000000000000 ) ) ;
#26842 = CARTESIAN_POINT ( 'NONE',  ( 783.7566961878529810, -144.8965053807781089, 305.1792804349288417 ) ) ;
#26843 = CARTESIAN_POINT ( 'NONE',  ( 758.0580252608178853, -390.4527844766011526, 328.0187753319985404 ) ) ;
#26844 = ORIENTED_EDGE ( 'NONE', *, *, #28896, .T. ) ;
#26845 = VECTOR ( 'NONE', #45155, 1000.000000000000000 ) ;
#26846 = CARTESIAN_POINT ( 'NONE',  ( 795.9930595647434757, -339.0783235625956422, -320.7433823573372820 ) ) ;
#26848 = CARTESIAN_POINT ( 'NONE',  ( 803.4237431249931660, -183.1800572038744974, 331.2633955100225194 ) ) ;
#26847 = CARTESIAN_POINT ( 'NONE',  ( 774.6312213355099630, -191.3618753856925991, 364.6798772138717482 ) ) ;
#26849 = CARTESIAN_POINT ( 'NONE',  ( 795.6651683502461765, -370.7146871989592114, -371.3240766477733814 ) ) ;
#26850 = FACE_OUTER_BOUND ( 'NONE', #12770, .T. ) ;
#26851 = ORIENTED_EDGE ( 'NONE', *, *, #1846, .F. ) ;
#26852 = CARTESIAN_POINT ( 'NONE',  ( 797.8594530101008786, -373.5436935675101040, 322.1405469898980982 ) ) ;
#26853 = ORIENTED_EDGE ( 'NONE', *, *, #17668, .F. ) ;
#26854 = CARTESIAN_POINT ( 'NONE',  ( 748.9653473494363425, -218.6346026584197944, -356.9462024416521331 ) ) ;
#26855 = CARTESIAN_POINT ( 'NONE',  ( 763.2262854647970016, -128.6346026584201354, 309.2812353651462445 ) ) ;
#26856 = AXIS2_PLACEMENT_3D ( 'NONE', #25475, #36555, #1440 ) ;
#26857 = ORIENTED_EDGE ( 'NONE', *, *, #28572, .F. ) ;
#26858 = AXIS2_PLACEMENT_3D ( 'NONE', #23153, #34241, #6075 ) ;
#26859 = CARTESIAN_POINT ( 'NONE',  ( 756.5762568750052424, -171.1800572038745543, -348.7366044899774238 ) ) ;
#26860 = CIRCLE ( 'NONE', #24662, 19.99999999999990763 ) ;
#26861 = ORIENTED_EDGE ( 'NONE', *, *, #6037, .T. ) ;
#26862 = CARTESIAN_POINT ( 'NONE',  ( 762.1405469898971887, -337.5436935675102177, -357.8594530101015607 ) ) ;
#26863 = CARTESIAN_POINT ( 'NONE',  ( 792.1044303154645831, 11.54721552339760038, -317.8323909638837677 ) ) ;
#26864 = CARTESIAN_POINT ( 'NONE',  ( 782.5225473063381969, -238.2709662947833920, 375.2698199232970637 ) ) ;
#26865 = CARTESIAN_POINT ( 'NONE',  ( 776.9566956441375396, -180.8965053807779952, 364.8461984189686405 ) ) ;
#26867 = DIRECTION ( 'NONE',  ( -0.000000000000000000, -0.000000000000000000, 1.000000000000000000 ) ) ;
#26866 = CARTESIAN_POINT ( 'NONE',  ( 793.3938497862117174, -453.0432664090020580, 372.3358127763068524 ) ) ;
#26868 = EDGE_CURVE ( 'NONE', #19781, #24420, #30028, .T. ) ;
#26869 = CARTESIAN_POINT ( 'NONE',  ( -338.8365100919713200, 260.0000000000001137, -199.9999999999917861 ) ) ;
#26870 = ORIENTED_EDGE ( 'NONE', *, *, #42492, .F. ) ;
#26871 = CARTESIAN_POINT ( 'NONE',  ( 760.7433823573367135, -444.0090635724249069, -355.9930595647440441 ) ) ;
#26872 = DIRECTION ( 'NONE',  ( 0.000000000000000000, 1.000000000000000000, -0.000000000000000000 ) ) ;
#26873 = LINE ( 'NONE', #33359, #27021 ) ;
#26874 = ORIENTED_EDGE ( 'NONE', *, *, #17684, .F. ) ;
#26875 = CARTESIAN_POINT ( 'NONE',  ( 802.2119215644370342, -222.0090635724254184, -367.5423716828165084 ) ) ;
#26876 = AXIS2_PLACEMENT_3D ( 'NONE', #11805, #33268, #1614 ) ;
#26877 = CARTESIAN_POINT ( 'NONE',  ( 799.9636004259356241, -118.9181544815167229, 311.2241431872006956 ) ) ;
#26878 = AXIS2_PLACEMENT_3D ( 'NONE', #27425, #6422, #37826 ) ;
#26880 = CARTESIAN_POINT ( 'NONE',  ( 788.8264449731200330, -189.1800572038744122, -363.6646147819171233 ) ) ;
#26879 = CARTESIAN_POINT ( 'NONE',  ( -208.8365100919714052, 260.0000000000001137, -193.8809999999926674 ) ) ;
#26881 = CARTESIAN_POINT ( 'NONE',  ( 787.6308680596127942, -371.2601417444136587, -364.1105419155492768 ) ) ;
#26882 = CARTESIAN_POINT ( 'NONE',  ( 787.4999999999992042, -512.9681489794448908, 329.9999999999999432 ) ) ;
#26883 = CARTESIAN_POINT ( 'NONE',  ( 814.8207195650702488, -218.1908817542437191, -336.2433038121456548 ) ) ;
#26884 = CARTESIAN_POINT ( 'NONE',  ( -959.5497976682736407, 240.0000000000002274, 350.0000000000000000 ) ) ;
#26885 = LINE ( 'NONE', #9352, #9102 ) ;
#26886 = CARTESIAN_POINT ( 'NONE',  ( 790.9844846989617508, -70.37269993606230400, -317.2208543904092721 ) ) ;
#26887 = CARTESIAN_POINT ( 'NONE',  ( 775.8780910478218402, -441.2817908451521021, 364.9511171171680530 ) ) ;
#26888 = VECTOR ( 'NONE', #29200, 1000.000000000000114 ) ;
#26889 = DIRECTION ( 'NONE',  ( -1.000000000000000000, 0.000000000000000000, 0.000000000000000000 ) ) ;
#26890 = CARTESIAN_POINT ( 'NONE',  ( 804.9511171171677688, -437.8055962898679923, -335.8780910478229202 ) ) ;
#26891 = CARTESIAN_POINT ( 'NONE',  ( 777.5031285880264704, -262.8164208402379245, -374.9108240113588408 ) ) ;
#26892 = DIRECTION ( 'NONE',  ( -1.880165489482579047E-16, -1.000000000000000000, 0.000000000000000000 ) ) ;
#26893 = DIRECTION ( 'NONE',  ( 0.000000000000000000, 0.000000000000000000, -1.000000000000000000 ) ) ;
#26894 = CARTESIAN_POINT ( 'NONE',  ( 788.7366044899766848, -59.90732993114762905, -316.5762568750059813 ) ) ;
#26895 = CARTESIAN_POINT ( 'NONE',  ( 809.0717654672305343, -220.9181544815164102, 360.1688906516309885 ) ) ;
#26896 = CARTESIAN_POINT ( 'NONE',  ( 800.1688906516307043, -178.1692326535052473, -369.0717654672308186 ) ) ;
#26897 = CARTESIAN_POINT ( 'NONE',  ( 751.9810565676468741, -170.0891481129654608, 360.9747183278973921 ) ) ;
#26898 = CARTESIAN_POINT ( 'NONE',  ( 801.1904061080336987, -404.0891481129646081, -368.3070685750235498 ) ) ;
#26899 = CARTESIAN_POINT ( 'NONE',  ( 791.7608162188021197, 178.9475563372491251, -320.0000000000000000 ) ) ;
#26900 = CARTESIAN_POINT ( 'NONE',  ( 797.8594530101008786, -253.5436935675104735, 322.1405469898980982 ) ) ;
#26901 = AXIS2_PLACEMENT_3D ( 'NONE', #1403, #2077, #36958 ) ;
#26902 = CARTESIAN_POINT ( 'NONE',  ( 787.5531968255692163, -45.82724539060783542, 316.1348686366205811 ) ) ;
#26903 = CARTESIAN_POINT ( 'NONE',  ( 765.0180583372156207, -408.9982390220556567, -360.0135310231089534 ) ) ;
#26904 = VECTOR ( 'NONE', #35831, 1000.000000000000000 ) ;
#26905 = CYLINDRICAL_SURFACE ( 'NONE', #31350, 8.024999999999948841 ) ;
#26906 = DIRECTION ( 'NONE',  ( -1.000000000000000000, 0.000000000000000000, 0.000000000000000000 ) ) ;
#26907 = CARTESIAN_POINT ( 'NONE',  ( 764.0069404352550464, -87.07832356259646645, 359.2566176426627180 ) ) ;
#26908 = ORIENTED_EDGE ( 'NONE', *, *, #6356, .F. ) ;
#26909 = CARTESIAN_POINT ( 'NONE',  ( 805.1016975059191054, -222.8965053807778531, -343.0745993439771837 ) ) ;
#26910 = CARTESIAN_POINT ( 'NONE',  ( 765.0180583372156207, -72.99823902205667991, 360.0135310231089534 ) ) ;
#26912 = CARTESIAN_POINT ( 'NONE',  ( 749.8865473780648472, -260.5328690171413086, -322.1177392798429082 ) ) ;
#26911 = SHAPE_REPRESENTATION ( 'Slot', ( #26858 ), #21701 ) ;
#26913 = DIRECTION ( 'NONE',  ( -1.000000000000000000, -4.625929269271485914E-16, 0.000000000000000000 ) ) ;
#26914 = CARTESIAN_POINT ( 'NONE',  ( 748.3538107759620743, -376.7146871989592682, 355.8262568251490165 ) ) ;
#26915 = VERTEX_POINT ( 'NONE', #39875 ) ;
#26916 = VECTOR ( 'NONE', #29486, 1000.000000000000000 ) ;
#26917 = CARTESIAN_POINT ( 'NONE',  ( 758.8095938919642549, 15.91085188703394238, 311.6929314249763365 ) ) ;
#26918 = ADVANCED_FACE ( 'NONE', ( #4743 ), #32001, .T. ) ;
#26919 = CARTESIAN_POINT ( 'NONE',  ( 765.0180583372156207, -168.9982390220563673, -360.0135310231089534 ) ) ;
#26920 = CARTESIAN_POINT ( 'NONE',  ( 756.5762568750052424, -387.1800572038738437, 348.7366044899774238 ) ) ;
#26921 = VECTOR ( 'NONE', #37308, 1000.000000000000000 ) ;
#26922 = EDGE_CURVE ( 'NONE', #3205, #13375, #31523, .T. ) ;
#26923 = CARTESIAN_POINT ( 'NONE',  ( 815.2698199232961542, -112.8164208402383508, -342.5225473063383106 ) ) ;
#26924 = VECTOR ( 'NONE', #14928, 1000.000000000000000 ) ;
#26925 = CARTESIAN_POINT ( 'NONE',  ( 768.0187753319979720, -56.63460265842036279, -318.0580252608186242 ) ) ;
#26926 = ORIENTED_EDGE ( 'NONE', *, *, #40756, .T. ) ;
#26927 = CARTESIAN_POINT ( 'NONE',  ( 784.1219089521767955, -45.28179084515329578, -315.0488828828318333 ) ) ;
#26928 = CARTESIAN_POINT ( 'NONE',  ( 772.4468031744293057, -369.8272453906068904, -363.8651313633793620 ) ) ;
#26930 = CARTESIAN_POINT ( 'NONE',  ( 805.2837595273609850, -410.7363362996976548, 340.5290396650784714 ) ) ;
#26929 = CARTESIAN_POINT ( 'NONE',  ( 802.1676090361156639, -86.63460265842023489, 327.8955696845344505 ) ) ;
#26931 = CARTESIAN_POINT ( 'NONE',  ( 793.2243759319678702, -98.53286901714187707, 318.4439275373583200 ) ) ;
#26932 = EDGE_CURVE ( 'NONE', #1769, #42109, #11228, .T. ) ;
#26935 = CARTESIAN_POINT ( 'NONE',  ( 756.1443688327750579, -357.6237781080501463, 314.3581564841659315 ) ) ;
#26934 = LINE ( 'NONE', #40375, #28433 ) ;
#26933 = CARTESIAN_POINT ( 'NONE',  ( 782.4968714119720516, -442.8164208402372992, 305.0891759886411023 ) ) ;
#26936 = EDGE_CURVE ( 'NONE', #29224, #39697, #1996, .T. ) ;
#26937 = CIRCLE ( 'NONE', #43880, 2.749999999999919176 ) ;
#26938 = CARTESIAN_POINT ( 'NONE',  ( 793.0897708529556667, -318.5545181178796952, -361.3366627262616362 ) ) ;
#26939 = CARTESIAN_POINT ( 'NONE',  ( 757.8323909638827445, -314.6346026584194533, -352.1044303154654358 ) ) ;
#26940 = CARTESIAN_POINT ( 'NONE',  ( 805.6418435158337843, -149.4636090269711417, -363.8556311672236916 ) ) ;
#26941 = AXIS2_PLACEMENT_3D ( 'NONE', #44353, #37434, #2089 ) ;
#26942 = CARTESIAN_POINT ( 'NONE',  ( 802.2119215644370342, -6.009063572426154742, 367.5423716828165084 ) ) ;
#26943 = VECTOR ( 'NONE', #23004, 1000.000000000000000 ) ;
#26945 = CARTESIAN_POINT ( 'NONE',  ( -37.63011601220122770, -110.5936016518799221, 750.6326042729449455 ) ) ;
#26944 = DIRECTION ( 'NONE',  ( -1.000000000000000000, 0.000000000000000000, 0.000000000000000000 ) ) ;
#26946 = CARTESIAN_POINT ( 'NONE',  ( 801.3366627262608972, -272.5328690171413086, -353.0897708529566899 ) ) ;
#26947 = CARTESIAN_POINT ( 'NONE',  ( 766.4474001241216001, -115.0999726633348956, -307.3154664389482491 ) ) ;
#26948 = LINE ( 'NONE', #12865, #14548 ) ;
#26949 = CARTESIAN_POINT ( 'NONE',  ( 799.9999999999993179, -462.9681489794448339, -309.9999999999998863 ) ) ;
#26950 = VECTOR ( 'NONE', #34569, 1000.000000000000000 ) ;
#26951 = CARTESIAN_POINT ( 'NONE',  ( 769.0155153010367712, -346.3726999360614514, 362.7791456095907279 ) ) ;
#26952 = CARTESIAN_POINT ( 'NONE',  ( 767.8955696845333705, -192.4527844766016926, 362.1676090361162323 ) ) ;
#26953 = ORIENTED_EDGE ( 'NONE', *, *, #36529, .F. ) ;
#26954 = CARTESIAN_POINT ( 'NONE',  ( 766.4474001241216001, -307.0999726633343130, 307.3154664389482491 ) ) ;
#26955 = CARTESIAN_POINT ( 'NONE',  ( 796.7737145352015204, -164.6346026584200217, -370.7187646348536987 ) ) ;
#26956 = EDGE_CURVE ( 'NONE', #41099, #11148, #35936, .T. ) ;
#26957 = CARTESIAN_POINT ( 'NONE',  ( 759.0860845406687076, 19.76315572498245743, -318.4906424660488256 ) ) ;
#26958 = CARTESIAN_POINT ( 'NONE',  ( 809.0717654672305343, -100.9181544815167513, 360.1688906516309885 ) ) ;
#26959 = EDGE_CURVE ( 'NONE', #8042, #30282, #30129, .T. ) ;
#26960 = CARTESIAN_POINT ( 'NONE',  ( 758.8095938919642549, -296.0891481129650629, -311.6929314249763365 ) ) ;
#26961 = VECTOR ( 'NONE', #21131, 1000.000000000000114 ) ;
#26962 = CARTESIAN_POINT ( 'NONE',  ( 1820.038553321469863, 47.45399382421944523, -201.9999999999999432 ) ) ;
#26963 = PRODUCT ( 'Treadle Extension Return Springs', 'Treadle Extension Return Springs', '', ( #28597 ) ) ;
#26964 = CARTESIAN_POINT ( 'NONE',  ( 778.1981804954714335, -154.2709662947836478, 314.8072714833589885 ) ) ;
#26965 = ORIENTED_EDGE ( 'NONE', *, *, #45245, .T. ) ;
#26966 = CARTESIAN_POINT ( 'NONE',  ( 755.8990559732751535, -419.4636090269702891, 365.9055244015606831 ) ) ;
#26967 = CARTESIAN_POINT ( 'NONE',  ( 778.7502325331095108, -336.3510508353228943, -304.6391490659818828 ) ) ;
#26968 = CARTESIAN_POINT ( 'NONE',  ( 796.7737145352015204, -116.6346026584201780, -370.7187646348536987 ) ) ;
#26969 = CARTESIAN_POINT ( 'NONE',  ( 802.9823548866075953, -49.09997266333511590, 330.0799878456151077 ) ) ;
#26970 = CARTESIAN_POINT ( 'NONE',  ( 811.0346526505616112, -374.6346026584192828, -323.0537975583477532 ) ) ;
#26971 = CARTESIAN_POINT ( 'NONE',  ( 787.4999999999992042, -512.9681489794448908, 339.9999999999999432 ) ) ;
#26972 = CARTESIAN_POINT ( 'NONE',  ( 755.0488828828309806, -425.8055962898680491, 344.1219089521771934 ) ) ;
#26973 = EDGE_LOOP ( 'NONE', ( #12448, #3302, #175, #39761 ) ) ;
#26974 = AXIS2_PLACEMENT_3D ( 'NONE', #14173, #17420, #28727 ) ;
#26975 = ADVANCED_FACE ( 'NONE', ( #34042 ), #19738, .F. ) ;
#26976 = CARTESIAN_POINT ( 'NONE',  ( 773.7943932421234194, -167.8055962898689586, -305.5313806188329409 ) ) ;
#26977 = DIRECTION ( 'NONE',  ( 0.000000000000000000, -0.9235249282889854694, 0.3835384033298675499 ) ) ;
#26978 = CARTESIAN_POINT ( 'NONE',  ( 748.3538107759620743, -280.7146871989594956, 355.8262568251490165 ) ) ;
#26979 = CARTESIAN_POINT ( 'NONE',  ( 762.3223304703356007, -79.54369356751119824, 322.3223304703362828 ) ) ;
#26980 = ORIENTED_EDGE ( 'NONE', *, *, #5145, .T. ) ;
#26981 = VECTOR ( 'NONE', #18339, 1000.000000000000000 ) ;
#26982 = EDGE_CURVE ( 'NONE', #17925, #12399, #35210, .T. ) ;
#26983 = CARTESIAN_POINT ( 'NONE',  ( 760.5453621957607311, 2.921676437403253779, -323.8424801807151425 ) ) ;
#26984 = CARTESIAN_POINT ( 'NONE',  ( 800.0135310231082713, -254.0891481129652334, 325.0180583372163028 ) ) ;
#26985 = EDGE_CURVE ( 'NONE', #19341, #45642, #25972, .T. ) ;
#26986 = CARTESIAN_POINT ( 'NONE',  ( 815.1787889125755555, -438.8965053807771710, -343.7953271457877804 ) ) ;
#26987 = LINE ( 'NONE', #30220, #9190 ) ;
#26988 = ORIENTED_EDGE ( 'NONE', *, *, #23239, .F. ) ;
#26989 = EDGE_LOOP ( 'NONE', ( #25581, #41755, #33144, #32123 ) ) ;
#26990 = CARTESIAN_POINT ( 'NONE',  ( 813.5763878283155464, -363.8272453906068336, -351.1614460488615350 ) ) ;
#26991 = AXIS2_PLACEMENT_3D ( 'NONE', #2145, #44407, #36805 ) ;
#26992 = EDGE_CURVE ( 'NONE', #15857, #33458, #44440, .T. ) ;
#26993 = AXIS2_PLACEMENT_3D ( 'NONE', #27618, #41489, #34559 ) ;
#26995 = CARTESIAN_POINT ( 'NONE',  ( 746.7653713866222915, -209.2601417444142839, 351.0478386215610271 ) ) ;
#26994 = CARTESIAN_POINT ( 'NONE',  ( 755.2512626584698410, -319.5436935675104451, 315.2512626584710915 ) ) ;
#26996 = CARTESIAN_POINT ( 'NONE',  ( 815.1787889125755555, -54.89650538077837183, 343.7953271457877804 ) ) ;
#26997 = CARTESIAN_POINT ( 'NONE',  ( 775.8780910478218402, -225.2817908451527273, -364.9511171171680530 ) ) ;
#26998 = CARTESIAN_POINT ( 'NONE',  ( 778.1981804954714335, -226.2709662947834204, -314.8072714833589885 ) ) ;
#26999 = CARTESIAN_POINT ( 'NONE',  ( 756.5762568750052424, -411.1800572038738437, -348.7366044899774238 ) ) ;
#27000 = EDGE_LOOP ( 'NONE', ( #6431, #26965, #30666, #11925 ) ) ;
#27001 = CARTESIAN_POINT ( 'NONE',  ( 774.6858677611749044, -201.7255117493290015, 315.5713283507209894 ) ) ;
#27002 = CARTESIAN_POINT ( 'NONE',  ( 774.6312213355099630, -95.36187538569294020, -364.6798772138717482 ) ) ;
#27003 = ORIENTED_EDGE ( 'NONE', *, *, #24646, .F. ) ;
#27004 = CARTESIAN_POINT ( 'NONE',  ( 808.0189434323515343, -350.0891481129648923, 319.0252816721025511 ) ) ;
#27005 = CARTESIAN_POINT ( 'NONE',  ( 799.9999999999993179, -365.3551492539851893, 18.13243251470705886 ) ) ;
#27006 = CARTESIAN_POINT ( 'NONE',  ( 776.3558828440975503, 16.45630643248848557, 314.5934542695748064 ) ) ;
#27007 = PLANE ( 'NONE',  #24492 ) ;
#27008 = CARTESIAN_POINT ( 'NONE',  ( 766.9102291470427417, -210.5545181178800647, 318.6633372737382501 ) ) ;
#27009 = CARTESIAN_POINT ( 'NONE',  ( 762.1405469898971887, -97.54369356751112718, 357.8594530101015607 ) ) ;
#27010 = ORIENTED_EDGE ( 'NONE', *, *, #43384, .F. ) ;
#27011 = CARTESIAN_POINT ( 'NONE',  ( 815.3608509340175488, -458.7363362996973706, -341.2497674668889545 ) ) ;
#27012 = CARTESIAN_POINT ( 'NONE',  ( 751.9810565676468741, -74.08914811296577341, -360.9747183278973921 ) ) ;
#27013 = CARTESIAN_POINT ( 'NONE',  ( 799.4546378042377910, -273.0783235625958696, 356.1575198192848006 ) ) ;
#27014 = VECTOR ( 'NONE', #14647, 1000.000000000000000 ) ;
#27015 = CARTESIAN_POINT ( 'NONE',  ( 757.8323909638827445, -434.6346026584190554, -352.1044303154654358 ) ) ;
#27016 = CARTESIAN_POINT ( 'NONE',  ( 759.7806653035535192, -30.99823902205680781, -324.8639956371181370 ) ) ;
#27017 = CARTESIAN_POINT ( 'NONE',  ( 796.7737145352015204, -452.6346026584191691, 370.7187646348536987 ) ) ;
#27018 = CARTESIAN_POINT ( 'NONE',  ( 804.9363028652555840, 7.729033705215793582, -338.2165204200192079 ) ) ;
#27019 = CARTESIAN_POINT ( 'NONE',  ( 786.5483106153019435, -295.6454272087888739, -364.1601925771022366 ) ) ;
#27021 = VECTOR ( 'NONE', #33590, 1000.000000000000000 ) ;
#27020 = CARTESIAN_POINT ( 'NONE',  ( 804.7487373415286811, -187.5436935675108430, -364.7487373415288516 ) ) ;
#27022 = CARTESIAN_POINT ( 'NONE',  ( 787.4397851343537695, -93.72551174932934259, 374.2001403089903988 ) ) ;
#27023 = CARTESIAN_POINT ( 'NONE',  ( 767.6429770376289525, -153.1800572038746395, 306.8695393053162093 ) ) ;
#27024 = CARTESIAN_POINT ( 'NONE',  ( 989.9999999999992042, -407.8586036264140375, -201.9999999999998863 ) ) ;
#27025 = CARTESIAN_POINT ( 'NONE',  ( 879.9999999999990905, 479.9999999999998863, 199.9999999999999716 ) ) ;
#27026 = CARTESIAN_POINT ( 'NONE',  ( 752.4576283171824116, -237.0783235625960117, -317.7880784355627952 ) ) ;
#27027 = CARTESIAN_POINT ( 'NONE',  ( 781.2370466360911223, -404.7363362996975980, 304.9990715423533629 ) ) ;
#27028 = CARTESIAN_POINT ( 'NONE',  ( 767.6429770376289525, -297.1800572038740711, -306.8695393053162093 ) ) ;
#27029 = CARTESIAN_POINT ( 'NONE',  ( -775.4999999999993179, -365.3551492539851893, -28.13243251470704109 ) ) ;
#27030 = CARTESIAN_POINT ( 'NONE',  ( 796.7737145352015204, -380.6346026584192828, 370.7187646348536987 ) ) ;
#27031 = CARTESIAN_POINT ( 'NONE',  ( 763.0537975583476964, -0.4527844766023629286, 371.0346526505628617 ) ) ;
#27032 = CARTESIAN_POINT ( 'NONE',  ( 767.8955696845333705, -336.4527844766012095, -362.1676090361162323 ) ) ;
#27033 = AXIS2_PLACEMENT_3D ( 'NONE', #2979, #10359, #39016 ) ;
#27034 = CARTESIAN_POINT ( 'NONE',  ( 800.7704444035546203, -4.169232653505813069, 326.0291762391768771 ) ) ;
#27035 = CARTESIAN_POINT ( 'NONE',  ( 810.4231160770870019, -96.55451811788039151, -321.9338519418446936 ) ) ;
#27036 = CARTESIAN_POINT ( 'NONE',  ( 765.8855110935204493, -166.1692326535053041, -319.0159684113471599 ) ) ;
#27037 = CARTESIAN_POINT ( 'NONE',  ( 786.2056067578752163, -155.8055962898689586, 374.4686193811670023 ) ) ;
#27038 = CARTESIAN_POINT ( 'NONE',  ( 797.8594530101009923, 10.45630643248851044, 322.1405469898982119 ) ) ;
#27039 = CARTESIAN_POINT ( 'NONE',  ( 813.2346286133761168, -173.2601417444143692, 328.9521613784389160 ) ) ;
#27040 = ORIENTED_EDGE ( 'NONE', *, *, #10062, .T. ) ;
#27041 = CARTESIAN_POINT ( 'NONE',  ( 767.8955696845333705, -48.45278447660219712, -362.1676090361162323 ) ) ;
#27042 = CARTESIAN_POINT ( 'NONE',  ( 805.0264073115434940, -150.3510508353235480, -339.4763451958999099 ) ) ;
#27043 = CARTESIAN_POINT ( 'NONE',  ( 797.8594530101008786, -181.5436935675108145, 322.1405469898980982 ) ) ;
#27044 = CARTESIAN_POINT ( 'NONE',  ( 776.2433038121456548, -12.89650538077851216, -374.8207195650711014 ) ) ;
#27046 = CARTESIAN_POINT ( 'NONE',  ( 788.8264449731201466, -309.1800572038740711, 363.6646147819170665 ) ) ;
#27045 = CARTESIAN_POINT ( 'NONE',  ( 771.2633955100217236, -287.9073299311468759, 363.4237431249939618 ) ) ;
#27047 = CARTESIAN_POINT ( 'NONE',  ( -858.8365100919713768, 260.0000000000002274, -199.9999999999881481 ) ) ;
#27048 = EDGE_LOOP ( 'NONE', ( #42471, #17566, #27692, #15307 ) ) ;
#27049 = CARTESIAN_POINT ( 'NONE',  ( 755.8398074228967971, -19.44195992623303937, 333.4516893846970333 ) ) ;
#27051 = CIRCLE ( 'NONE', #18950, 10.00000000000000888 ) ;
#27050 = CARTESIAN_POINT ( 'NONE',  ( 776.2046728542105711, -284.1908817542434917, -304.8212110874238761 ) ) ;
#27052 = CIRCLE ( 'NONE', #7153, 2.749999999999919176 ) ;
#27053 = ORIENTED_EDGE ( 'NONE', *, *, #3388, .T. ) ;
#27054 = DIRECTION ( 'NONE',  ( 1.000000000000000000, 0.000000000000000000, 0.000000000000000000 ) ) ;
#27055 = VECTOR ( 'NONE', #18907, 1000.000000000000000 ) ;
#27056 = CARTESIAN_POINT ( 'NONE',  ( 805.0032342141413437, -229.5436935675107009, 314.9967657858572352 ) ) ;
#27057 = CARTESIAN_POINT ( 'NONE',  ( 773.4516893846965786, -307.6454272087888171, 315.8398074228977066 ) ) ;
#27058 = CARTESIAN_POINT ( 'NONE',  ( 795.9930595647434757, -435.0783235625953580, 320.7433823573372820 ) ) ;
#27059 = ORIENTED_EDGE ( 'NONE', *, *, #11177, .T. ) ;
#27061 = VECTOR ( 'NONE', #19795, 999.9999999999998863 ) ;
#27060 = CARTESIAN_POINT ( 'NONE',  ( 796.9571628226829034, -119.4636090269712554, -321.2382568024804641 ) ) ;
#27062 = CARTESIAN_POINT ( 'NONE',  ( 762.1405469898971887, -97.54369356751112718, -357.8594530101015607 ) ) ;
#27063 = CARTESIAN_POINT ( 'NONE',  ( 800.2193346964446619, -330.9982390220558273, -355.1360043628816925 ) ) ;
#27064 = ORIENTED_EDGE ( 'NONE', *, *, #25106, .T. ) ;
#27065 = CARTESIAN_POINT ( 'NONE',  ( 759.9864689768902508, -434.0891481129646081, -354.9819416627836404 ) ) ;
#27066 = VECTOR ( 'NONE', #4001, 1000.000000000000000 ) ;
#27067 = CARTESIAN_POINT ( 'NONE',  ( 775.9200461376533440, -311.8055962898685038, 315.3028492785443291 ) ) ;
#27068 = CARTESIAN_POINT ( 'NONE',  ( 792.0613484971601110, -458.0032201311295807, 367.4685979341032294 ) ) ;
#27069 = CARTESIAN_POINT ( 'NONE',  ( -858.8365100919713768, 260.0000000000002274, -199.9999999999881481 ) ) ;
#27070 = CIRCLE ( 'NONE', #41084, 19.99999999999990763 ) ;
#27071 = CARTESIAN_POINT ( 'NONE',  ( 755.5913626894240451, -109.6454272087894566, 346.6156483768012890 ) ) ;
#27072 = LINE ( 'NONE', #37219, #28539 ) ;
#27073 = VERTEX_POINT ( 'NONE', #19497 ) ;
#27074 = CARTESIAN_POINT ( 'NONE',  ( 814.2805881961230625, -337.6454272087888171, -331.2368401574024119 ) ) ;
#27075 = CARTESIAN_POINT ( 'NONE',  ( 774.6312213355099630, -335.3618753856920307, -364.6798772138717482 ) ) ;
#27076 = CARTESIAN_POINT ( 'NONE',  ( 200.7583438952258916, 294.6698570112193920, -244.9999999999999716 ) ) ;
#27077 = CARTESIAN_POINT ( 'NONE',  ( 757.4527132478984868, -184.3726999360619629, -329.1273215169538844 ) ) ;
#27078 = CARTESIAN_POINT ( 'NONE',  ( 746.8695393053150156, -29.90732993114771787, 327.6429770376306010 ) ) ;
#27079 = CARTESIAN_POINT ( 'NONE',  ( -784.4999999999993179, -857.0166862835568509, -63.94525337997358605 ) ) ;
#27080 = CARTESIAN_POINT ( 'NONE',  ( 787.4397851343537695, -381.7255117493284615, -374.2001403089903988 ) ) ;
#27081 = CARTESIAN_POINT ( 'NONE',  ( 799.9999999999993179, -512.9681489794448908, 309.9999999999998863 ) ) ;
#27082 = CARTESIAN_POINT ( 'NONE',  ( 791.0478386215596629, -333.8272453906070041, 306.7653713866226326 ) ) ;
#27083 = CARTESIAN_POINT ( 'NONE',  ( 794.9999999999993179, 240.0000000000000568, -244.9999999999999716 ) ) ;
#27084 = CARTESIAN_POINT ( 'NONE',  ( 751.6929314249748586, -294.9982390220560546, 318.8095938919659034 ) ) ;
#27085 = CARTESIAN_POINT ( 'NONE',  ( 745.7998596910086917, -5.361875385693257279, -332.5602148656461168 ) ) ;
#27086 = VECTOR ( 'NONE', #32532, 1000.000000000000000 ) ;
#27087 = CARTESIAN_POINT ( 'NONE',  ( 805.1927285166397041, -256.8164208402379245, -341.8018195045277707 ) ) ;
#27088 = CARTESIAN_POINT ( 'NONE',  ( 919.9999999999993179, 219.9999999999998863, -350.0000000000000000 ) ) ;
#27089 = CARTESIAN_POINT ( 'NONE',  ( 755.5713283507202505, -389.3618753856919739, 334.6858677611754729 ) ) ;
#27090 = CARTESIAN_POINT ( 'NONE',  ( 769.0155153010367712, -130.3726999360621619, 362.7791456095907279 ) ) ;
#27091 = CARTESIAN_POINT ( 'NONE',  ( 799.4546378042377910, -33.07832356259662987, -356.1575198192848006 ) ) ;
#27092 = CARTESIAN_POINT ( 'NONE',  ( 793.4146539503750546, -49.98741447168749374, 307.6481478633938877 ) ) ;
#27093 = CARTESIAN_POINT ( 'NONE',  ( 781.7834795799800531, -370.8164208402375834, 315.0636971347436202 ) ) ;
#27094 = CIRCLE ( 'NONE', #2023, 20.00000000000004619 ) ;
#27095 = LINE ( 'NONE', #16702, #33587 ) ;
#27096 = CARTESIAN_POINT ( 'NONE',  ( 799.9999999999993179, -357.6843811873878280, -0.3380660510726891665 ) ) ;
#27097 = CARTESIAN_POINT ( 'NONE',  ( 768.8385539511368734, -143.2601417444144829, 306.4236121716840557 ) ) ;
#27098 = CARTESIAN_POINT ( 'NONE',  ( 792.1044303154645831, -444.4527844766009821, 317.8323909638837677 ) ) ;
#27099 = ORIENTED_EDGE ( 'NONE', *, *, #36083, .T. ) ;
#27100 = CARTESIAN_POINT ( 'NONE',  ( 804.6798772138708955, -63.72551174932939233, -334.6312213355107019 ) ) ;
#27101 = CARTESIAN_POINT ( 'NONE',  ( 776.9566956441375396, -348.8965053807774552, -364.8461984189686405 ) ) ;
#27103 = CARTESIAN_POINT ( 'NONE',  ( 774.6312213355098493, -191.3618753856926276, 364.6798772138717482 ) ) ;
#27102 = CARTESIAN_POINT ( 'NONE',  ( 778.2165204200184689, -190.8164208402381234, 364.9363028652563230 ) ) ;
#27104 = CARTESIAN_POINT ( 'NONE',  ( 791.1614460488616487, -371.2601417444136587, -373.5763878283158874 ) ) ;
#27105 = CARTESIAN_POINT ( 'NONE',  ( -786.4999999999993179, -110.5936016518799221, 750.6326042729449455 ) ) ;
#27106 = ORIENTED_EDGE ( 'NONE', *, *, #7243, .T. ) ;
#27107 = CARTESIAN_POINT ( 'NONE',  ( 800.2193346964447755, -378.9982390220555999, 355.1360043628815788 ) ) ;
#27108 = ORIENTED_EDGE ( 'NONE', *, *, #45675, .T. ) ;
#27109 = CYLINDRICAL_SURFACE ( 'NONE', #34985, 2.749999999999835687 ) ;
#27110 = CARTESIAN_POINT ( 'NONE',  ( 796.9462024416508257, -204.4527844766016926, -308.9653473494370246 ) ) ;
#27111 = CARTESIAN_POINT ( 'NONE',  ( 744.7301800767020268, -124.8164208402383366, 337.4774526936615189 ) ) ;
#27112 = EDGE_LOOP ( 'NONE', ( #33138, #4415, #18214, #24633 ) ) ;
#27113 = CARTESIAN_POINT ( 'NONE',  ( 755.5713283507202505, -221.3618753856925707, -334.6858677611754729 ) ) ;
#27114 = ORIENTED_EDGE ( 'NONE', *, *, #7247, .T. ) ;
#27115 = CARTESIAN_POINT ( 'NONE',  ( 762.3223304703356007, -319.5436935675104451, -322.3223304703362828 ) ) ;
#27116 = CARTESIAN_POINT ( 'NONE',  ( 755.1538015810308480, -446.1908817542429802, -343.0433043558613804 ) ) ;
#27117 = CARTESIAN_POINT ( 'NONE',  ( 796.7737145352015204, -260.6346026584197375, 370.7187646348536987 ) ) ;
#27118 = CARTESIAN_POINT ( 'NONE',  ( 801.3366627262608972, -200.5328690171415644, 353.0897708529566899 ) ) ;
#27120 = DIRECTION ( 'NONE',  ( -1.000000000000000000, -0.000000000000000000, -0.000000000000000000 ) ) ;
#27119 = DIRECTION ( 'NONE',  ( 0.000000000000000000, 0.000000000000000000, 1.000000000000000000 ) ) ;
#27121 = DIRECTION ( 'NONE',  ( -1.000000000000000000, 0.000000000000000000, 0.000000000000000000 ) ) ;
#27122 = EDGE_LOOP ( 'NONE', ( #12009, #7117, #4170, #17408 ) ) ;
#27123 = CARTESIAN_POINT ( 'NONE',  ( 804.4086373105744769, -457.6454272087884760, -333.3843516231986541 ) ) ;
#27124 = DIRECTION ( 'NONE',  ( 0.000000000000000000, 0.000000000000000000, 1.000000000000000000 ) ) ;
#27125 = CARTESIAN_POINT ( 'NONE',  ( 989.9999999999992042, 62.85347435602256638, 357.4246812887967053 ) ) ;
#27126 = VERTEX_POINT ( 'NONE', #33594 ) ;
#27127 = CARTESIAN_POINT ( 'NONE',  ( 744.6391490659812007, -230.7363362996981664, -338.7502325331110455 ) ) ;
#27128 = CARTESIAN_POINT ( 'NONE',  ( 771.3260364891663130, -91.64542720878951343, 306.0683387631859773 ) ) ;
#27129 = AXIS2_PLACEMENT_3D ( 'NONE', #288, #42783, #11145 ) ;
#27131 = CARTESIAN_POINT ( 'NONE',  ( 759.7806653035534055, -198.9982390220562252, -324.8639956371180801 ) ) ;
#27130 = CARTESIAN_POINT ( 'NONE',  ( 115.7583438952258774, 430.0000000000002842, -320.0000000000000568 ) ) ;
#27132 = CARTESIAN_POINT ( 'NONE',  ( 763.2154366446407039, -357.6237781080501463, -321.4292242960311228 ) ) ;
#27133 = CARTESIAN_POINT ( 'NONE',  ( 802.2119215644370342, -246.0090635724253900, -367.5423716828165084 ) ) ;
#27134 = CARTESIAN_POINT ( 'NONE',  ( 999.9999999999992042, 478.9999999999999432, -200.9999999999999432 ) ) ;
#27135 = CARTESIAN_POINT ( 'NONE',  ( 999.9999999999992042, 249.5857864376267798, 200.4142135623730496 ) ) ;
#27136 = CARTESIAN_POINT ( 'NONE',  ( 766.9102291470427417, -66.55451811788050520, -318.6633372737382501 ) ) ;
#27137 = CARTESIAN_POINT ( 'NONE',  ( 772.4468031744293057, -441.8272453906066630, 363.8651313633793620 ) ) ;
#27138 = CARTESIAN_POINT ( 'NONE',  ( 804.1009440267234822, -359.4636090269705164, 314.0944755984392600 ) ) ;
#27139 = FACE_BOUND ( 'NONE', #22947, .T. ) ;
#27140 = CARTESIAN_POINT ( 'NONE',  ( 803.2186876482843445, -439.9874144716862929, -350.0220218866286928 ) ) ;
#27141 = CARTESIAN_POINT ( 'NONE',  ( 812.7932403749906598, -279.1800572038741848, -327.7687537140311633 ) ) ;
#27142 = CARTESIAN_POINT ( 'NONE',  ( 786.4999999999993179, -512.9681489794448908, -350.0000000000000000 ) ) ;
#27143 = DIRECTION ( 'NONE',  ( 0.000000000000000000, 0.000000000000000000, 1.000000000000000000 ) ) ;
#27144 = CARTESIAN_POINT ( 'NONE',  ( 774.6858677611749044, -33.72551174932952733, -315.5713283507209894 ) ) ;
#27145 = CARTESIAN_POINT ( 'NONE',  ( 795.8262568251477660, -214.3726999360618493, 308.3538107759623585 ) ) ;
#27146 = CARTESIAN_POINT ( 'NONE',  ( 781.2497674668890113, -156.3510508353235480, -375.3608509340180603 ) ) ;
#27147 = CARTESIAN_POINT ( 'NONE',  ( 814.5518280994195948, -183.7255117493290015, 332.4837098697145734 ) ) ;
#27148 = CARTESIAN_POINT ( 'NONE',  ( 815.2698199232961542, -424.8164208402372992, -342.5225473063383106 ) ) ;
#27149 = FACE_OUTER_BOUND ( 'NONE', #19997, .T. ) ;
#27150 = CARTESIAN_POINT ( 'NONE',  ( 803.4237431249931660, -255.1800572038742700, 331.2633955100225194 ) ) ;
#27151 = CARTESIAN_POINT ( 'NONE',  ( 766.0291762391763086, -58.91815448151690759, 360.7704444035551319 ) ) ;
#27152 = CARTESIAN_POINT ( 'NONE',  ( 781.8018195045266339, -430.2709662947827383, -365.1927285166406705 ) ) ;
#27153 = DIRECTION ( 'NONE',  ( 0.000000000000000000, -1.000000000000000000, -0.000000000000000000 ) ) ;
#27154 = PLANE ( 'NONE',  #36522 ) ;
#27156 = CARTESIAN_POINT ( 'NONE',  ( 791.9812246680005501, -308.6346026584195670, 361.9419747391813189 ) ) ;
#27155 = CARTESIAN_POINT ( 'NONE',  ( 761.2382568024794409, -87.62377810805102740, 356.9571628226838129 ) ) ;
#27157 = VERTEX_POINT ( 'NONE', #2178 ) ;
#27158 = EDGE_CURVE ( 'NONE', #12219, #40969, #15311, .T. ) ;
#27159 = CARTESIAN_POINT ( 'NONE',  ( 755.0488828828309806, -257.8055962898686744, -344.1219089521771934 ) ) ;
#27160 = CARTESIAN_POINT ( 'NONE',  ( 791.9812246680005501, -68.63460265842033436, 361.9419747391813189 ) ) ;
#27161 = CARTESIAN_POINT ( 'NONE',  ( 776.2433038121456548, -252.8965053807777394, -374.8207195650711014 ) ) ;
#27162 = DIRECTION ( 'NONE',  ( -0.000000000000000000, 0.000000000000000000, 1.000000000000000000 ) ) ;
#27163 = CARTESIAN_POINT ( 'NONE',  ( 783.7566961878529810, -384.8965053807772847, 305.1792804349288417 ) ) ;
#27164 = EDGE_LOOP ( 'NONE', ( #7051, #37387, #6765, #35792 ) ) ;
#27165 = CARTESIAN_POINT ( 'NONE',  ( 803.6646147819161570, -305.9073299311467622, 348.8264449731210561 ) ) ;
#27166 = CARTESIAN_POINT ( 'NONE',  ( 803.8556311672234642, -441.6237781080499190, 365.6418435158340117 ) ) ;
#27167 = CARTESIAN_POINT ( 'NONE',  ( 769.1273215169530886, -22.71468719896029853, -317.4527132478988847 ) ) ;
#27168 = CARTESIAN_POINT ( 'NONE',  ( 804.6798772138708955, -183.7255117493290015, -334.6312213355107019 ) ) ;
#27169 = CARTESIAN_POINT ( 'NONE',  ( 804.9363028652555840, -376.2709662947829656, 338.2165204200192079 ) ) ;
#27170 = CARTESIAN_POINT ( 'NONE',  ( 808.0189434323515343, -110.0891481129656597, -319.0252816721025511 ) ) ;
#27171 = CARTESIAN_POINT ( 'NONE',  ( 803.4237431249931660, -111.1800572038747532, -331.2633955100225194 ) ) ;
#27172 = VERTEX_POINT ( 'NONE', #33825 ) ;
#27173 = CARTESIAN_POINT ( 'NONE',  ( 783.0745993439762742, -32.19088175424425913, -365.1016975059196739 ) ) ;
#27174 = CARTESIAN_POINT ( 'NONE',  ( 755.8894580844503253, -351.8272453906068336, -332.3691319403863531 ) ) ;
#27176 = CARTESIAN_POINT ( 'NONE',  ( 766.0291762391763086, -394.9181544815158418, 360.7704444035551319 ) ) ;
#27175 = CARTESIAN_POINT ( 'NONE',  ( 805.1927285166397041, -88.81642084023842187, 341.8018195045277707 ) ) ;
#27177 = CARTESIAN_POINT ( 'NONE',  ( 805.1016975059191054, -102.8965053807782368, 343.0745993439771837 ) ) ;
#27180 = CARTESIAN_POINT ( 'NONE',  ( 810.1134526219336749, -344.5328690171410813, 357.8822607201570349 ) ) ;
#27179 = DIRECTION ( 'NONE',  ( -1.000000000000000000, -0.000000000000000000, 0.000000000000000000 ) ) ;
#27178 = CARTESIAN_POINT ( 'NONE',  ( -784.4999999999993179, -563.3203001761231690, -342.3463313526983143 ) ) ;
#27181 = EDGE_CURVE ( 'NONE', #38147, #29157, #4975, .T. ) ;
#27182 = CARTESIAN_POINT ( 'NONE',  ( 779.4763451958990572, -368.7363362996977685, -365.0264073115438919 ) ) ;
#27183 = CARTESIAN_POINT ( 'NONE',  ( 765.0180583372156207, -336.9982390220558273, -360.0135310231089534 ) ) ;
#27184 = CARTESIAN_POINT ( 'NONE',  ( 786.2694204179717872, -117.2817908451530684, -305.1769319972829067 ) ) ;
#27185 = CARTESIAN_POINT ( 'NONE',  ( 754.3581564841646241, 6.536390973028352924, 316.1443688327762516 ) ) ;
#27186 = CARTESIAN_POINT ( 'NONE',  ( -338.8365100919713200, 260.0000000000001137, -199.9999999999917861 ) ) ;
#27187 = CARTESIAN_POINT ( 'NONE',  ( 814.4686193811664907, -123.2817908451530542, -346.2056067578752732 ) ) ;
#27188 = CARTESIAN_POINT ( 'NONE',  ( -858.8365100919713768, 230.0000000000001990, -202.7499999999880345 ) ) ;
#27189 = DIRECTION ( 'NONE',  ( -0.000000000000000000, 1.000000000000000000, -0.000000000000000000 ) ) ;
#27190 = CARTESIAN_POINT ( 'NONE',  ( 798.5707757039680246, -341.4636090269705733, 356.7845633553585003 ) ) ;
#27191 = VERTEX_POINT ( 'NONE', #11901 ) ;
#27192 = DIRECTION ( 'NONE',  ( 0.000000000000000000, 0.000000000000000000, -1.000000000000000000 ) ) ;
#27193 = AXIS2_PLACEMENT_3D ( 'NONE', #392, #11025, #22089 ) ;
#27194 = CARTESIAN_POINT ( 'NONE',  ( 810.4231160770870019, -96.55451811788039151, 321.9338519418446936 ) ) ;
#27195 = CARTESIAN_POINT ( 'NONE',  ( 749.2812353651451076, -294.4527844766013800, -323.2262854647983090 ) ) ;
#27196 = ADVANCED_FACE ( 'NONE', ( #15811 ), #5644, .T. ) ;
#27197 = LINE ( 'NONE', #10323, #36265 ) ;
#27198 = FACE_OUTER_BOUND ( 'NONE', #41886, .T. ) ;
#27199 = CARTESIAN_POINT ( 'NONE',  ( 771.1735550268778070, -153.1800572038746395, 316.3353852180827630 ) ) ;
#27200 = ORIENTED_EDGE ( 'NONE', *, *, #41642, .F. ) ;
#27201 = CARTESIAN_POINT ( 'NONE',  ( 773.7305795820266212, -417.2817908451522158, 374.8230680027170365 ) ) ;
#27202 = CARTESIAN_POINT ( 'NONE',  ( 768.8385539511368734, -383.2601417444137155, -306.4236121716840557 ) ) ;
#27203 = CARTESIAN_POINT ( 'NONE',  ( 801.1904061080336987, -116.0891481129656029, -368.3070685750235498 ) ) ;
#27204 = CARTESIAN_POINT ( 'NONE',  ( 796.9571628226829034, -47.46360902697148987, 321.2382568024804641 ) ) ;
#27205 = CARTESIAN_POINT ( 'NONE',  ( 745.0891759886404770, -388.2709662947829656, -342.4968714119734159 ) ) ;
#27206 = CARTESIAN_POINT ( 'NONE',  ( 759.9999999999992042, 205.0000000000000568, 339.9999999999999432 ) ) ;
#27207 = CARTESIAN_POINT ( 'NONE',  ( 786.6156483768007774, -433.4419599262316183, 315.5913626894246136 ) ) ;
#27208 = ORIENTED_EDGE ( 'NONE', *, *, #11193, .T. ) ;
#27209 = EDGE_CURVE ( 'NONE', #25389, #28026, #19967, .T. ) ;
#27210 = CARTESIAN_POINT ( 'NONE',  ( 808.7758568127978833, -148.1692326535053610, -320.0363995740631822 ) ) ;
#27211 = CARTESIAN_POINT ( 'NONE',  ( 772.4999999999993179, -462.9681489794448339, 370.0000000000000568 ) ) ;
#27212 = CARTESIAN_POINT ( 'NONE',  ( 811.6461892240364477, -292.7146871989594956, 324.1737431748509835 ) ) ;
#27213 = CARTESIAN_POINT ( 'NONE',  ( 797.8594530101009923, -85.54369356751118403, 322.1405469898982119 ) ) ;
#27214 = EDGE_LOOP ( 'NONE', ( #41155, #35305 ) ) ;
#27215 = CARTESIAN_POINT ( 'NONE',  ( 755.0488828828309806, 6.194403710130517382, -344.1219089521771934 ) ) ;
#27216 = CARTESIAN_POINT ( 'NONE',  ( 797.8594530101008786, -253.5436935675104735, 322.1405469898980982 ) ) ;
#27217 = CARTESIAN_POINT ( 'NONE',  ( 810.7187646348534145, 5.547215523397618142, -356.7737145352016341 ) ) ;
#27218 = CARTESIAN_POINT ( 'NONE',  ( 790.4268473037436706, -448.2010802157933540, 366.7838603755944291 ) ) ;
#27219 = EDGE_CURVE ( 'NONE', #14468, #35726, #22639, .T. ) ;
#27220 = ORIENTED_EDGE ( 'NONE', *, *, #2688, .F. ) ;
#27221 = ORIENTED_EDGE ( 'NONE', *, *, #35972, .T. ) ;
#27222 = CARTESIAN_POINT ( 'NONE',  ( 804.1009440267234822, -407.4636090269703459, -314.0944755984392600 ) ) ;
#27223 = VECTOR ( 'NONE', #12037, 1000.000000000000000 ) ;
#27224 = EDGE_CURVE ( 'NONE', #3234, #7749, #12575, .T. ) ;
#27225 = CARTESIAN_POINT ( 'NONE',  ( 804.4286716492782716, -257.3618753856924286, -345.3141322388244703 ) ) ;
#27227 = CARTESIAN_POINT ( 'NONE',  ( 783.7566961878529810, -240.8965053807777963, 305.1792804349288417 ) ) ;
#27226 = CARTESIAN_POINT ( 'NONE',  ( 808.3070685750232087, -330.9982390220558273, 361.1904061080339829 ) ) ;
#27228 = CARTESIAN_POINT ( 'NONE',  ( 779.4763451958990572, -224.7363362996982232, -365.0264073115438919 ) ) ;
#27229 = CARTESIAN_POINT ( 'NONE',  ( 800.0135310231082713, -206.0891481129653471, -325.0180583372163028 ) ) ;
#27230 = CARTESIAN_POINT ( 'NONE',  ( 774.6858677611749044, -417.7255117493283478, -315.5713283507209894 ) ) ;
#27231 = CARTESIAN_POINT ( 'NONE',  ( 791.9812246680005501, -260.6346026584197375, 361.9419747391813189 ) ) ;
#27232 = ORIENTED_EDGE ( 'NONE', *, *, #18259, .F. ) ;
#27233 = CARTESIAN_POINT ( 'NONE',  ( 745.7998596910086917, -365.3618753856920875, 332.5602148656461168 ) ) ;
#27234 = CARTESIAN_POINT ( 'NONE',  ( 789.7124813865536908, -452.9681489794450613, -363.0370378529873960 ) ) ;
#27235 = CARTESIAN_POINT ( 'NONE',  ( 781.2370466360911223, -20.73633629969883430, -304.9990715423533629 ) ) ;
#27236 = CARTESIAN_POINT ( 'NONE',  ( 795.0120564873543572, 16.45630643248849267, 314.4408280072604498 ) ) ;
#27237 = DIRECTION ( 'NONE',  ( -0.000000000000000000, 1.000000000000000000, -0.000000000000000000 ) ) ;
#27238 = CARTESIAN_POINT ( 'NONE',  ( 796.9571628226829034, -239.4636090269709143, 321.2382568024804641 ) ) ;
#27239 = CARTESIAN_POINT ( 'NONE',  ( 804.9363028652555840, -88.27096629478390355, 338.2165204200192079 ) ) ;
#27240 = VERTEX_POINT ( 'NONE', #9107 ) ;
#27241 = CARTESIAN_POINT ( 'NONE',  ( 813.5763878283155464, -435.8272453906066062, -351.1614460488615350 ) ) ;
#27242 = CARTESIAN_POINT ( 'NONE',  ( 772.4837098697145166, -71.36187538569303968, -374.5518280994205611 ) ) ;
#27243 = CARTESIAN_POINT ( 'NONE',  ( 764.0069404352550464, -255.0783235625958980, 359.2566176426627180 ) ) ;
#27244 = CARTESIAN_POINT ( 'NONE',  ( 778.1981804954714335, -418.2709662947827383, -314.8072714833589885 ) ) ;
#27245 = CARTESIAN_POINT ( 'NONE',  ( 762.3223304703356007, -31.54369356751135456, -322.3223304703362828 ) ) ;
#27246 = EDGE_CURVE ( 'NONE', #14459, #37618, #19067, .T. ) ;
#27247 = CARTESIAN_POINT ( 'NONE',  ( 783.7953271457878373, -8.190881754244330182, 375.1787889125761239 ) ) ;
#27248 = CYLINDRICAL_SURFACE ( 'NONE', #7789, 10.00000000000000888 ) ;
#27249 = CARTESIAN_POINT ( 'NONE',  ( 769.0155153010367712, -274.3726999360617356, -362.7791456095907279 ) ) ;
#27250 = CARTESIAN_POINT ( 'NONE',  ( 754.9967657858570647, -217.5436935675107293, -365.0032342141425374 ) ) ;
#27251 = EDGE_CURVE ( 'NONE', #10697, #34191, #15591, .T. ) ;
#27252 = CARTESIAN_POINT ( 'NONE',  ( 747.2067596250078623, -99.18005720387478164, 352.2312462859687230 ) ) ;
#27253 = CARTESIAN_POINT ( 'NONE',  ( 772.5602148656447525, -129.7255117493292289, 305.7998596910095443 ) ) ;
#27254 = CARTESIAN_POINT ( 'NONE',  ( 799.9999999999993179, -357.6843811873878280, 0.3380660510726891665 ) ) ;
#27255 = FILL_AREA_STYLE ('',( #13174 ) ) ;
#27256 = CARTESIAN_POINT ( 'NONE',  ( 800.1688906516307043, -274.1692326535049915, -369.0717654672308186 ) ) ;
#27257 = AXIS2_PLACEMENT_3D ( 'NONE', #25472, #11627, #35874 ) ;
#27258 = CARTESIAN_POINT ( 'NONE',  ( 762.1177392798416577, -426.5545181178794678, 309.8865473780659272 ) ) ;
#27259 = CARTESIAN_POINT ( 'NONE',  ( 800.9747183278959710, -276.9982390220559978, -311.9810565676471583 ) ) ;
#27260 = DIRECTION ( 'NONE',  ( 0.000000000000000000, 0.000000000000000000, 1.000000000000000000 ) ) ;
#27261 = CARTESIAN_POINT ( 'NONE',  ( 808.3070685750230950, -402.9982390220555430, 361.1904061080339261 ) ) ;
#27262 = CARTESIAN_POINT ( 'NONE',  ( 767.6429770376291799, -9.180057203875058747, 306.8695393053162093 ) ) ;
#27263 = EDGE_CURVE ( 'NONE', #28817, #1373, #13824, .T. ) ;
#27264 = CARTESIAN_POINT ( 'NONE',  ( 755.3201227861273992, -363.7255117493284047, -345.3687786644892981 ) ) ;
#27265 = ADVANCED_FACE ( 'NONE', ( #40987 ), #5401, .F. ) ;
#27266 = CARTESIAN_POINT ( 'NONE',  ( 801.3366627262608972, -8.532869017142163059, 353.0897708529566899 ) ) ;
#27267 = CARTESIAN_POINT ( 'NONE',  ( 778.7502325331095108, -48.35105083532386061, -304.6391490659818828 ) ) ;
#27268 = CARTESIAN_POINT ( 'NONE',  ( 793.2243759319678702, -146.5328690171417350, -318.4439275373583200 ) ) ;
#27269 = CARTESIAN_POINT ( 'NONE',  ( 786.2056067578752163, -179.8055962898688733, 374.4686193811670023 ) ) ;
#27270 = CARTESIAN_POINT ( 'NONE',  ( 795.1360043628808398, 3.910851887033986785, 360.2193346964456282 ) ) ;
#27271 = ORIENTED_EDGE ( 'NONE', *, *, #5410, .T. ) ;
#27272 = CARTESIAN_POINT ( 'NONE',  ( 791.9812246680005501, -68.63460265842033436, -361.9419747391813189 ) ) ;
#27273 = CARTESIAN_POINT ( 'NONE',  ( 775.9200461376533440, -167.8055962898689586, -315.3028492785443291 ) ) ;
#27274 = CARTESIAN_POINT ( 'NONE',  ( 791.9812246680005501, -164.6346026584200217, 361.9419747391813189 ) ) ;
#27275 = CARTESIAN_POINT ( 'NONE',  ( 754.0944755984390895, -15.62377810805123524, -364.1009440267246760 ) ) ;
#27276 = CARTESIAN_POINT ( 'NONE',  ( 774.6312213355099630, -287.3618753856923718, 364.6798772138717482 ) ) ;
#27277 = CYLINDRICAL_SURFACE ( 'NONE', #36719, 2.749999999999863665 ) ;
#27278 = ORIENTED_EDGE ( 'NONE', *, *, #20407, .F. ) ;
#27279 = CARTESIAN_POINT ( 'NONE',  ( 805.0264073115434940, -6.351050835323991173, 339.4763451958999099 ) ) ;
#27280 = CARTESIAN_POINT ( 'NONE',  ( 773.7305795820266212, -321.2817908451525000, -374.8230680027170365 ) ) ;
#27281 = APPLICATION_PROTOCOL_DEFINITION ( 'draft international standard', 'automotive_design', 1998, #37001 ) ;
#27282 = CARTESIAN_POINT ( 'NONE',  ( 751.9810565676468741, -218.0891481129653187, 360.9747183278973921 ) ) ;
#27283 = CARTESIAN_POINT ( 'NONE',  ( 769.0155153010367712, -322.3726999360615082, 362.7791456095907279 ) ) ;
#27284 = CARTESIAN_POINT ( 'NONE',  ( 766.7756240680305382, -422.5328690171408539, 361.5560724626415663 ) ) ;
#27285 = CARTESIAN_POINT ( 'NONE',  ( 805.2837595273609850, -98.73633629969859271, -340.5290396650784714 ) ) ;
#27286 = CARTESIAN_POINT ( 'NONE',  ( 756.5762568750052424, -123.1800572038747106, -348.7366044899774238 ) ) ;
#27287 = CARTESIAN_POINT ( 'NONE',  ( 795.1360043628808398, -332.0891481129649492, -360.2193346964456282 ) ) ;
#27288 = ORIENTED_EDGE ( 'NONE', *, *, #42969, .F. ) ;
#27289 = CARTESIAN_POINT ( 'NONE',  ( 785.3687786644884454, -419.3618753856918033, -315.3201227861279676 ) ) ;
#27290 = CARTESIAN_POINT ( 'NONE',  ( 802.7791456095903868, -292.7146871989594956, 329.0155153010375102 ) ) ;
#27291 = DIRECTION ( 'NONE',  ( -0.000000000000000000, 1.000000000000000000, -0.000000000000000000 ) ) ;
#27292 = CARTESIAN_POINT ( 'NONE',  ( -786.4999999999993179, -434.0043448692482002, 397.6917108626901154 ) ) ;
#27293 = CARTESIAN_POINT ( 'NONE',  ( 754.7162404726377645, -110.7363362996985501, 339.4709603349214717 ) ) ;
#27294 = CARTESIAN_POINT ( 'NONE',  ( 804.4286716492782716, 6.638124614306706306, 345.3141322388244703 ) ) ;
#27295 = VERTEX_POINT ( 'NONE', #37518 ) ;
#27296 = CARTESIAN_POINT ( 'NONE',  ( 781.2370466360911223, -332.7363362996979390, -304.9990715423533629 ) ) ;
#27297 = CARTESIAN_POINT ( 'NONE',  ( 811.3240766477731540, -196.3726999360619061, 355.6651683502462902 ) ) ;
#27298 = CARTESIAN_POINT ( 'NONE',  ( 771.1735550268778070, -321.1800572038740142, -316.3353852180827630 ) ) ;
#27299 = EDGE_CURVE ( 'NONE', #3536, #29825, #8440, .T. ) ;
#27300 = DIRECTION ( 'NONE',  ( 1.000000000000000000, -0.000000000000000000, -0.000000000000000000 ) ) ;
#27301 = CARTESIAN_POINT ( 'NONE',  ( 772.4468031744293057, -177.8272453906074304, -363.8651313633793620 ) ) ;
#27302 = CARTESIAN_POINT ( 'NONE',  ( 782.5225473063381969, -46.27096629478404566, 375.2698199232970637 ) ) ;
#27303 = CARTESIAN_POINT ( 'NONE',  ( 808.5285127195401174, -452.9681489794448339, 336.5948204574517035 ) ) ;
#27304 = CARTESIAN_POINT ( 'NONE',  ( 744.7301800767020268, -388.8164208402374129, -337.4774526936615189 ) ) ;
#27305 = PLANE ( 'NONE',  #43113 ) ;
#27306 = CARTESIAN_POINT ( 'NONE',  ( 815.3608509340175488, -314.7363362996979959, 341.2497674668889545 ) ) ;
#27307 = CYLINDRICAL_SURFACE ( 'NONE', #17602, 6.119000000000013095 ) ;
#27308 = CARTESIAN_POINT ( 'NONE',  ( 814.2001403089898304, -305.3618753856922581, 347.4397851343538264 ) ) ;
#27309 = CARTESIAN_POINT ( 'NONE',  ( 813.1304606946830518, -17.90732993114776406, -352.3570229623690580 ) ) ;
#27310 = EDGE_CURVE ( 'NONE', #9857, #41889, #8679, .T. ) ;
#27311 = CARTESIAN_POINT ( 'NONE',  ( 802.1676090361156639, -230.6346026584197659, -327.8955696845344505 ) ) ;
#27312 = DIRECTION ( 'NONE',  ( 0.000000000000000000, 0.000000000000000000, 1.000000000000000000 ) ) ;
#27313 = CARTESIAN_POINT ( 'NONE',  ( 756.5762568750052424, -387.1800572038738437, 348.7366044899774238 ) ) ;
#27314 = CARTESIAN_POINT ( 'NONE',  ( 802.5472867521000353, -172.3726999360619914, 350.8726784830461156 ) ) ;
#27315 = CARTESIAN_POINT ( 'NONE',  ( 805.0264073115434940, -54.35105083532383219, -339.4763451958999099 ) ) ;
#27316 = CARTESIAN_POINT ( 'NONE',  ( 811.6461892240364477, -76.71468719896012090, 324.1737431748509835 ) ) ;
#27317 = CARTESIAN_POINT ( 'NONE',  ( 755.3201227861273992, -363.7255117493284615, 345.3687786644892981 ) ) ;
#27318 = CARTESIAN_POINT ( 'NONE',  ( 763.2262854647970016, 15.36539734157940629, 309.2812353651462445 ) ) ;
#27319 = SURFACE_SIDE_STYLE ('',( #23828 ) ) ;
#27320 = CARTESIAN_POINT ( 'NONE',  ( 756.5762568750052424, -435.1800572038737869, 348.7366044899774238 ) ) ;
#27321 = VERTEX_POINT ( 'NONE', #37979 ) ;
#27322 = CARTESIAN_POINT ( 'NONE',  ( 755.0636971347428243, -76.27096629478394618, -341.7834795799807353 ) ) ;
#27323 = CARTESIAN_POINT ( 'NONE',  ( 764.0069404352550464, -351.0783235625955854, -359.2566176426627180 ) ) ;
#27325 = CARTESIAN_POINT ( 'NONE',  ( 762.3223304703356007, -175.5436935675108998, 322.3223304703362828 ) ) ;
#27324 = CARTESIAN_POINT ( 'NONE',  ( 788.7366044899766848, -179.9073299311472454, 316.5762568750059813 ) ) ;
#27326 = CARTESIAN_POINT ( 'NONE',  ( 749.8865473780648472, -356.5328690171410813, -322.1177392798429082 ) ) ;
#27327 = CARTESIAN_POINT ( 'NONE',  ( -200.7583438952258916, 294.6698570112193920, -244.9999999999999716 ) ) ;
#27328 = ORIENTED_EDGE ( 'NONE', *, *, #38163, .T. ) ;
#27329 = CARTESIAN_POINT ( 'NONE',  ( 785.3687786644884454, -395.3618753856918602, 315.3201227861279676 ) ) ;
#27330 = VERTEX_POINT ( 'NONE', #10474 ) ;
#27331 = DIRECTION ( 'NONE',  ( -1.880165489482579047E-16, -1.000000000000000000, -0.000000000000000000 ) ) ;
#27332 = CARTESIAN_POINT ( 'NONE',  ( 787.5162901302840055, -227.3618753856925707, -305.4481719005792684 ) ) ;
#27333 = CARTESIAN_POINT ( 'NONE',  ( 811.0346526505617248, -110.6346026584201923, 323.0537975583478101 ) ) ;
#27334 = ORIENTED_EDGE ( 'NONE', *, *, #33712, .T. ) ;
#27335 = CARTESIAN_POINT ( 'NONE',  ( 756.5762568750052424, -195.1800572038744974, -348.7366044899774238 ) ) ;
#27336 = VERTEX_POINT ( 'NONE', #44913 ) ;
#27337 = CARTESIAN_POINT ( 'NONE',  ( 762.1405469898971887, -313.5436935675102745, -357.8594530101015607 ) ) ;
#27338 = CARTESIAN_POINT ( 'NONE',  ( 803.4237431249931660, 8.819942796124882634, -331.2633955100225194 ) ) ;
#27339 = CARTESIAN_POINT ( 'NONE',  ( 783.0433043558608688, -192.8965053807779668, 315.1538015810313027 ) ) ;
#27340 = DIRECTION ( 'NONE',  ( -1.000000000000000000, -0.000000000000000000, 0.000000000000000000 ) ) ;
#27341 = CARTESIAN_POINT ( 'NONE',  ( 181.1634899080285948, 230.0000000000000000, -199.9999999999953957 ) ) ;
#27342 = PRODUCT_DEFINITION_SHAPE ( 'NONE', 'NONE',  #45734 ) ;
#27343 = ORIENTED_EDGE ( 'NONE', *, *, #14519, .F. ) ;
#27344 = CARTESIAN_POINT ( 'NONE',  ( 800.9840315886518738, -460.9181544815156713, -354.1144889064786412 ) ) ;
#27345 = FACE_OUTER_BOUND ( 'NONE', #40251, .T. ) ;
#27346 = DIRECTION ( 'NONE',  ( 0.000000000000000000, 0.000000000000000000, -1.000000000000000000 ) ) ;
#27347 = CARTESIAN_POINT ( 'NONE',  ( 745.7194118038753459, -253.6454272087889876, -348.7631598425976449 ) ) ;
#27348 = CARTESIAN_POINT ( 'NONE',  ( 786.2694204179717872, -93.28179084515315367, 305.1769319972829067 ) ) ;
#27350 = CARTESIAN_POINT ( 'NONE',  ( 762.1405469898971887, -217.5436935675107293, -357.8594530101015607 ) ) ;
#27349 = PLANE ( 'NONE',  #291 ) ;
#27351 = CARTESIAN_POINT ( 'NONE',  ( 803.8651313633788504, -365.2601417444137155, -332.4468031744301015 ) ) ;
#27352 = CARTESIAN_POINT ( 'NONE',  ( 814.2805881961230625, -241.6454272087890729, -331.2368401574024119 ) ) ;
#27353 = SURFACE_SIDE_STYLE ('',( #17660 ) ) ;
#27354 = CARTESIAN_POINT ( 'NONE',  ( 780.5236548040995785, -92.73633629969860692, -314.9735926884559944 ) ) ;
#27355 = CARTESIAN_POINT ( 'NONE',  ( 805.2837595273609850, -434.7363362996975980, 340.5290396650784714 ) ) ;
#27356 = CARTESIAN_POINT ( 'NONE',  ( 999.9999999999992042, 478.9999999999999432, 359.0000000000000000 ) ) ;
#27357 = CARTESIAN_POINT ( 'NONE',  ( 754.8983024940795303, -426.8965053807771142, -336.9254006560228163 ) ) ;
#27358 = CARTESIAN_POINT ( 'NONE',  ( 777.5031285880264704, -286.8164208402378677, -374.9108240113588408 ) ) ;
#27359 = CARTESIAN_POINT ( 'NONE',  ( 187.1337867209877857, 56.78581973499402835, 212.6378164459127049 ) ) ;
#27360 = DIRECTION ( 'NONE',  ( 0.000000000000000000, 0.000000000000000000, 1.000000000000000000 ) ) ;
#27361 = CARTESIAN_POINT ( 'NONE',  ( 791.9812246680005501, -44.63460265842040542, -361.9419747391813189 ) ) ;
#27362 = CARTESIAN_POINT ( 'NONE',  ( 778.7629533639073998, -224.7363362996982232, 375.0009284576466371 ) ) ;
#27363 = CARTESIAN_POINT ( 'NONE',  ( 747.3154664389472828, -163.9874144716871456, -326.4474001241230781 ) ) ;
#27364 = CARTESIAN_POINT ( 'NONE',  ( 745.0891759886404770, -172.2709662947836478, 342.4968714119734159 ) ) ;
#27365 = CARTESIAN_POINT ( 'NONE',  ( 813.1304606946830518, -425.9073299311463074, -352.3570229623690580 ) ) ;
#27366 = DIRECTION ( 'NONE',  ( -0.000000000000000000, 1.000000000000000000, -0.000000000000000000 ) ) ;
#27367 = CARTESIAN_POINT ( 'NONE',  ( 759.9864689768902508, -290.0891481129650629, 354.9819416627836404 ) ) ;
#27368 = CARTESIAN_POINT ( 'NONE',  ( 755.1538015810308480, -62.19088175424416676, 343.0433043558613804 ) ) ;
#27369 = CARTESIAN_POINT ( 'NONE',  ( 795.1360043628807261, -428.0891481129644944, -360.2193346964456282 ) ) ;
#27370 = DIRECTION ( 'NONE',  ( 0.000000000000000000, -0.000000000000000000, 1.000000000000000000 ) ) ;
#27371 = CARTESIAN_POINT ( 'NONE',  ( 999.9999999999992042, -590.0000000000001137, -360.0000000000000000 ) ) ;
#27373 = CARTESIAN_POINT ( 'NONE',  ( 804.6798772138708955, -327.7255117493285184, 334.6312213355107019 ) ) ;
#27372 = CARTESIAN_POINT ( 'NONE',  ( 754.8983024940795303, -114.8965053807782226, 336.9254006560228163 ) ) ;
#27374 = ORIENTED_EDGE ( 'NONE', *, *, #38685, .F. ) ;
#27375 = CARTESIAN_POINT ( 'NONE',  ( 794.1144889064781864, -250.1692326535050199, -360.9840315886528401 ) ) ;
#27376 = CARTESIAN_POINT ( 'NONE',  ( 792.1044303154645831, -132.4527844766018916, -317.8323909638837677 ) ) ;
#27377 = CARTESIAN_POINT ( 'NONE',  ( 785.3687786644884454, -83.36187538569296862, 315.3201227861279676 ) ) ;
#27378 = CARTESIAN_POINT ( 'NONE',  ( 812.6845335610512393, -247.9874144716867761, -353.5525998758768651 ) ) ;
#27379 = CARTESIAN_POINT ( 'NONE',  ( 989.9999999999992042, -190.2822455671962416, 69.00746428064729798 ) ) ;
#27380 = CARTESIAN_POINT ( 'NONE',  ( 803.8556311672234642, -369.6237781080500895, 365.6418435158340117 ) ) ;
#27381 = VERTEX_POINT ( 'NONE', #20416 ) ;
#27382 = CARTESIAN_POINT ( 'NONE',  ( 762.3223304703356007, -295.5436935675105588, 322.3223304703362828 ) ) ;
#27383 = CARTESIAN_POINT ( 'NONE',  ( 814.5518280994195948, 8.274488250670337663, 332.4837098697145734 ) ) ;
#27384 = CARTESIAN_POINT ( 'NONE',  ( 776.9566956441375396, -60.89650538077837894, -364.8461984189686405 ) ) ;
#27385 = CARTESIAN_POINT ( 'NONE',  ( 802.1676090361156639, -182.6346026584199649, -327.8955696845344505 ) ) ;
#27386 = CARTESIAN_POINT ( 'NONE',  ( 755.3201227861273992, -387.7255117493283478, 345.3687786644892981 ) ) ;
#27387 = CARTESIAN_POINT ( 'NONE',  ( 792.2312462859673587, -107.9073299311474727, -307.2067596250082602 ) ) ;
#27388 = CARTESIAN_POINT ( 'NONE',  ( 781.8018195045267476, -118.2709662947838041, -365.1927285166407273 ) ) ;
#27389 = ORIENTED_EDGE ( 'NONE', *, *, #24423, .T. ) ;
#27390 = CARTESIAN_POINT ( 'NONE',  ( 793.0897708529556667, -54.55451811788054783, -361.3366627262616362 ) ) ;
#27391 = CARTESIAN_POINT ( 'NONE',  ( 772.4468031744293057, -345.8272453906069472, -363.8651313633793620 ) ) ;
#27393 = CARTESIAN_POINT ( 'NONE',  ( 760.7433823573367135, -420.0090635724249069, 355.9930595647440441 ) ) ;
#27392 = CARTESIAN_POINT ( 'NONE',  ( 757.8323909638827445, -98.63460265842024910, 352.1044303154654358 ) ) ;
#27396 = CARTESIAN_POINT ( 'NONE',  ( 815.0009284576459549, -366.3510508353228374, 338.7629533639073429 ) ) ;
#27395 = DIRECTION ( 'NONE',  ( -0.000000000000000000, 1.000000000000000000, -0.000000000000000000 ) ) ;
#27394 = LINE ( 'NONE', #31314, #22539 ) ;
#27397 = CARTESIAN_POINT ( 'NONE',  ( 749.8865473780648472, -116.5328690171418202, 322.1177392798429082 ) ) ;
#27398 = CARTESIAN_POINT ( 'NONE',  ( 783.0745993439762742, -368.1908817542433212, -365.1016975059196739 ) ) ;
#27399 = CARTESIAN_POINT ( 'NONE',  ( 792.1044303154645831, -372.4527844766010958, -317.8323909638837677 ) ) ;
#27400 = CARTESIAN_POINT ( 'NONE',  ( 748.6759233522253680, -136.3726999360621051, -324.3348316497537098 ) ) ;
#27401 = CARTESIAN_POINT ( 'NONE',  ( 812.7932403749906598, -447.1800572038736732, 327.7687537140311633 ) ) ;
#27403 = CARTESIAN_POINT ( 'NONE',  ( 799.9999999999993179, -512.9681489794448908, 370.0000000000000000 ) ) ;
#27402 = CARTESIAN_POINT ( 'NONE',  ( 999.5857864376259840, 479.9999999999999432, -199.9999999999999432 ) ) ;
#27404 = CARTESIAN_POINT ( 'NONE',  ( 757.2208543904082489, -256.7146871989595525, -350.9844846989624330 ) ) ;
#27405 = CARTESIAN_POINT ( 'NONE',  ( 771.3260364891663130, -163.6454272087893003, -306.0683387631859773 ) ) ;
#27406 = CARTESIAN_POINT ( 'NONE',  ( 769.9999999999992042, 205.0000000000000568, -339.9999999999999432 ) ) ;
#27407 = CARTESIAN_POINT ( 'NONE',  ( 521.6730038022808458, 199.9999999999999147, 339.9999999999999432 ) ) ;
#27408 = CARTESIAN_POINT ( 'NONE',  ( 804.6971507214547046, -315.2817908451525000, 344.0799538623459739 ) ) ;
#27409 = EDGE_LOOP ( 'NONE', ( #4497, #774 ) ) ;
#27410 = CARTESIAN_POINT ( 'NONE',  ( 802.2119215644370342, -318.0090635724251911, 367.5423716828165084 ) ) ;
#27411 = EDGE_CURVE ( 'NONE', #8915, #13265, #13271, .T. ) ;
#27412 = CARTESIAN_POINT ( 'NONE',  ( 796.9462024416508257, -180.4527844766017495, -308.9653473494370246 ) ) ;
#27413 = CARTESIAN_POINT ( 'NONE',  ( -769.9999999999992042, 205.0000000000000568, -339.9999999999999432 ) ) ;
#27414 = CARTESIAN_POINT ( 'NONE',  ( 802.2119215644370342, -102.0090635724258448, 367.5423716828165084 ) ) ;
#27415 = CARTESIAN_POINT ( 'NONE',  ( 759.0252816721024374, -312.9982390220559409, -368.0189434323527280 ) ) ;
#27416 = FACE_OUTER_BOUND ( 'NONE', #2840, .T. ) ;
#27417 = CARTESIAN_POINT ( 'NONE',  ( 775.4999999999993179, -513.1383975375929367, -350.0000000000000000 ) ) ;
#27418 = CARTESIAN_POINT ( 'NONE',  ( 767.8955696845333705, -168.4527844766018347, 362.1676090361162323 ) ) ;
#27419 = AXIS2_PLACEMENT_3D ( 'NONE', #32594, #4204, #25423 ) ;
#27420 = CARTESIAN_POINT ( 'NONE',  ( 815.3608509340175488, -434.7363362996975980, 341.2497674668889545 ) ) ;
#27421 = CARTESIAN_POINT ( 'NONE',  ( 810.1134526219336749, -392.5328690171409107, -357.8822607201570349 ) ) ;
#27422 = CARTESIAN_POINT ( 'NONE',  ( 796.9462024416508257, -132.4527844766018916, -308.9653473494370246 ) ) ;
#27423 = CARTESIAN_POINT ( 'NONE',  ( 783.0745993439762742, -56.19088175424417386, 365.1016975059196739 ) ) ;
#27424 = CARTESIAN_POINT ( 'NONE',  ( 758.8095938919642549, -392.0891481129648355, -311.6929314249763365 ) ) ;
#27425 = CARTESIAN_POINT ( 'NONE',  ( 919.9999999999993179, 154.9999999999998863, 350.0000000000000000 ) ) ;
#27426 = CARTESIAN_POINT ( 'NONE',  ( 760.5453621957607311, -429.0783235625953580, 323.8424801807151425 ) ) ;
#27427 = ORIENTED_EDGE ( 'NONE', *, *, #16452, .T. ) ;
#27428 = CARTESIAN_POINT ( 'NONE',  ( 754.0944755984390895, -159.6237781080508285, -364.1009440267246760 ) ) ;
#27429 = CARTESIAN_POINT ( 'NONE',  ( 811.6461892240364477, -268.7146871989595525, 324.1737431748509835 ) ) ;
#27430 = CARTESIAN_POINT ( 'NONE',  ( 755.3201227861273992, -75.72551174932938522, 345.3687786644892981 ) ) ;
#27431 = VERTEX_POINT ( 'NONE', #10250 ) ;
#27432 = CARTESIAN_POINT ( 'NONE',  ( 754.9735926884551418, -18.35105083532395298, -340.5236548041000333 ) ) ;
#27433 = CARTESIAN_POINT ( 'NONE',  ( 802.1676090361156639, -278.6346026584196807, 327.8955696845344505 ) ) ;
#27434 = CARTESIAN_POINT ( 'NONE',  ( 745.0891759886404770, -4.270966294784170003, -342.4968714119734159 ) ) ;
#27435 = DIRECTION ( 'NONE',  ( -0.000000000000000000, 1.000000000000000000, -0.000000000000000000 ) ) ;
#27436 = VERTEX_POINT ( 'NONE', #16961 ) ;
#27437 = ORIENTED_EDGE ( 'NONE', *, *, #28592, .F. ) ;
#27438 = CARTESIAN_POINT ( 'NONE',  ( 744.6391490659812007, -398.7363362996976548, -338.7502325331110455 ) ) ;
#27439 = CARTESIAN_POINT ( 'NONE',  ( 762.3223304703356007, -271.5436935675106156, -322.3223304703362828 ) ) ;
#27441 = CARTESIAN_POINT ( 'NONE',  ( 793.4146539503750546, -241.9874144716869182, 307.6481478633938877 ) ) ;
#27440 = CARTESIAN_POINT ( 'NONE',  ( 782.4968714119720516, -346.8164208402376971, 305.0891759886411023 ) ) ;
#27442 = EDGE_CURVE ( 'NONE', #30488, #14297, #27809, .T. ) ;
#27443 = CARTESIAN_POINT ( 'NONE',  ( 754.7162404726377645, -254.7363362996981095, -339.4709603349214717 ) ) ;
#27444 = CARTESIAN_POINT ( 'NONE',  ( 791.9812246680005501, -260.6346026584197375, -361.9419747391813189 ) ) ;
#27445 = VECTOR ( 'NONE', #9798, 999.9999999999998863 ) ;
#27446 = CARTESIAN_POINT ( 'NONE',  ( 757.8323909638828582, -434.6346026584190554, -352.1044303154654358 ) ) ;
#27447 = CARTESIAN_POINT ( 'NONE',  ( 803.6646147819161570, -233.9073299311470180, 348.8264449731210561 ) ) ;
#27448 = ORIENTED_EDGE ( 'NONE', *, *, #42479, .T. ) ;
#27449 = CARTESIAN_POINT ( 'NONE',  ( 745.7998596910086917, -341.3618753856922012, 332.5602148656461168 ) ) ;
#27450 = DIRECTION ( 'NONE',  ( 1.000000000000000000, -0.000000000000000000, -0.000000000000000000 ) ) ;
#27451 = CARTESIAN_POINT ( 'NONE',  ( 764.1737431748507561, -34.37269993606243901, -371.6461892240376415 ) ) ;
#27452 = FACE_OUTER_BOUND ( 'NONE', #27900, .T. ) ;
#27453 = FACE_OUTER_BOUND ( 'NONE', #28465, .T. ) ;
#27454 = EDGE_CURVE ( 'NONE', #1441, #23261, #24549, .T. ) ;
#27455 = CARTESIAN_POINT ( 'NONE',  ( 804.1105419155481968, -219.8272453906073167, 347.6308680596136469 ) ) ;
#27456 = CARTESIAN_POINT ( 'NONE',  ( 762.3223304703356007, -103.5436935675111272, 322.3223304703362828 ) ) ;
#27457 = ORIENTED_EDGE ( 'NONE', *, *, #43102, .F. ) ;
#27458 = CARTESIAN_POINT ( 'NONE',  ( 804.1105419155481968, -27.82724539060790292, -347.6308680596136469 ) ) ;
#27459 = CARTESIAN_POINT ( 'NONE',  ( 787.4397851343537695, -69.72551174932942786, -374.2001403089903988 ) ) ;
#27460 = CARTESIAN_POINT ( 'NONE',  ( 783.0433043558608688, -288.8965053807775121, 315.1538015810313027 ) ) ;
#27461 = CARTESIAN_POINT ( 'NONE',  ( 800.0135310231082713, -422.0891481129647218, -325.0180583372163028 ) ) ;
#27462 = CARTESIAN_POINT ( 'NONE',  ( 797.8594530101009923, -37.54369356751133324, -322.1405469898982119 ) ) ;
#27463 = CARTESIAN_POINT ( 'NONE',  ( 813.5763878283155464, -3.827245390607979303, 351.1614460488615350 ) ) ;
#27464 = CARTESIAN_POINT ( 'NONE',  ( 747.2067596250078623, -195.1800572038744974, -352.2312462859687230 ) ) ;
#27465 = CARTESIAN_POINT ( 'NONE',  ( 745.4481719005789273, -75.72551174932937101, 347.5162901302853129 ) ) ;
#27466 = CARTESIAN_POINT ( 'NONE',  ( 767.7687537140311633, -167.9073299311473022, 372.7932403749916830 ) ) ;
#27467 = AXIS2_PLACEMENT_3D ( 'NONE', #23015, #43156, #40598 ) ;
#27468 = CARTESIAN_POINT ( 'NONE',  ( 779.9999999999992042, 126.4563064324884465, 329.9999999999999432 ) ) ;
#27469 = FACE_OUTER_BOUND ( 'NONE', #19830, .T. ) ;
#27470 = CARTESIAN_POINT ( 'NONE',  ( 752.4576283171824116, -261.0783235625959264, -317.7880784355627952 ) ) ;
#27471 = CARTESIAN_POINT ( 'NONE',  ( 750.9282345327678740, -400.9181544815159555, 319.8311093483690115 ) ) ;
#27472 = ADVANCED_FACE ( 'NONE', ( #17180 ), #27349, .T. ) ;
#27473 = CARTESIAN_POINT ( 'NONE',  ( 747.2067596250078623, -267.1800572038742985, -352.2312462859687230 ) ) ;
#27474 = LINE ( 'NONE', #34858, #36099 ) ;
#27475 = CARTESIAN_POINT ( 'NONE',  ( 782.4968714119720516, -394.8164208402374697, 305.0891759886411023 ) ) ;
#27476 = CARTESIAN_POINT ( 'NONE',  ( 814.2001403089898304, -17.36187538569322086, 347.4397851343538264 ) ) ;
#27477 = CARTESIAN_POINT ( 'NONE',  ( 803.4237431249931660, -351.1800572038740142, -331.2633955100225194 ) ) ;
#27478 = CARTESIAN_POINT ( 'NONE',  ( 799.4546378042377910, -33.07832356259662987, 356.1575198192848006 ) ) ;
#27479 = CARTESIAN_POINT ( 'NONE',  ( 764.3348316497523456, -46.71468719896022748, -308.6759233522265617 ) ) ;
#27480 = CARTESIAN_POINT ( 'NONE',  ( 754.8983024940795303, -138.8965053807781374, -336.9254006560228163 ) ) ;
#27481 = CARTESIAN_POINT ( 'NONE',  ( 751.2241431872005251, -184.1692326535052757, 359.9636004259367610 ) ) ;
#27482 = CARTESIAN_POINT ( 'NONE',  ( 778.2165204200184689, 1.183579159761269040, 364.9363028652563230 ) ) ;
#27483 = EDGE_LOOP ( 'NONE', ( #5163, #8860, #16361, #19374 ) ) ;
#27484 = CARTESIAN_POINT ( 'NONE',  ( 767.8955696845333705, -72.45278447660213317, -362.1676090361162323 ) ) ;
#27485 = CARTESIAN_POINT ( 'NONE',  ( 796.7845633553578182, -177.6237781080507148, -358.5707757039688204 ) ) ;
#27486 = PRODUCT_DEFINITION_CONTEXT ( 'detailed design', #37001, 'design' ) ;
#27487 = CARTESIAN_POINT ( 'NONE',  ( 802.1676090361156639, -158.6346026584199933, 327.8955696845344505 ) ) ;
#27488 = CARTESIAN_POINT ( 'NONE',  ( 812.6845335610512393, 16.01258552831230375, -353.5525998758768651 ) ) ;
#27489 = CARTESIAN_POINT ( 'NONE',  ( 771.2633955100217236, -287.9073299311468759, 363.4237431249939618 ) ) ;
#27490 = DIRECTION ( 'NONE',  ( 0.000000000000000000, -0.6594541114781782287, -0.7517448203044211352 ) ) ;
#27491 = VERTEX_POINT ( 'NONE', #6560 ) ;
#27492 = CARTESIAN_POINT ( 'NONE',  ( 756.7813123517142913, -19.98741447168758256, 329.9779781133712504 ) ) ;
#27493 = CARTESIAN_POINT ( 'NONE',  ( 788.6739635108323228, -295.6454272087888739, -373.9316612368139090 ) ) ;
#27494 = ADVANCED_FACE ( 'NONE', ( #35193 ), #34265, .F. ) ;
#27495 = CARTESIAN_POINT ( 'NONE',  ( 808.3070685750232087, -258.9982390220561115, 361.1904061080339829 ) ) ;
#27496 = EDGE_CURVE ( 'NONE', #6776, #34351, #13495, .T. ) ;
#27497 = CARTESIAN_POINT ( 'NONE',  ( 793.0897708529556667, -342.5545181178796952, 361.3366627262616362 ) ) ;
#27498 = CARTESIAN_POINT ( 'NONE',  ( 790.8726784830453198, -442.7146871989589840, 362.5472867521010585 ) ) ;
#27499 = CARTESIAN_POINT ( 'NONE',  ( 793.9708237608222134, -166.9181544815165523, -319.2295555964448681 ) ) ;
#27500 = CARTESIAN_POINT ( 'NONE',  ( 771.1735550268778070, -105.1800572038747248, -316.3353852180827630 ) ) ;
#27501 = VECTOR ( 'NONE', #23641, 1000.000000000000000 ) ;
#27502 = EDGE_LOOP ( 'NONE', ( #16238, #37044 ) ) ;
#27503 =( GEOMETRIC_REPRESENTATION_CONTEXT ( 3 ) GLOBAL_UNCERTAINTY_ASSIGNED_CONTEXT ( ( #1918 ) ) GLOBAL_UNIT_ASSIGNED_CONTEXT ( ( #28708, #14857, #969 ) ) REPRESENTATION_CONTEXT ( 'NONE', 'WORKASPACE' ) );
#27504 = CARTESIAN_POINT ( 'NONE',  ( 800.7704444035546203, -292.1692326535048210, 326.0291762391768771 ) ) ;
#27505 = LINE ( 'NONE', #33983, #1246 ) ;
#27506 = EDGE_CURVE ( 'NONE', #33095, #20456, #23862, .T. ) ;
#27507 = CARTESIAN_POINT ( 'NONE',  ( 783.0745993439762742, -128.1908817542439465, 365.1016975059196739 ) ) ;
#27508 = CARTESIAN_POINT ( 'NONE',  ( 778.1981804954714335, -10.27096629478414691, 314.8072714833589885 ) ) ;
#27509 = ORIENTED_EDGE ( 'NONE', *, *, #34612, .F. ) ;
#27510 = CARTESIAN_POINT ( 'NONE',  ( 814.2805881961230625, -385.6454272087888171, -331.2368401574024119 ) ) ;
#27511 = CARTESIAN_POINT ( 'NONE',  ( 752.7379699480933368, -228.0090635724254753, 361.9858362298580232 ) ) ;
#27512 = CARTESIAN_POINT ( 'NONE',  ( 785.3141322388236176, -333.7255117493286320, -364.4286716492789537 ) ) ;
#27513 = CARTESIAN_POINT ( 'NONE',  ( 799.9999999999993179, -462.9681489794448339, -309.9999999999998863 ) ) ;
#27514 = CARTESIAN_POINT ( 'NONE',  ( 755.3028492785439312, -183.2817908451528695, -335.9200461376539693 ) ) ;
#27515 = CARTESIAN_POINT ( 'NONE',  ( 814.2001403089898304, -89.36187538569299704, 347.4397851343538264 ) ) ;
#27516 = CARTESIAN_POINT ( 'NONE',  ( 809.5171784329539832, -452.9681489794445497, 335.1922280983832252 ) ) ;
#27517 = CARTESIAN_POINT ( 'NONE',  ( 759.0252816721024374, -384.9982390220556567, -368.0189434323527280 ) ) ;
#27518 = CARTESIAN_POINT ( 'NONE',  ( -39.63011601220123481, -365.3551492539851893, -18.13243251470705886 ) ) ;
#27519 = EDGE_CURVE ( 'NONE', #18941, #35125, #28302, .T. ) ;
#27520 = CARTESIAN_POINT ( 'NONE',  ( 776.2046728542105711, -308.1908817542434349, 304.8212110874238761 ) ) ;
#27521 = EDGE_CURVE ( 'NONE', #24322, #27963, #31038, .T. ) ;
#27522 = DIRECTION ( 'NONE',  ( 0.000000000000000000, 0.000000000000000000, 1.000000000000000000 ) ) ;
#27523 = CARTESIAN_POINT ( 'NONE',  ( 810.7187646348534145, -306.4527844766013800, 356.7737145352016341 ) ) ;
#27524 = CARTESIAN_POINT ( 'NONE',  ( 745.0891759886404770, -4.270966294784170003, -342.4968714119734159 ) ) ;
#27525 = CARTESIAN_POINT ( 'NONE',  ( 804.4286716492782716, -233.3618753856925423, -345.3141322388244703 ) ) ;
#27526 = DIRECTION ( 'NONE',  ( -1.000000000000000000, -0.000000000000000000, -0.000000000000000000 ) ) ;
#27527 = CARTESIAN_POINT ( 'NONE',  ( 791.9812246680005501, -404.6346026584193396, 361.9419747391813189 ) ) ;
#27528 = CARTESIAN_POINT ( 'NONE',  ( 763.0428371773158460, -155.4636090269711417, 358.7617431975195359 ) ) ;
#27529 = CARTESIAN_POINT ( 'NONE',  ( 747.6481478633932056, -37.09997266333514432, -353.4146539503763620 ) ) ;
#27530 = CARTESIAN_POINT ( 'NONE',  ( 769.1273215169530886, -46.71468719896022748, -317.4527132478988847 ) ) ;
#27531 = CARTESIAN_POINT ( 'NONE',  ( 800.1688906516307043, -58.16923265350564520, 369.0717654672308186 ) ) ;
#27532 = CARTESIAN_POINT ( 'NONE',  ( 804.4286716492782716, -377.3618753856920875, 345.3141322388244703 ) ) ;
#27533 = CIRCLE ( 'NONE', #26800, 8.024999999999948841 ) ;
#27534 = CARTESIAN_POINT ( 'NONE',  ( 755.2512626584698410, 16.45630643248848912, 315.2512626584710915 ) ) ;
#27535 = CARTESIAN_POINT ( 'NONE',  ( 749.8865473780648472, -140.5328690171417634, 322.1177392798429082 ) ) ;
#27536 = CARTESIAN_POINT ( 'NONE',  ( 774.6858677611749044, -417.7255117493283478, 315.5713283507209894 ) ) ;
#27537 = ORIENTED_EDGE ( 'NONE', *, *, #25839, .T. ) ;
#27538 = CARTESIAN_POINT ( 'NONE',  ( 764.8639956371174549, -80.08914811296574499, -319.7806653035542013 ) ) ;
#27539 = CARTESIAN_POINT ( 'NONE',  ( 801.3366627262608972, -368.5328690171409676, -353.0897708529566899 ) ) ;
#27541 = CARTESIAN_POINT ( 'NONE',  ( 805.1927285166399315, -184.8164208402381234, 341.8018195045277707 ) ) ;
#27540 = CARTESIAN_POINT ( 'NONE',  ( 801.9419747391806368, -210.4527844766016926, 351.9812246680014027 ) ) ;
#27542 = VERTEX_POINT ( 'NONE', #38432 ) ;
#27543 = CARTESIAN_POINT ( 'NONE',  ( 747.3154664389472828, -379.9874144716865203, -326.4474001241230781 ) ) ;
#27544 = LINE ( 'NONE', #41648, #42634 ) ;
#27545 = ORIENTED_EDGE ( 'NONE', *, *, #37043, .F. ) ;
#27546 = CARTESIAN_POINT ( 'NONE',  ( 778.2165204200184689, -406.8164208402375266, 364.9363028652563230 ) ) ;
#27547 = AXIS2_PLACEMENT_3D ( 'NONE', #25100, #14953, #43564 ) ;
#27548 = ADVANCED_FACE ( 'NONE', ( #17425, #6333 ), #21110, .T. ) ;
#27549 = EDGE_LOOP ( 'NONE', ( #1975, #44306, #29329, #14790 ) ) ;
#27550 = CARTESIAN_POINT ( 'NONE',  ( 814.5518280994195948, -207.7255117493289447, -332.4837098697145734 ) ) ;
#27551 = CARTESIAN_POINT ( 'NONE',  ( 748.9653473494365699, -146.6346026584200786, 356.9462024416520762 ) ) ;
#27552 = EDGE_CURVE ( 'NONE', #20679, #18073, #32000, .T. ) ;
#27553 = EDGE_LOOP ( 'NONE', ( #1465, #6327, #10515, #6015 ) ) ;
#27554 = CARTESIAN_POINT ( 'NONE',  ( 774.6858677611749044, -201.7255117493290015, -315.5713283507209894 ) ) ;
#27555 = ORIENTED_EDGE ( 'NONE', *, *, #15681, .T. ) ;
#27556 = CARTESIAN_POINT ( 'NONE',  ( 788.7366044899766848, -323.9073299311468190, -316.5762568750059813 ) ) ;
#27557 = CARTESIAN_POINT ( 'NONE',  ( 800.2193346964447755, -18.99823902205683979, -355.1360043628815788 ) ) ;
#27558 = CARTESIAN_POINT ( 'NONE',  ( 761.2382568024794409, -183.6237781080507148, 356.9571628226838129 ) ) ;
#27559 = ADVANCED_FACE ( 'NONE', ( #7021, #27571, #13954, #44682 ), #10032, .F. ) ;
#27560 = CYLINDRICAL_SURFACE ( 'NONE', #40288, 19.99999999999990763 ) ;
#27561 = LINE ( 'NONE', #7012, #9554 ) ;
#27562 = VERTEX_POINT ( 'NONE', #38664 ) ;
#27563 = CARTESIAN_POINT ( 'NONE',  ( 790.7339360641449275, -462.9631818684622999, -362.6136660859752965 ) ) ;
#27564 = CARTESIAN_POINT ( 'NONE',  ( 770.0084009877317612, 19.77989614203463375, -311.3857915150574627 ) ) ;
#27565 = DIRECTION ( 'NONE',  ( 0.000000000000000000, 0.000000000000000000, 1.000000000000000000 ) ) ;
#27566 = VECTOR ( 'NONE', #22754, 1000.000000000000114 ) ;
#27567 = ORIENTED_EDGE ( 'NONE', *, *, #32926, .F. ) ;
#27568 = CARTESIAN_POINT ( 'NONE',  ( 813.5763878283155464, -243.8272453906072030, -351.1614460488615350 ) ) ;
#27569 = MECHANICAL_DESIGN_GEOMETRIC_PRESENTATION_REPRESENTATION (  '', ( #18746 ), #23127 ) ;
#27570 = CARTESIAN_POINT ( 'NONE',  ( 773.7305795820266212, -129.2817908451530400, 374.8230680027170365 ) ) ;
#27572 = CARTESIAN_POINT ( 'NONE',  ( 771.2633955100217236, -215.9073299311471317, -363.4237431249939618 ) ) ;
#27571 = FACE_BOUND ( 'NONE', #9419, .T. ) ;
#27573 = CARTESIAN_POINT ( 'NONE',  ( 765.8855110935204493, -382.1692326535045936, -319.0159684113471599 ) ) ;
#27574 = DIRECTION ( 'NONE',  ( 0.000000000000000000, 0.7071067811865578978, 0.7071067811865372477 ) ) ;
#27575 = FACE_OUTER_BOUND ( 'NONE', #27719, .T. ) ;
#27576 = CARTESIAN_POINT ( 'NONE',  ( 755.5913626894240451, -85.64542720878952764, -346.6156483768012890 ) ) ;
#27577 = CARTESIAN_POINT ( 'NONE',  ( 798.5707757039680246, -437.4636090269703459, 356.7845633553585003 ) ) ;
#27578 = CARTESIAN_POINT ( 'NONE',  ( 799.9636004259356241, -358.9181544815160123, 311.2241431872006956 ) ) ;
#27579 = DIRECTION ( 'NONE',  ( 0.000000000000000000, 0.000000000000000000, 1.000000000000000000 ) ) ;
#27580 = CARTESIAN_POINT ( 'NONE',  ( 744.8212110874229666, 5.103494619221427442, -336.2046728542121627 ) ) ;
#27581 = CARTESIAN_POINT ( 'NONE',  ( 744.7301800767020268, -292.8164208402378108, -337.4774526936615189 ) ) ;
#27582 = CARTESIAN_POINT ( 'NONE',  ( -858.8365100919713768, 240.0000000000002274, -202.7499999999880345 ) ) ;
#27583 = CARTESIAN_POINT ( 'NONE',  ( 802.1676090361156639, 9.365397341579420498, 327.8955696845344505 ) ) ;
#27584 = CARTESIAN_POINT ( 'NONE',  ( 762.3223304703356007, -79.54369356751119824, -322.3223304703362828 ) ) ;
#27585 = AXIS2_PLACEMENT_3D ( 'NONE', #8169, #36110, #29182 ) ;
#27586 = CARTESIAN_POINT ( 'NONE',  ( 747.6481478633932056, -229.0999726633345404, 353.4146539503763620 ) ) ;
#27587 = CARTESIAN_POINT ( 'NONE',  ( 815.0009284576459549, -174.3510508353234627, -338.7629533639073429 ) ) ;
#27588 = CARTESIAN_POINT ( 'NONE',  ( 755.2512626584698410, -199.5436935675108430, 315.2512626584710915 ) ) ;
#27589 = CARTESIAN_POINT ( 'NONE',  ( 777.4774526936600978, -394.2709662947827951, -304.7301800767027657 ) ) ;
#27590 = DIRECTION ( 'NONE',  ( -0.000000000000000000, 1.000000000000000000, -0.000000000000000000 ) ) ;
#27591 = CARTESIAN_POINT ( 'NONE',  ( 771.1735550268778070, -273.1800572038742985, 316.3353852180827630 ) ) ;
#27592 = CARTESIAN_POINT ( 'NONE',  ( 759.0159684113467620, -64.91815448151686496, 325.8855110935213020 ) ) ;
#27593 = CARTESIAN_POINT ( 'NONE',  ( 794.9819416627830151, -420.9982390220555999, -319.9864689768909898 ) ) ;
#27594 = LINE ( 'NONE', #31739, #17376 ) ;
#27595 = FACE_BOUND ( 'NONE', #7968, .T. ) ;
#27597 = CARTESIAN_POINT ( 'NONE',  ( 756.5762568750052424, -339.1800572038740142, 348.7366044899774238 ) ) ;
#27596 = CARTESIAN_POINT ( 'NONE',  ( 799.4546378042377910, -129.0783235625963243, 356.1575198192848006 ) ) ;
#27598 = ORIENTED_EDGE ( 'NONE', *, *, #17400, .F. ) ;
#27599 = CARTESIAN_POINT ( 'NONE',  ( 755.8398074228967971, -259.4419599262322436, -333.4516893846970333 ) ) ;
#27600 = CARTESIAN_POINT ( 'NONE',  ( 805.1927285166397041, -88.81642084023842187, 341.8018195045277707 ) ) ;
#27601 = AXIS2_PLACEMENT_3D ( 'NONE', #23592, #40934, #30298 ) ;
#27602 = CARTESIAN_POINT ( 'NONE',  ( 771.2368401574024119, -253.4419599262323572, -374.2805881961240857 ) ) ;
#27603 = CARTESIAN_POINT ( 'NONE',  ( 919.9999999999993179, 154.9999999999998863, -360.0000000000000000 ) ) ;
#27604 = CARTESIAN_POINT ( 'NONE',  ( 759.8311093483677041, -382.1692326535045936, 310.9282345327691814 ) ) ;
#27605 = VERTEX_POINT ( 'NONE', #37746 ) ;
#27606 = CARTESIAN_POINT ( 'NONE',  ( 802.1676090361156639, -278.6346026584196807, 327.8955696845344505 ) ) ;
#27607 = CARTESIAN_POINT ( 'NONE',  ( 770.0799878456142551, -37.98741447168752927, -362.9823548866085616 ) ) ;
#27608 = CARTESIAN_POINT ( 'NONE',  ( 754.8072714833581358, -172.8164208402381234, -338.1981804954720587 ) ) ;
#27609 = CARTESIAN_POINT ( 'NONE',  ( 764.8639956371174549, -392.0891481129648355, 319.7806653035542013 ) ) ;
#27610 = CARTESIAN_POINT ( 'NONE',  ( 777.5031285880264704, -118.8164208402383508, -374.9108240113588408 ) ) ;
#27611 = CARTESIAN_POINT ( 'NONE',  ( 803.6646147819162707, -113.9073299311474585, -348.8264449731211130 ) ) ;
#27612 = ORIENTED_EDGE ( 'NONE', *, *, #15628, .F. ) ;
#27613 = CARTESIAN_POINT ( 'NONE',  ( 790.0220218866281812, -31.09997266333516919, -363.2186876482849129 ) ) ;
#27614 = CARTESIAN_POINT ( 'NONE',  ( 798.5707757039680246, -341.4636090269705733, -356.7845633553585003 ) ) ;
#27615 = AXIS2_PLACEMENT_3D ( 'NONE', #5501, #44310, #19595 ) ;
#27616 = CARTESIAN_POINT ( 'NONE',  ( 774.6312213355099630, -119.3618753856928691, 364.6798772138717482 ) ) ;
#27617 = CARTESIAN_POINT ( 'NONE',  ( 765.8855110935204493, -94.16923265350555994, 319.0159684113471599 ) ) ;
#27620 = CARTESIAN_POINT ( 'NONE',  ( 771.2368401574024119, -349.4419599262320162, 374.2805881961240857 ) ) ;
#27619 = CYLINDRICAL_SURFACE ( 'NONE', #40962, 10.00000000000000888 ) ;
#27618 = CARTESIAN_POINT ( 'NONE',  ( -37.63011601220122770, -365.3551492539851893, -18.13243251470705886 ) ) ;
#27621 = AXIS2_PLACEMENT_3D ( 'NONE', #13289, #41926, #44931 ) ;
#27622 = CARTESIAN_POINT ( 'NONE',  ( 754.7162404726377645, -350.7363362996978253, -339.4709603349214717 ) ) ;
#27623 = CARTESIAN_POINT ( 'NONE',  ( 805.1927285166397041, -352.8164208402374129, -341.8018195045277707 ) ) ;
#27624 = CARTESIAN_POINT ( 'NONE',  ( 760.0363995740630116, -130.9181544815166660, -368.7758568127991907 ) ) ;
#27625 = CARTESIAN_POINT ( 'NONE',  ( 757.7880784355613741, 5.990936427573807954, 312.4576283171834916 ) ) ;
#27627 = CARTESIAN_POINT ( 'NONE',  ( 911.9749999999993406, 154.9999999999998863, -360.0000000000000000 ) ) ;
#27626 = CARTESIAN_POINT ( 'NONE',  ( 999.9999999999992042, 479.5857864376268935, -200.4142135623730496 ) ) ;
#27628 = CARTESIAN_POINT ( 'NONE',  ( 756.7813123517142913, -307.9874144716866340, -329.9779781133712504 ) ) ;
#27629 = CARTESIAN_POINT ( 'NONE',  ( 795.8262568251477660, -166.3726999360620198, -308.3538107759623585 ) ) ;
#27630 = DIRECTION ( 'NONE',  ( 0.000000000000000000, -1.000000000000000000, 0.000000000000000000 ) ) ;
#27631 = DIRECTION ( 'NONE',  ( 0.000000000000000000, 0.000000000000000000, -1.000000000000000000 ) ) ;
#27632 = CARTESIAN_POINT ( 'NONE',  ( 780.5236548040995785, -332.7363362996979390, 314.9735926884559944 ) ) ;
#27633 = CLOSED_SHELL ( 'NONE', ( #3506, #10045, #35110, #32783, #6879, #13381, #34577, #12232, #27559, #14321, #2385, #2354, #36068, #36030, #41386, #44738, #30909, #37685, #44671, #9776, #7730, #24735, #17674, #17623, #22679, #13956, #13961, #30950, #29228, #17846, #38218, #27895, #43513, #32908, #6406, #12194, #30365, #4064, #33726, #12805, #3130, #44965, #24711, #40916, #19018, #992, #7773, #19347, #11135, #35440, #13666, #18504, #30925, #19876, #40501, #20930, #37996, #28831, #1539, #34339 ) ) ;
#27634 = CARTESIAN_POINT ( 'NONE',  ( 745.1792804349281596, -302.1908817542433781, 343.7566961878542884 ) ) ;
#27635 = CONICAL_SURFACE ( 'NONE', #3311, 8.024999999999948841, 0.7853981633963380560 ) ;
#27636 = CARTESIAN_POINT ( 'NONE',  ( 748.9653473494365699, -170.6346026584199933, -356.9462024416520762 ) ) ;
#27637 = CARTESIAN_POINT ( 'NONE',  ( -598.8365100919716042, 260.0000000000001705, -199.9999999999899671 ) ) ;
#27638 = AXIS2_PLACEMENT_3D ( 'NONE', #37990, #38220, #25248 ) ;
#27639 = CARTESIAN_POINT ( 'NONE',  ( 815.3608509340175488, -98.73633629969859271, 341.2497674668889545 ) ) ;
#27640 = CARTESIAN_POINT ( 'NONE',  ( 767.6429770376289525, -321.1800572038740142, -306.8695393053162093 ) ) ;
#27641 = FACE_OUTER_BOUND ( 'NONE', #19477, .T. ) ;
#27642 = DIRECTION ( 'NONE',  ( 0.000000000000000000, 0.000000000000000000, 1.000000000000000000 ) ) ;
#27643 = CARTESIAN_POINT ( 'NONE',  ( 802.1676090361156639, -182.6346026584199649, 327.8955696845344505 ) ) ;
#27644 = ORIENTED_EDGE ( 'NONE', *, *, #20206, .F. ) ;
#27645 = CARTESIAN_POINT ( 'NONE',  ( 810.4231160770870019, -408.5545181178794110, 321.9338519418446936 ) ) ;
#27646 = CARTESIAN_POINT ( 'NONE',  ( 800.1688906516307043, -370.1692326535045936, -369.0717654672308186 ) ) ;
#27647 = CARTESIAN_POINT ( 'NONE',  ( 814.9108240113580450, -136.2709662947837330, -337.5031285880265273 ) ) ;
#27648 = VECTOR ( 'NONE', #3866, 1000.000000000000000 ) ;
#27649 =( BOUNDED_CURVE ( )  B_SPLINE_CURVE ( 3, ( #21545, #982, #7697, #43255 ),
 .UNSPECIFIED., .F., .T. ) 
 B_SPLINE_CURVE_WITH_KNOTS ( ( 4, 4 ),
 ( 3.141592653589793116, 4.712388980384689674 ),
 .UNSPECIFIED. ) 
 CURVE ( )  GEOMETRIC_REPRESENTATION_ITEM ( )  RATIONAL_B_SPLINE_CURVE ( ( 1.000000000000000000, 0.8047378541243649375, 0.8047378541243649375, 1.000000000000000000 ) ) 
 REPRESENTATION_ITEM ( '' )  );
#27650 = CARTESIAN_POINT ( 'NONE',  ( 761.4292242960306112, -41.46360902697149697, 323.2154366446414429 ) ) ;
#27651 = CARTESIAN_POINT ( 'NONE',  ( 782.4968714119720516, -370.8164208402375834, -305.0891759886411023 ) ) ;
#27652 = CARTESIAN_POINT ( 'NONE',  ( 939.9999999999993179, -600.0000000000001137, -350.0000000000000000 ) ) ;
#27653 = CARTESIAN_POINT ( 'NONE',  ( 748.3538107759620743, 7.285312801039605546, 355.8262568251490165 ) ) ;
#27654 = ORIENTED_EDGE ( 'NONE', *, *, #39704, .F. ) ;
#27655 = AXIS2_PLACEMENT_3D ( 'NONE', #9818, #34978, #34751 ) ;
#27656 = VECTOR ( 'NONE', #36165, 1000.000000000000000 ) ;
#27657 = CARTESIAN_POINT ( 'NONE',  ( 812.6845335610512393, -151.9874144716871740, -353.5525998758768651 ) ) ;
#27658 = DIRECTION ( 'NONE',  ( 0.000000000000000000, 0.000000000000000000, -1.000000000000000000 ) ) ;
#27659 = CARTESIAN_POINT ( 'NONE',  ( 751.2241431872005251, -280.1692326535049347, 359.9636004259367610 ) ) ;
#27660 = CARTESIAN_POINT ( 'NONE',  ( 774.6858677611749044, -105.7255117493293000, 315.5713283507209894 ) ) ;
#27661 = ORIENTED_EDGE ( 'NONE', *, *, #14227, .F. ) ;
#27662 = SHAPE_REPRESENTATION ( 'MirrorHeavy Cast Iron Table Bed Base', ( #26858 ), #9809 ) ;
#27663 = CARTESIAN_POINT ( 'NONE',  ( 755.8398074228967971, -19.44195992623303937, -333.4516893846970333 ) ) ;
#27664 = CARTESIAN_POINT ( 'NONE',  ( 778.1981804954714335, -274.2709662947833067, 314.8072714833589885 ) ) ;
#27665 = AXIS2_PLACEMENT_3D ( 'NONE', #5888, #13282, #41229 ) ;
#27666 = CARTESIAN_POINT ( 'NONE',  ( 812.7932403749906598, -15.18005720387504631, -327.7687537140311633 ) ) ;
#27667 = AXIS2_PLACEMENT_3D ( 'NONE', #26567, #6480, #41359 ) ;
#27668 = VERTEX_POINT ( 'NONE', #27130 ) ;
#27669 = ORIENTED_EDGE ( 'NONE', *, *, #37429, .T. ) ;
#27670 = ADVANCED_BREP_SHAPE_REPRESENTATION ( '', ( #17219, #26858 ), #39435 ) ;
#27671 = CARTESIAN_POINT ( 'NONE',  ( 783.7953271457878373, -416.1908817542430938, -375.1787889125761239 ) ) ;
#27672 = VECTOR ( 'NONE', #42296, 1000.000000000000000 ) ;
#27673 = CARTESIAN_POINT ( 'NONE',  ( 803.6646147819161570, -257.9073299311469896, -348.8264449731210561 ) ) ;
#27675 = CARTESIAN_POINT ( 'NONE',  ( 748.3538107759620743, -256.7146871989595525, 355.8262568251490165 ) ) ;
#27674 = CARTESIAN_POINT ( 'NONE',  ( 767.6429770376291799, -369.1800572038739006, 306.8695393053162093 ) ) ;
#27676 = CARTESIAN_POINT ( 'NONE',  ( 813.2346286133761168, -53.26014174441475291, 328.9521613784389160 ) ) ;
#27677 = CARTESIAN_POINT ( 'NONE',  ( 802.5472867521000353, -268.3726999360616787, -350.8726784830461156 ) ) ;
#27678 = CARTESIAN_POINT ( 'NONE',  ( 785.3141322388236176, -261.7255117493288026, -364.4286716492789537 ) ) ;
#27679 = CARTESIAN_POINT ( 'NONE',  ( 803.6646147819162707, -401.9073299311464211, -348.8264449731211130 ) ) ;
#27680 = CARTESIAN_POINT ( 'NONE',  ( 755.3201227861273992, -75.72551174932937101, -345.3687786644892981 ) ) ;
#27681 = CARTESIAN_POINT ( 'NONE',  ( 797.8594530101008786, -229.5436935675106440, 322.1405469898980982 ) ) ;
#27682 = ORIENTED_EDGE ( 'NONE', *, *, #11378, .F. ) ;
#27683 = CARTESIAN_POINT ( 'NONE',  ( 749.2812353651451076, -366.4527844766012095, 323.2262854647983090 ) ) ;
#27684 = AXIS2_PLACEMENT_3D ( 'NONE', #38009, #34535, #45395 ) ;
#27685 = CARTESIAN_POINT ( 'NONE',  ( -28.63011601220122415, -513.1383975375929367, -349.9999999999999432 ) ) ;
#27686 = CARTESIAN_POINT ( 'NONE',  ( 752.7379699480933368, -60.00906357242598688, -361.9858362298580232 ) ) ;
#27687 = CARTESIAN_POINT ( 'NONE',  ( 786.4999999999993179, -512.9681489794448908, -350.0000000000000000 ) ) ;
#27688 = CARTESIAN_POINT ( 'NONE',  ( 779.9999999999992042, 16.45630643248849267, 350.0000000000000000 ) ) ;
#27689 = CARTESIAN_POINT ( 'NONE',  ( 786.5483106153019435, -223.6454272087891013, 364.1601925771022366 ) ) ;
#27690 = CARTESIAN_POINT ( 'NONE',  ( 756.3353852180819104, -125.9073299311474159, 331.1735550268788302 ) ) ;
#27691 = ADVANCED_FACE ( 'NONE', ( #41219 ), #9576, .F. ) ;
#27692 = ORIENTED_EDGE ( 'NONE', *, *, #33400, .F. ) ;
#27693 = CARTESIAN_POINT ( 'NONE',  ( 796.9571628226829034, 0.5363909730283709099, -321.2382568024804641 ) ) ;
#27694 = CARTESIAN_POINT ( 'NONE',  ( 763.2262854647970016, -56.63460265842036279, -309.2812353651462445 ) ) ;
#27695 = CARTESIAN_POINT ( 'NONE',  ( 805.0264073115434940, -294.3510508353230648, 339.4763451958999099 ) ) ;
#27696 = CARTESIAN_POINT ( 'NONE',  ( 800.2193346964447755, -426.9982390220554862, -355.1360043628815788 ) ) ;
#27697 = CARTESIAN_POINT ( 'NONE',  ( 754.8072714833583632, -52.81642084023856398, -338.1981804954721156 ) ) ;
#27698 = CARTESIAN_POINT ( 'NONE',  ( 764.1737431748507561, -10.37269993606250473, 371.6461892240376415 ) ) ;
#27699 = CARTESIAN_POINT ( 'NONE',  ( 777.5031285880264704, -190.8164208402381234, -374.9108240113588408 ) ) ;
#27700 = CARTESIAN_POINT ( 'NONE',  ( 772.5602148656447525, -177.7255117493290868, 305.7998596910095443 ) ) ;
#27701 = CARTESIAN_POINT ( 'NONE',  ( 801.9419747391806368, -90.45278447660209054, 351.9812246680014027 ) ) ;
#27702 = DIRECTION ( 'NONE',  ( 1.644774851296528363E-16, -1.000000000000000000, 0.000000000000000000 ) ) ;
#27703 = CIRCLE ( 'NONE', #26974, 6.119000000000013095 ) ;
#27704 = CARTESIAN_POINT ( 'NONE',  ( 879.9999999999990905, 479.9999999999998863, 360.0000000000000000 ) ) ;
#27705 = CARTESIAN_POINT ( 'NONE',  ( 746.0683387631852383, -283.4419599262321867, -331.3260364891676204 ) ) ;
#27706 = AXIS2_PLACEMENT_3D ( 'NONE', #32694, #14466, #1041 ) ;
#27707 = CARTESIAN_POINT ( 'NONE',  ( 757.7880784355613741, -402.0090635724250205, 312.4576283171834916 ) ) ;
#27708 = CARTESIAN_POINT ( 'NONE',  ( 745.0891759886404770, -268.2709662947833067, -342.4968714119734159 ) ) ;
#27709 = CARTESIAN_POINT ( 'NONE',  ( 939.9999999999993179, -407.8586036264139807, -201.9999999999998863 ) ) ;
#27710 = CARTESIAN_POINT ( 'NONE',  ( 767.7687537140311633, -407.9073299311465348, 372.7932403749916830 ) ) ;
#27711 = CARTESIAN_POINT ( 'NONE',  ( 801.1904061080338124, -20.08914811296593328, 368.3070685750236066 ) ) ;
#27712 = CARTESIAN_POINT ( 'NONE',  ( 778.1981804954714335, -394.2709662947827951, -314.8072714833589885 ) ) ;
#27713 = CARTESIAN_POINT ( 'NONE',  ( 787.6308680596127942, -11.26014174441488258, 364.1105419155492768 ) ) ;
#27714 = CARTESIAN_POINT ( 'NONE',  ( 748.3538107759620743, -64.71468719896019195, -355.8262568251490165 ) ) ;
#27715 = CARTESIAN_POINT ( 'NONE',  ( 759.2295555964440155, -160.1692326535053326, -353.9708237608231229 ) ) ;
#27716 = CARTESIAN_POINT ( 'NONE',  ( 746.0683387631852383, -187.4419599262325278, 331.3260364891676204 ) ) ;
#27717 = CARTESIAN_POINT ( 'NONE',  ( 759.7806653035535192, -30.99823902205680781, 324.8639956371181370 ) ) ;
#27718 = CARTESIAN_POINT ( 'NONE',  ( 791.1614460488616487, -179.2601417444143692, 373.5763878283158874 ) ) ;
#27719 = EDGE_LOOP ( 'NONE', ( #42618, #37782, #43725, #2507 ) ) ;
#27720 = CARTESIAN_POINT ( 'NONE',  ( 759.7806653035534055, -78.99823902205662307, -324.8639956371180801 ) ) ;
#27721 = CARTESIAN_POINT ( 'NONE',  ( 789.9200121543843807, -193.9874144716870319, -317.0176451133914384 ) ) ;
#27722 = CARTESIAN_POINT ( 'NONE',  ( 762.3223304703356007, -151.5436935675109851, 322.3223304703362828 ) ) ;
#27723 = EDGE_CURVE ( 'NONE', #12447, #33185, #7952, .T. ) ;
#27724 = VECTOR ( 'NONE', #38477, 1000.000000000000000 ) ;
#27725 = CARTESIAN_POINT ( 'NONE',  ( 813.9316612368132837, 16.55804007376685050, -348.6739635108323228 ) ) ;
#27726 = CARTESIAN_POINT ( 'NONE',  ( 774.6312213355098493, -287.3618753856923718, 364.6798772138717482 ) ) ;
#27727 = CARTESIAN_POINT ( 'NONE',  ( 187.1337867209877857, -428.4497686941065808, -352.6378164459125060 ) ) ;
#27728 = ORIENTED_EDGE ( 'NONE', *, *, #28642, .F. ) ;
#27729 = CARTESIAN_POINT ( 'NONE',  ( 784.0799538623451781, -11.80559628986942577, 364.6971507214555572 ) ) ;
#27730 = CARTESIAN_POINT ( 'NONE',  ( 814.4686193811664907, -291.2817908451525000, -346.2056067578752732 ) ) ;
#27731 = CARTESIAN_POINT ( 'NONE',  ( 772.4837098697145166, -263.3618753856924286, 374.5518280994205611 ) ) ;
#27732 = CARTESIAN_POINT ( 'NONE',  ( 790.0220218866281812, -343.0999726633342561, 363.2186876482849129 ) ) ;
#27733 = CARTESIAN_POINT ( 'NONE',  ( 801.9858362298568863, 20.92167643740319605, 312.7379699480935642 ) ) ;
#27734 = CARTESIAN_POINT ( 'NONE',  ( 759.0159684113467620, -136.9181544815166376, -325.8855110935213020 ) ) ;
#27735 = CARTESIAN_POINT ( 'NONE',  ( 758.0580252608178853, -150.4527844766018916, -328.0187753319985404 ) ) ;
#27736 = CARTESIAN_POINT ( 'NONE',  ( 771.1735550268780344, -321.1800572038740711, -316.3353852180828198 ) ) ;
#27737 = ORIENTED_EDGE ( 'NONE', *, *, #21115, .T. ) ;
#27738 = AXIS2_PLACEMENT_3D ( 'NONE', #37042, #5181, #23166 ) ;
#27739 = CARTESIAN_POINT ( 'NONE',  ( 766.7756240680305382, -326.5328690171411381, 361.5560724626415663 ) ) ;
#27740 = VECTOR ( 'NONE', #42858, 1000.000000000000000 ) ;
#27741 = CARTESIAN_POINT ( 'NONE',  ( 175.6195620086261613, 290.0000000000001137, -244.9999999999999716 ) ) ;
#27742 = CARTESIAN_POINT ( 'NONE',  ( 769.0155153010367712, -106.3726999360621903, 362.7791456095907279 ) ) ;
#27743 = CARTESIAN_POINT ( 'NONE',  ( 771.2633955100217236, 0.09267006885218045942, 363.4237431249939618 ) ) ;
#27744 = EDGE_CURVE ( 'NONE', #7984, #35816, #24794, .T. ) ;
#27745 = VERTEX_POINT ( 'NONE', #17657 ) ;
#27746 = CARTESIAN_POINT ( 'NONE',  ( 811.3240766477731540, -364.3726999360614514, -355.6651683502462902 ) ) ;
#27747 = CYLINDRICAL_SURFACE ( 'NONE', #23221, 10.00000000000006395 ) ;
#27748 = CARTESIAN_POINT ( 'NONE',  ( 804.1009440267234822, -239.4636090269709143, 314.0944755984392600 ) ) ;
#27749 = CARTESIAN_POINT ( 'NONE',  ( 800.7704444035546203, -196.1692326535052473, 326.0291762391768771 ) ) ;
#27750 = CARTESIAN_POINT ( 'NONE',  ( 759.9864689768902508, -314.0891481129650629, -354.9819416627836404 ) ) ;
#27751 = SURFACE_SIDE_STYLE ('',( #20804 ) ) ;
#27752 = CARTESIAN_POINT ( 'NONE',  ( 757.4527132478984868, -232.3726999360617924, -329.1273215169538844 ) ) ;
#27753 = AXIS2_PLACEMENT_3D ( 'NONE', #28883, #33049, #36263 ) ;
#27754 = CARTESIAN_POINT ( 'NONE',  ( 782.5225473063381969, -70.27096629478397460, 375.2698199232970637 ) ) ;
#27755 = CARTESIAN_POINT ( 'NONE',  ( 51.16348990802859475, 240.0000000000000568, -199.9999999999945146 ) ) ;
#27756 = CARTESIAN_POINT ( 'NONE',  ( 811.0346526505617248, -422.6346026584191691, -323.0537975583478101 ) ) ;
#27757 = LINE ( 'NONE', #34910, #4763 ) ;
#27758 = CARTESIAN_POINT ( 'NONE',  ( 781.2370466360911223, -356.7363362996978253, 304.9990715423533629 ) ) ;
#27759 = DIRECTION ( 'NONE',  ( -1.000000000000000000, -0.000000000000000000, -0.000000000000000000 ) ) ;
#27760 = CARTESIAN_POINT ( 'NONE',  ( 772.5602148656447525, -297.7255117493286889, 305.7998596910095443 ) ) ;
#27761 = CARTESIAN_POINT ( 'NONE',  ( 808.0189434323515343, -62.08914811296580183, -319.0252816721025511 ) ) ;
#27762 = CARTESIAN_POINT ( 'NONE',  ( 804.4286716492782716, -281.3618753856923718, -345.3141322388244703 ) ) ;
#27763 = EDGE_CURVE ( 'NONE', #29887, #8835, #35637, .T. ) ;
#27764 = CARTESIAN_POINT ( 'NONE',  ( 187.1337867209877857, 62.85347435602256638, 357.4246812887967053 ) ) ;
#27765 = CARTESIAN_POINT ( 'NONE',  ( 801.9419747391806368, -378.4527844766011526, 351.9812246680014027 ) ) ;
#27766 = CARTESIAN_POINT ( 'NONE',  ( 761.4292242960306112, -161.4636090269711133, 323.2154366446414429 ) ) ;
#27767 = CARTESIAN_POINT ( 'NONE',  ( 744.6391490659812007, -14.73633629969885384, -338.7502325331110455 ) ) ;
#27768 = CARTESIAN_POINT ( 'NONE',  ( 754.9735926884551418, -66.35105083532378956, -340.5236548041000333 ) ) ;
#27769 = CARTESIAN_POINT ( 'NONE',  ( 752.4576283171824116, -69.07832356259653750, 317.7880784355627952 ) ) ;
#27770 = CARTESIAN_POINT ( 'NONE',  ( 771.2633955100217236, -383.9073299311466485, 363.4237431249939618 ) ) ;
#27771 = CYLINDRICAL_SURFACE ( 'NONE', #9983, 30.00000000000008171 ) ;
#27772 = CARTESIAN_POINT ( 'NONE',  ( 768.0187753319979720, -416.6346026584192259, 318.0580252608186242 ) ) ;
#27773 = ORIENTED_EDGE ( 'NONE', *, *, #7148, .T. ) ;
#27774 = CARTESIAN_POINT ( 'NONE',  ( 781.8018195045266339, -70.27096629478397460, -365.1927285166406705 ) ) ;
#27775 = EDGE_CURVE ( 'NONE', #44488, #24071, #15039, .T. ) ;
#27776 = VECTOR ( 'NONE', #26082, 1000.000000000000000 ) ;
#27777 = ADVANCED_FACE ( 'NONE', ( #35882 ), #4474, .F. ) ;
#27778 = CARTESIAN_POINT ( 'NONE',  ( 786.6156483768007774, -361.4419599262319593, -315.5913626894246136 ) ) ;
#27780 = CARTESIAN_POINT ( 'NONE',  ( 801.9419747391806368, -186.4527844766017779, 351.9812246680014027 ) ) ;
#27779 = CARTESIAN_POINT ( 'NONE',  ( 800.0135310231082713, -230.0891481129652618, 325.0180583372163028 ) ) ;
#27781 = VECTOR ( 'NONE', #4801, 1000.000000000000000 ) ;
#27782 = CARTESIAN_POINT ( 'NONE',  ( 793.4146539503750546, -385.9874144716864066, -307.6481478633938877 ) ) ;
#27783 = DIRECTION ( 'NONE',  ( -1.000000000000000000, 0.000000000000000000, 0.000000000000000000 ) ) ;
#27784 = ORIENTED_EDGE ( 'NONE', *, *, #26959, .T. ) ;
#27785 = CARTESIAN_POINT ( 'NONE',  ( 803.6646147819161570, -377.9073299311466485, 348.8264449731210561 ) ) ;
#27786 = AXIS2_PLACEMENT_3D ( 'NONE', #5583, #4910, #5346 ) ;
#27787 = ORIENTED_EDGE ( 'NONE', *, *, #34861, .T. ) ;
#27788 = VECTOR ( 'NONE', #26269, 1000.000000000000000 ) ;
#27789 = CARTESIAN_POINT ( 'NONE',  ( 811.0346526505616112, -230.6346026584197659, -323.0537975583477532 ) ) ;
#27790 = CARTESIAN_POINT ( 'NONE',  ( 767.6429770376291799, -153.1800572038746111, 306.8695393053162093 ) ) ;
#27791 = EDGE_LOOP ( 'NONE', ( #17806, #25741, #44292, #11488 ) ) ;
#27792 = CARTESIAN_POINT ( 'NONE',  ( 773.7943932421234194, -191.8055962898689017, 305.5313806188329409 ) ) ;
#27793 = CARTESIAN_POINT ( 'NONE',  ( 764.8639956371174549, -224.0891481129652902, -319.7806653035542581 ) ) ;
#27794 = ORIENTED_EDGE ( 'NONE', *, *, #10834, .T. ) ;
#27795 = EDGE_CURVE ( 'NONE', #1032, #42107, #4257, .T. ) ;
#27796 = CARTESIAN_POINT ( 'NONE',  ( 805.1927285166397041, -376.8164208402375834, -341.8018195045277707 ) ) ;
#27797 = CARTESIAN_POINT ( 'NONE',  ( 804.9363028652555840, -16.27096629478413092, -338.2165204200192079 ) ) ;
#27798 = EDGE_CURVE ( 'NONE', #14856, #24787, #14416, .T. ) ;
#27799 = CARTESIAN_POINT ( 'NONE',  ( 795.9930595647434757, -243.0783235625959833, 320.7433823573372820 ) ) ;
#27800 = CARTESIAN_POINT ( 'NONE',  ( 879.9999999999992042, 259.9999999999998863, -219.9999999999999716 ) ) ;
#27801 = CARTESIAN_POINT ( 'NONE',  ( -454.7528517110261532, 8.550106180308601742E-14, 350.0000000000000000 ) ) ;
#27802 = ORIENTED_EDGE ( 'NONE', *, *, #3160, .F. ) ;
#27803 = CARTESIAN_POINT ( 'NONE',  ( 778.2165204200184689, 1.183579159761269040, -364.9363028652563230 ) ) ;
#27804 = LINE ( 'NONE', #10468, #40997 ) ;
#27805 = LINE ( 'NONE', #34953, #12289 ) ;
#27806 = EDGE_CURVE ( 'NONE', #2064, #7404, #32191, .T. ) ;
#27807 = CARTESIAN_POINT ( 'NONE',  ( 755.8990559732751535, -275.4636090269708575, -365.9055244015606831 ) ) ;
#27808 = CARTESIAN_POINT ( 'NONE',  ( 814.2805881961230625, -121.6454272087894282, 331.2368401574024119 ) ) ;
#27810 = CARTESIAN_POINT ( 'NONE',  ( 781.7834795799800531, -226.8164208402380098, -315.0636971347436202 ) ) ;
#27809 = LINE ( 'NONE', #45370, #37908 ) ;
#27811 = CARTESIAN_POINT ( 'NONE',  ( 804.9511171171677688, -389.8055962898682765, -335.8780910478229202 ) ) ;
#27812 = DIRECTION ( 'NONE',  ( -0.000000000000000000, 1.000000000000000000, -0.000000000000000000 ) ) ;
#27813 = CARTESIAN_POINT ( 'NONE',  ( 764.8639956371174549, 15.91085188703394593, -319.7806653035542581 ) ) ;
#27814 = CARTESIAN_POINT ( 'NONE',  ( 804.4086373105744769, -97.64542720878949922, -333.3843516231986541 ) ) ;
#27815 = CIRCLE ( 'NONE', #3487, 10.00000000000000888 ) ;
#27816 = CARTESIAN_POINT ( 'NONE',  ( 802.2119215644370342, -390.0090635724249069, 367.5423716828165084 ) ) ;
#27817 = CARTESIAN_POINT ( 'NONE',  ( 1007.605605532488426, 323.4107432173689176, 352.9408934102648345 ) ) ;
#27818 = CARTESIAN_POINT ( 'NONE',  ( 744.9990715423526808, 5.648949164675971524, -341.2370466360926002 ) ) ;
#27819 = CARTESIAN_POINT ( 'NONE',  ( 801.1904061080338124, -308.0891481129650629, -368.3070685750236066 ) ) ;
#27820 = FACE_OUTER_BOUND ( 'NONE', #33311, .T. ) ;
#27821 = LINE ( 'NONE', #41230, #1033 ) ;
#27822 = CARTESIAN_POINT ( 'NONE',  ( 759.9864689768902508, -74.08914811296577341, -354.9819416627836404 ) ) ;
#27823 = AXIS2_PLACEMENT_3D ( 'NONE', #19474, #16026, #6071 ) ;
#27824 = EDGE_CURVE ( 'NONE', #338, #33957, #43794, .T. ) ;
#27825 = CARTESIAN_POINT ( 'NONE',  ( 786.2694204179717872, -237.2817908451526421, 305.1769319972829067 ) ) ;
#27826 = CARTESIAN_POINT ( 'NONE',  ( 748.3538107759620743, -184.7146871989598083, -355.8262568251490165 ) ) ;
#27827 = CARTESIAN_POINT ( 'NONE',  ( 777.4774526936600978, -202.2709662947834772, 304.7301800767027657 ) ) ;
#27828 = CARTESIAN_POINT ( 'NONE',  ( 745.7998596910086917, -437.3618753856919170, -332.5602148656461168 ) ) ;
#27829 = VECTOR ( 'NONE', #26651, 1000.000000000000000 ) ;
#27830 = LINE ( 'NONE', #13751, #44574 ) ;
#27831 = EDGE_CURVE ( 'NONE', #22606, #39117, #3254, .T. ) ;
#27832 = CARTESIAN_POINT ( 'NONE',  ( 805.1927285166397041, -280.8164208402378677, 341.8018195045277707 ) ) ;
#27833 = CARTESIAN_POINT ( 'NONE',  ( 766.9102291470427417, -66.55451811788050520, 318.6633372737382501 ) ) ;
#27834 = CARTESIAN_POINT ( 'NONE',  ( 757.8323909638827445, -434.6346026584190554, -352.1044303154654358 ) ) ;
#27835 = CARTESIAN_POINT ( 'NONE',  ( -789.9999999999992042, 205.0000000000000568, -339.9999999999999432 ) ) ;
#27836 = PLANE ( 'NONE',  #44630 ) ;
#27838 = CARTESIAN_POINT ( 'NONE',  ( 795.1360043628807261, -332.0891481129649492, 360.2193346964456282 ) ) ;
#27837 = CARTESIAN_POINT ( 'NONE',  ( 801.3366627262608972, -128.5328690171417634, 353.0897708529566899 ) ) ;
#27839 = EDGE_LOOP ( 'NONE', ( #15080, #24834, #13662, #8816 ) ) ;
#27840 = EDGE_CURVE ( 'NONE', #20535, #5169, #22232, .T. ) ;
#27841 = CARTESIAN_POINT ( 'NONE',  ( 784.0799538623451781, -251.8055962898686744, -364.6971507214555572 ) ) ;
#27842 = CARTESIAN_POINT ( 'NONE',  ( 765.0180583372156207, -96.99823902205660886, 360.0135310231089534 ) ) ;
#27843 = CARTESIAN_POINT ( 'NONE',  ( 783.7566961878529810, -264.8965053807776826, -305.1792804349288417 ) ) ;
#27844 = CARTESIAN_POINT ( 'NONE',  ( 794.9999999999993179, 205.0000000000000568, -235.0000000000000000 ) ) ;
#27845 = CARTESIAN_POINT ( 'NONE',  ( 811.6461892240364477, -412.7146871989590409, 324.1737431748509835 ) ) ;
#27846 = ORIENTED_EDGE ( 'NONE', *, *, #7195, .T. ) ;
#27847 = CARTESIAN_POINT ( 'NONE',  ( 794.9819416627830151, -276.9982390220559978, 319.9864689768909898 ) ) ;
#27848 = CARTESIAN_POINT ( 'NONE',  ( 803.2186876482843445, -31.98741447168754348, -350.0220218866286928 ) ) ;
#27849 = CARTESIAN_POINT ( 'NONE',  ( 758.0580252608178853, -150.4527844766018916, -328.0187753319985404 ) ) ;
#27850 = CARTESIAN_POINT ( 'NONE',  ( 768.0187753319979720, -200.6346026584199365, -318.0580252608186242 ) ) ;
#27851 = CARTESIAN_POINT ( 'NONE',  ( 804.4286716492782716, -401.3618753856920307, 345.3141322388244703 ) ) ;
#27852 = CARTESIAN_POINT ( 'NONE',  ( 749.2812353651451076, -126.4527844766019626, -323.2262854647983090 ) ) ;
#27853 = APPLICATION_CONTEXT ( 'automotive_design' ) ;
#27854 = CARTESIAN_POINT ( 'NONE',  ( 788.8264449731201466, -93.18005720387479585, -363.6646147819170665 ) ) ;
#27855 = VERTEX_POINT ( 'NONE', #36329 ) ;
#27856 = CARTESIAN_POINT ( 'NONE',  ( 804.6971507214547046, -51.28179084515328867, -344.0799538623459739 ) ) ;
#27857 = AXIS2_PLACEMENT_3D ( 'NONE', #18542, #32621, #40463 ) ;
#27858 = CARTESIAN_POINT ( 'NONE',  ( 760.7433823573367135, -396.0090635724249637, -355.9930595647440441 ) ) ;
#27860 = CARTESIAN_POINT ( 'NONE',  ( 805.2837595273609850, -434.7363362996975980, 340.5290396650784714 ) ) ;
#27859 = CARTESIAN_POINT ( 'NONE',  ( 759.9864689768902508, -122.0891481129656171, 354.9819416627836404 ) ) ;
#27861 = CARTESIAN_POINT ( 'NONE',  ( 790.8726784830453198, -106.7146871989600498, 362.5472867521010585 ) ) ;
#27864 = CARTESIAN_POINT ( 'NONE',  ( 747.3154664389472828, -355.9874144716865203, 326.4474001241230781 ) ) ;
#27863 = CYLINDRICAL_SURFACE ( 'NONE', #22523, 6.119000000000013095 ) ;
#27862 = CARTESIAN_POINT ( 'NONE',  ( 799.9999999999993179, -365.3551492539851893, 18.13243251470705886 ) ) ;
#27865 = ORIENTED_EDGE ( 'NONE', *, *, #20953, .F. ) ;
#27866 = CARTESIAN_POINT ( 'NONE',  ( 804.6971507214547046, -363.2817908451523294, -344.0799538623459739 ) ) ;
#27867 = CARTESIAN_POINT ( 'NONE',  ( 774.6312213355099630, -359.3618753856920875, -364.6798772138717482 ) ) ;
#27868 = CARTESIAN_POINT ( 'NONE',  ( 745.5313806188320314, -159.2817908451529547, -333.7943932421247268 ) ) ;
#27869 = CARTESIAN_POINT ( 'NONE',  ( 815.3608509340175488, -50.73633629969874193, 341.2497674668889545 ) ) ;
#27871 = CARTESIAN_POINT ( 'NONE',  ( 999.9999999999992042, -599.0000000000001137, 359.0000000000000000 ) ) ;
#27870 = DIRECTION ( 'NONE',  ( 0.000000000000000000, 0.000000000000000000, 1.000000000000000000 ) ) ;
#27872 = CARTESIAN_POINT ( 'NONE',  ( 770.0799878456142551, -277.9874144716867477, -362.9823548866085616 ) ) ;
#27873 = CARTESIAN_POINT ( 'NONE',  ( 756.5762568750052424, -435.1800572038737869, -348.7366044899774238 ) ) ;
#27874 = CARTESIAN_POINT ( 'NONE',  ( 811.3240766477731540, -148.3726999360620198, -355.6651683502462902 ) ) ;
#27875 = DIRECTION ( 'NONE',  ( 0.000000000000000000, 0.000000000000000000, 1.000000000000000000 ) ) ;
#27876 = DIRECTION ( 'NONE',  ( 0.000000000000000000, 0.000000000000000000, 1.000000000000000000 ) ) ;
#27877 = CARTESIAN_POINT ( 'NONE',  ( 754.7162404726377645, -350.7363362996978253, 339.4709603349214717 ) ) ;
#27878 = CARTESIAN_POINT ( 'NONE',  ( 745.5313806188320314, -351.2817908451523294, 333.7943932421247268 ) ) ;
#27879 = CARTESIAN_POINT ( 'NONE',  ( 772.4837098697145166, -167.3618753856927412, -374.5518280994205611 ) ) ;
#27880 = DIRECTION ( 'NONE',  ( 0.000000000000000000, 0.000000000000000000, -1.000000000000000000 ) ) ;
#27881 = EDGE_CURVE ( 'NONE', #7575, #7469, #553, .T. ) ;
#27882 = CARTESIAN_POINT ( 'NONE',  ( 811.3240766477731540, -124.3726999360621619, 355.6651683502462902 ) ) ;
#27883 = CARTESIAN_POINT ( 'NONE',  ( 772.4837098697144029, -311.3618753856922581, -374.5518280994205611 ) ) ;
#27884 = CARTESIAN_POINT ( 'NONE',  ( -775.4999999999993179, -365.3551492539851893, -18.13243251470705886 ) ) ;
#27885 = CARTESIAN_POINT ( 'NONE',  ( 831.1634899080286232, 259.9999999999998863, -199.9999999999999432 ) ) ;
#27886 = CARTESIAN_POINT ( 'NONE',  ( 764.8639956371174549, -176.0891481129653755, 319.7806653035542013 ) ) ;
#27887 = CARTESIAN_POINT ( 'NONE',  ( 812.3518521366052028, -409.0999726633340288, 326.5853460496235243 ) ) ;
#27888 = CARTESIAN_POINT ( 'NONE',  ( 773.7943932421234194, -383.8055962898682765, -305.5313806188329409 ) ) ;
#27889 = VECTOR ( 'NONE', #754, 1000.000000000000000 ) ;
#27890 = CARTESIAN_POINT ( 'NONE',  ( 804.7487373415286811, -139.5436935675110135, -364.7487373415288516 ) ) ;
#27891 = CARTESIAN_POINT ( 'NONE',  ( 745.4481719005789273, -387.7255117493283478, -347.5162901302853129 ) ) ;
#27892 = DIRECTION ( 'NONE',  ( 1.000000000000000000, 4.625929269271485914E-16, 0.000000000000000000 ) ) ;
#27893 = CARTESIAN_POINT ( 'NONE',  ( 801.9858362298568863, -3.078323562596726681, 312.7379699480935642 ) ) ;
#27894 = ORIENTED_EDGE ( 'NONE', *, *, #5789, .T. ) ;
#27895 = ADVANCED_FACE ( 'NONE', ( #21788 ), #3783, .T. ) ;
#27896 = CARTESIAN_POINT ( 'NONE',  ( 813.9316612368132837, -151.4419599262326415, -348.6739635108323228 ) ) ;
#27897 = DIRECTION ( 'NONE',  ( 1.000000000000000000, 0.000000000000000000, 0.000000000000000000 ) ) ;
#27898 = CARTESIAN_POINT ( 'NONE',  ( 752.4576283171824116, -309.0783235625957559, 317.7880784355627952 ) ) ;
#27899 = CARTESIAN_POINT ( 'NONE',  ( 765.0180583372156207, -120.9982390220565378, 360.0135310231089534 ) ) ;
#27900 = EDGE_LOOP ( 'NONE', ( #4503, #3503, #30812, #42746 ) ) ;
#27901 = CARTESIAN_POINT ( 'NONE',  ( 791.9812246680005501, -308.6346026584195670, 361.9419747391813189 ) ) ;
#27902 = CARTESIAN_POINT ( 'NONE',  ( 767.7687537140311633, -23.90732993114773919, -372.7932403749916830 ) ) ;
#27903 = DIRECTION ( 'NONE',  ( -1.000000000000000000, -0.000000000000000000, -0.000000000000000000 ) ) ;
#27904 = VERTEX_POINT ( 'NONE', #25481 ) ;
#27905 = CARTESIAN_POINT ( 'NONE',  ( 807.2620300519052989, -408.0090635724249069, -318.0141637701419768 ) ) ;
#27906 = ORIENTED_EDGE ( 'NONE', *, *, #39475, .T. ) ;
#27907 = CARTESIAN_POINT ( 'NONE',  ( 800.0135310231082713, -14.08914811296595460, 325.0180583372163028 ) ) ;
#27908 = CARTESIAN_POINT ( 'NONE',  ( 774.6312213355099630, -263.3618753856924855, -364.6798772138717482 ) ) ;
#27910 = CARTESIAN_POINT ( 'NONE',  ( 745.1769319972822814, -257.8055962898686744, 346.2694204179732083 ) ) ;
#27909 = CARTESIAN_POINT ( 'NONE',  ( 814.9108240113580450, -376.2709662947829656, 337.5031285880265273 ) ) ;
#27911 = CARTESIAN_POINT ( 'NONE',  ( 775.8780910478218402, -249.2817908451526421, -364.9511171171680530 ) ) ;
#27912 = CARTESIAN_POINT ( 'NONE',  ( 756.3353852180819104, -269.9073299311468190, -331.1735550268788302 ) ) ;
#27913 = CARTESIAN_POINT ( 'NONE',  ( -208.8365100919714052, 230.0000000000000853, -199.9999999999926956 ) ) ;
#27914 = CARTESIAN_POINT ( 'NONE',  ( 765.0180583372156207, -72.99823902205667991, -360.0135310231089534 ) ) ;
#27915 = CARTESIAN_POINT ( 'NONE',  ( 756.3353852180819104, -245.9073299311469896, 331.1735550268788302 ) ) ;
#27916 = ORIENTED_EDGE ( 'NONE', *, *, #13757, .F. ) ;
#27917 = VECTOR ( 'NONE', #42727, 1000.000000000000000 ) ;
#27918 = CARTESIAN_POINT ( 'NONE',  ( 814.9108240113580450, -400.2709662947828519, 337.5031285880265273 ) ) ;
#27919 = DIRECTION ( 'NONE',  ( 1.000000000000000000, 0.000000000000000000, 0.000000000000000000 ) ) ;
#27920 = CARTESIAN_POINT ( 'NONE',  ( 809.0717654672305343, -52.91815448151692891, -360.1688906516309885 ) ) ;
#27921 = DIRECTION ( 'NONE',  ( -1.000000000000000000, -0.000000000000000000, -0.000000000000000000 ) ) ;
#27922 = FACE_BOUND ( 'NONE', #25269, .T. ) ;
#27923 = CARTESIAN_POINT ( 'NONE',  ( 784.1219089521767955, -237.2817908451526421, 315.0488828828318333 ) ) ;
#27924 = CARTESIAN_POINT ( 'NONE',  ( 757.8323909638827445, -122.6346026584201354, 352.1044303154654358 ) ) ;
#27925 = VERTEX_POINT ( 'NONE', #15095 ) ;
#27926 = CARTESIAN_POINT ( 'NONE',  ( 793.0897708529556667, -6.554518117880697048, -361.3366627262616362 ) ) ;
#27927 = CARTESIAN_POINT ( 'NONE',  ( 745.0891759886404770, -76.27096629478394618, -342.4968714119734159 ) ) ;
#27928 = CARTESIAN_POINT ( 'NONE',  ( 761.2382568024794409, -303.6237781080503169, 356.9571628226838129 ) ) ;
#27929 = CARTESIAN_POINT ( 'NONE',  ( 801.9419747391806368, -426.4527844766010389, -351.9812246680014027 ) ) ;
#27930 = CARTESIAN_POINT ( 'NONE',  ( 776.2046728542105711, -20.19088175424429110, 304.8212110874238761 ) ) ;
#27931 = CARTESIAN_POINT ( 'NONE',  ( 792.3570229623688874, -213.1800572038743553, -373.1304606946836202 ) ) ;
#27932 = CARTESIAN_POINT ( 'NONE',  ( 755.3201227861273992, -75.72551174932937101, 345.3687786644892981 ) ) ;
#27933 = CARTESIAN_POINT ( 'NONE',  ( -190.7583438952258916, 294.6698570112193920, -244.9999999999999716 ) ) ;
#27934 = CARTESIAN_POINT ( 'NONE',  ( 747.3154664389472828, -259.9874144716869182, -326.4474001241230781 ) ) ;
#27935 = CARTESIAN_POINT ( 'NONE',  ( 748.6759233522253680, -400.3726999360612808, 324.3348316497537098 ) ) ;
#27936 = CARTESIAN_POINT ( 'NONE',  ( 745.7998596910086917, -293.3618753856923718, -332.5602148656461168 ) ) ;
#27937 = CARTESIAN_POINT ( 'NONE',  ( 919.9999999999993179, 219.9999999999998863, 350.0000000000000000 ) ) ;
#27938 = CARTESIAN_POINT ( 'NONE',  ( 805.0264073115434940, -366.3510508353228374, 339.4763451958999099 ) ) ;
#27939 = CARTESIAN_POINT ( 'NONE',  ( 746.8695393053151292, -53.90732993114765037, 327.6429770376306578 ) ) ;
#27940 = CARTESIAN_POINT ( 'NONE',  ( 785.3687786644884454, -371.3618753856919739, -315.3201227861279676 ) ) ;
#27941 = CARTESIAN_POINT ( 'NONE',  ( 805.0264073115434940, -6.351050835323991173, 339.4763451958999099 ) ) ;
#27942 = CARTESIAN_POINT ( 'NONE',  ( 802.1676090361156639, -206.6346026584198512, -327.8955696845344505 ) ) ;
#27943 = CARTESIAN_POINT ( 'NONE',  ( 744.8212110874229666, -42.89650538077842157, -336.2046728542121627 ) ) ;
#27944 = CARTESIAN_POINT ( 'NONE',  ( 764.0069404352550464, -183.0783235625961538, -359.2566176426627180 ) ) ;
#27945 = CARTESIAN_POINT ( 'NONE',  ( 788.7631598425961101, -169.4419599262325562, 305.7194118038759143 ) ) ;
#27946 = CARTESIAN_POINT ( 'NONE',  ( 804.4286716492782716, -17.36187538569322086, 345.3141322388244703 ) ) ;
#27947 = CIRCLE ( 'NONE', #33847, 8.024999999999948841 ) ;
#27948 = ORIENTED_EDGE ( 'NONE', *, *, #42431, .T. ) ;
#27949 = CARTESIAN_POINT ( 'NONE',  ( 783.0433043558608688, -192.8965053807779668, -315.1538015810313027 ) ) ;
#27950 = CARTESIAN_POINT ( 'NONE',  ( 792.1044303154645831, -204.4527844766016926, 317.8323909638837677 ) ) ;
#27951 = CARTESIAN_POINT ( 'NONE',  ( 744.9990715423526808, -42.35105083532388193, -341.2370466360926002 ) ) ;
#27952 = CARTESIAN_POINT ( 'NONE',  ( 771.1735550268780344, -321.1800572038740711, 316.3353852180828198 ) ) ;
#27953 = DIRECTION ( 'NONE',  ( -0.000000000000000000, 1.000000000000000000, -0.000000000000000000 ) ) ;
#27954 = ORIENTED_EDGE ( 'NONE', *, *, #25526, .T. ) ;
#27955 = CARTESIAN_POINT ( 'NONE',  ( 769.1273215169530886, -46.71468719896022748, 317.4527132478988847 ) ) ;
#27956 = CARTESIAN_POINT ( 'NONE',  ( 754.3581564841646241, -305.4636090269706870, -316.1443688327762516 ) ) ;
#27957 = CARTESIAN_POINT ( 'NONE',  ( 767.6429770376291799, -273.1800572038742985, 306.8695393053162093 ) ) ;
#27958 = CARTESIAN_POINT ( 'NONE',  ( 804.6971507214547046, -339.2817908451524431, 344.0799538623459739 ) ) ;
#27959 = CARTESIAN_POINT ( 'NONE',  ( 778.7502325331095108, 23.64894916467591912, 304.6391490659818828 ) ) ;
#27960 = CARTESIAN_POINT ( 'NONE',  ( 776.9254006560222479, -140.1908817542438896, -314.8983024940802125 ) ) ;
#27961 = CARTESIAN_POINT ( 'NONE',  ( 795.1360043628807261, -140.0891481129654892, -360.2193346964456282 ) ) ;
#27962 = CARTESIAN_POINT ( 'NONE',  ( 785.3141322388236176, -333.7255117493286320, -364.4286716492789537 ) ) ;
#27963 = VERTEX_POINT ( 'NONE', #10954 ) ;
#27964 = CARTESIAN_POINT ( 'NONE',  ( 782.4968714119720516, -250.8164208402379245, 305.0891759886411023 ) ) ;
#27965 = CARTESIAN_POINT ( 'NONE',  ( 805.1016975059191054, -342.8965053807773984, 343.0745993439771837 ) ) ;
#27966 = DIRECTION ( 'NONE',  ( -1.000000000000000000, -0.000000000000000000, -0.000000000000000000 ) ) ;
#27967 = CARTESIAN_POINT ( 'NONE',  ( 755.8894580844503253, -111.8272453906076151, 332.3691319403863531 ) ) ;
#27968 = CARTESIAN_POINT ( 'NONE',  ( 771.1735550268778070, -9.180057203875058747, 316.3353852180827630 ) ) ;
#27969 = ORIENTED_EDGE ( 'NONE', *, *, #31676, .F. ) ;
#27970 = CARTESIAN_POINT ( 'NONE',  ( 793.5525998758768083, -367.0999726633342561, -372.6845335610516941 ) ) ;
#27971 = DIRECTION ( 'NONE',  ( 0.000000000000000000, 0.000000000000000000, 1.000000000000000000 ) ) ;
#27972 = CARTESIAN_POINT ( 'NONE',  ( 814.4686193811664907, -243.2817908451526705, 346.2056067578752732 ) ) ;
#27973 = CIRCLE ( 'NONE', #45674, 20.00000000000001776 ) ;
#27974 = CARTESIAN_POINT ( 'NONE',  ( 801.3366627262608972, -176.5328690171416213, 353.0897708529566899 ) ) ;
#27975 = CARTESIAN_POINT ( 'NONE',  ( 778.2165204200184689, -310.8164208402377540, -364.9363028652563230 ) ) ;
#27976 = CARTESIAN_POINT ( 'NONE',  ( 773.4999999999993179, -512.9681489794448908, -329.9999999999999432 ) ) ;
#27977 = CARTESIAN_POINT ( 'NONE',  ( 787.5531968255692163, -213.8272453906073167, -316.1348686366205811 ) ) ;
#27978 = CARTESIAN_POINT ( 'NONE',  ( 763.0537975583475827, -24.45278447660229304, 371.0346526505627480 ) ) ;
#27979 = CARTESIAN_POINT ( 'NONE',  ( 751.6929314249748586, -78.99823902205662307, 318.8095938919659034 ) ) ;
#27980 = CARTESIAN_POINT ( 'NONE',  ( 809.1994704715707485, -452.9681489794448908, 335.3884333643831042 ) ) ;
#27981 = CARTESIAN_POINT ( 'NONE',  ( 814.9108240113580450, -424.2709662947829088, -337.5031285880265273 ) ) ;
#27982 = CARTESIAN_POINT ( 'NONE',  ( -26.63011601220122060, -365.3551492539851893, -28.13243251470704109 ) ) ;
#27983 = CARTESIAN_POINT ( 'NONE',  ( 797.8822607201568644, -342.5545181178796952, 370.1134526219340160 ) ) ;
#27984 = CARTESIAN_POINT ( 'NONE',  ( 794.9999999999993179, 240.0000000000000284, -275.0000000000000000 ) ) ;
#27985 = CARTESIAN_POINT ( 'NONE',  ( 746.8695393053150156, -317.9073299311468190, 327.6429770376306010 ) ) ;
#27986 = CARTESIAN_POINT ( 'NONE',  ( 792.3570229623688874, -69.18005720387488111, -373.1304606946836202 ) ) ;
#27987 = CARTESIAN_POINT ( 'NONE',  ( 778.1981804954714335, -298.2709662947830793, -314.8072714833589885 ) ) ;
#27988 = FACE_OUTER_BOUND ( 'NONE', #33809, .T. ) ;
#27989 = CARTESIAN_POINT ( 'NONE',  ( 800.2193346964447755, -378.9982390220555999, 355.1360043628815788 ) ) ;
#27990 = CARTESIAN_POINT ( 'NONE',  ( 802.9823548866075953, -145.0999726633347677, 330.0799878456151077 ) ) ;
#27991 = CARTESIAN_POINT ( 'NONE',  ( 814.4686193811664907, -27.28179084515336328, -346.2056067578752732 ) ) ;
#27992 = CARTESIAN_POINT ( 'NONE',  ( 795.9930595647434757, -99.07832356259642381, -320.7433823573372820 ) ) ;
#27993 = CARTESIAN_POINT ( 'NONE',  ( 793.4146539503750546, -73.98741447168741558, 307.6481478633938877 ) ) ;
#27994 = CARTESIAN_POINT ( 'NONE',  ( 785.3141322388236176, -405.7255117493283478, 364.4286716492789537 ) ) ;
#27995 = CARTESIAN_POINT ( 'NONE',  ( -521.6730038022808458, 200.0000000000001421, -122.7905160835438068 ) ) ;
#27996 = SURFACE_STYLE_FILL_AREA ( #30788 ) ;
#27997 = CARTESIAN_POINT ( 'NONE',  ( 756.3353852180819104, -437.9073299311463074, 331.1735550268788302 ) ) ;
#27999 = ORIENTED_EDGE ( 'NONE', *, *, #18226, .T. ) ;
#27998 = CARTESIAN_POINT ( 'NONE',  ( 803.8651313633788504, -101.2601417444146250, -332.4468031744301015 ) ) ;
#28000 = CARTESIAN_POINT ( 'NONE',  ( 759.9864689768902508, -50.08914811296584446, -354.9819416627836404 ) ) ;
#28001 = CARTESIAN_POINT ( 'NONE',  ( 757.2208543904082489, -376.7146871989592682, -350.9844846989624330 ) ) ;
#28002 = ADVANCED_FACE ( 'NONE', ( #32428 ), #777, .T. ) ;
#28004 = CARTESIAN_POINT ( 'NONE',  ( 785.3141322388236176, -213.7255117493289731, 364.4286716492789537 ) ) ;
#28003 = CARTESIAN_POINT ( 'NONE',  ( 755.3201227861273992, -243.7255117493287742, 345.3687786644892981 ) ) ;
#28005 = CARTESIAN_POINT ( 'NONE',  ( 746.0683387631852383, -403.4419599262317888, -331.3260364891676204 ) ) ;
#28006 = DIRECTION ( 'NONE',  ( 0.000000000000000000, 0.7372773368101328550, -0.6755902076156506952 ) ) ;
#28007 = ORIENTED_EDGE ( 'NONE', *, *, #21897, .T. ) ;
#28008 = CARTESIAN_POINT ( 'NONE',  ( 788.8264449731200330, -381.1800572038737869, 363.6646147819171233 ) ) ;
#28009 = ORIENTED_EDGE ( 'NONE', *, *, #41026, .F. ) ;
#28010 = CARTESIAN_POINT ( 'NONE',  ( 782.5225473063381969, -262.2709662947831930, -375.2698199232970637 ) ) ;
#28011 = CARTESIAN_POINT ( 'NONE',  ( 751.6929314249750860, -150.9982390220564241, 318.8095938919659034 ) ) ;
#28012 = ORIENTED_EDGE ( 'NONE', *, *, #42223, .F. ) ;
#28013 = CARTESIAN_POINT ( 'NONE',  ( 810.1134526219336749, -200.5328690171415644, 357.8822607201570349 ) ) ;
#28014 = CARTESIAN_POINT ( 'NONE',  ( 778.2165204200184689, -214.8164208402380666, -364.9363028652563230 ) ) ;
#28015 = EDGE_LOOP ( 'NONE', ( #22035, #2762, #11168, #45339, #21362, #17914, #18949, #27328 ) ) ;
#28016 = CARTESIAN_POINT ( 'NONE',  ( 771.2633955100217236, -359.9073299311467053, -363.4237431249939618 ) ) ;
#28017 = CARTESIAN_POINT ( 'NONE',  ( 754.8072714833581358, -4.816420840238714085, -338.1981804954720587 ) ) ;
#28018 = CARTESIAN_POINT ( 'NONE',  ( 776.9566956441375396, -228.8965053807778816, 364.8461984189686405 ) ) ;
#28019 = DIRECTION ( 'NONE',  ( 1.000000000000000000, 0.000000000000000000, 0.000000000000000000 ) ) ;
#28020 = DIRECTION ( 'NONE',  ( 0.000000000000000000, 0.000000000000000000, 1.000000000000000000 ) ) ;
#28021 = EDGE_CURVE ( 'NONE', #39568, #36156, #14877, .T. ) ;
#28022 = EDGE_LOOP ( 'NONE', ( #12619, #2615, #28778, #18344 ) ) ;
#28023 = CARTESIAN_POINT ( 'NONE',  ( 774.6858677611749044, 14.27448825067031812, -315.5713283507209894 ) ) ;
#28024 = FACE_OUTER_BOUND ( 'NONE', #27048, .T. ) ;
#28025 = LINE ( 'NONE', #41216, #43994 ) ;
#28026 = VERTEX_POINT ( 'NONE', #28953 ) ;
#28027 = CARTESIAN_POINT ( 'NONE',  ( 762.1177392798416577, -258.5545181178799226, -309.8865473780659272 ) ) ;
#28028 = CARTESIAN_POINT ( 'NONE',  ( 802.2119215644370342, -126.0090635724257737, 367.5423716828165084 ) ) ;
#28030 = CARTESIAN_POINT ( 'NONE',  ( 791.9812246680005501, -236.6346026584198228, -361.9419747391813189 ) ) ;
#28029 = DIRECTION ( 'NONE',  ( 1.000000000000000000, 1.644774851296528363E-16, 0.000000000000000000 ) ) ;
#28031 = CARTESIAN_POINT ( 'NONE',  ( 754.8983024940795303, -402.8965053807773415, -336.9254006560228163 ) ) ;
#28032 = CARTESIAN_POINT ( 'NONE',  ( 311.1634899080286232, 258.0939999999999941, -193.8809999999963338 ) ) ;
#28033 = DIRECTION ( 'NONE',  ( 0.000000000000000000, 0.000000000000000000, 1.000000000000000000 ) ) ;
#28034 = CARTESIAN_POINT ( 'NONE',  ( 786.5483106153019435, -103.6454272087894850, -364.1601925771022366 ) ) ;
#28035 = EDGE_CURVE ( 'NONE', #29766, #34711, #10712, .T. ) ;
#28036 = CARTESIAN_POINT ( 'NONE',  ( 745.7194118038753459, -373.6454272087887034, 348.7631598425976449 ) ) ;
#28037 = CARTESIAN_POINT ( 'NONE',  ( 939.9999999999992042, 74.99999999999984368, 360.0000000000000000 ) ) ;
#28038 = CARTESIAN_POINT ( 'NONE',  ( 815.1787889125755555, 17.10349461922139369, -343.7953271457877804 ) ) ;
#28039 = CARTESIAN_POINT ( 'NONE',  ( 808.0189434323515343, -302.0891481129650629, -319.0252816721025511 ) ) ;
#28040 = CARTESIAN_POINT ( 'NONE',  ( 805.1927285166397041, 7.183579159761247723, 341.8018195045277707 ) ) ;
#28041 = CARTESIAN_POINT ( 'NONE',  ( 795.1360043628807261, -92.08914811296568814, -360.2193346964456282 ) ) ;
#28042 = CARTESIAN_POINT ( 'NONE',  ( 771.3260364891663130, -235.6454272087890729, 306.0683387631859773 ) ) ;
#28043 = CARTESIAN_POINT ( 'NONE',  ( 798.0661480581538854, -218.5328690171414792, -309.5768839229118043 ) ) ;
#28044 = CARTESIAN_POINT ( 'NONE',  ( 772.4837098697144029, -191.3618753856925991, 374.5518280994205611 ) ) ;
#28045 = CARTESIAN_POINT ( 'NONE',  ( 772.5602148656447525, -441.7255117493282910, -305.7998596910095443 ) ) ;
#28046 = CARTESIAN_POINT ( 'NONE',  ( 784.4999999999993179, -512.9681489794448908, -339.9999999999999432 ) ) ;
#28047 = CARTESIAN_POINT ( 'NONE',  ( 805.1927285166397041, -304.8164208402376403, 341.8018195045277707 ) ) ;
#28048 = CARTESIAN_POINT ( 'NONE',  ( 790.9844846989617508, -94.37269993606224716, 317.2208543904092721 ) ) ;
#28049 = EDGE_CURVE ( 'NONE', #37811, #8747, #25025, .T. ) ;
#28050 = CARTESIAN_POINT ( 'NONE',  ( 805.1927285166397041, -448.8164208402371855, -341.8018195045277707 ) ) ;
#28051 = FACE_OUTER_BOUND ( 'NONE', #13821, .T. ) ;
#28053 = ADVANCED_FACE ( 'NONE', ( #312 ), #40487, .F. ) ;
#28052 = LINE ( 'NONE', #21132, #7793 ) ;
#28055 = CARTESIAN_POINT ( 'NONE',  ( 756.3353852180819104, -317.9073299311468190, 331.1735550268788302 ) ) ;
#28054 = CARTESIAN_POINT ( 'NONE',  ( 754.9735926884551418, -138.3510508353236048, 340.5236548041000333 ) ) ;
#28056 = ORIENTED_EDGE ( 'NONE', *, *, #28958, .T. ) ;
#28057 = CARTESIAN_POINT ( 'NONE',  ( 805.0264073115434940, -270.3510508353231216, -339.4763451958999099 ) ) ;
#28058 = CARTESIAN_POINT ( 'NONE',  ( 795.1360043628807261, -92.08914811296568814, 360.2193346964456282 ) ) ;
#28059 = CARTESIAN_POINT ( 'NONE',  ( 764.3348316497523456, -286.7146871989594388, -308.6759233522265617 ) ) ;
#28060 = DIRECTION ( 'NONE',  ( 0.000000000000000000, 0.000000000000000000, -1.000000000000000000 ) ) ;
#28061 = CARTESIAN_POINT ( 'NONE',  ( 813.2346286133761168, -413.2601417444136018, 328.9521613784389160 ) ) ;
#28062 = ORIENTED_EDGE ( 'NONE', *, *, #30074, .F. ) ;
#28063 = CARTESIAN_POINT ( 'NONE',  ( 792.1044303154645831, -300.4527844766012663, 317.8323909638837677 ) ) ;
#28064 = CARTESIAN_POINT ( 'NONE',  ( 759.9864689768902508, -194.0891481129654039, -354.9819416627836404 ) ) ;
#28065 = CARTESIAN_POINT ( 'NONE',  ( 762.1405469898971887, -409.5436935675101040, 357.8594530101015607 ) ) ;
#28066 = CARTESIAN_POINT ( 'NONE',  ( 800.9747183278959710, -156.9982390220564241, -311.9810565676471583 ) ) ;
#28067 = CARTESIAN_POINT ( 'NONE',  ( 759.9864689768902508, -98.08914811296568814, -354.9819416627836404 ) ) ;
#28068 = ORIENTED_EDGE ( 'NONE', *, *, #45051, .T. ) ;
#28069 = CARTESIAN_POINT ( 'NONE',  ( 783.0745993439762742, -392.1908817542432075, -365.1016975059196739 ) ) ;
#28070 = ADVANCED_FACE ( 'NONE', ( #18787 ), #5352, .T. ) ;
#28072 = CARTESIAN_POINT ( 'NONE',  ( 759.0159684113467620, -424.9181544815158986, 325.8855110935213020 ) ) ;
#28071 = CARTESIAN_POINT ( 'NONE',  ( 764.8639956371174549, -128.0891481129655176, 319.7806653035542013 ) ) ;
#28073 = CARTESIAN_POINT ( 'NONE',  ( 770.0799878456142551, -109.9874144716873019, 362.9823548866085616 ) ) ;
#28076 = CARTESIAN_POINT ( 'NONE',  ( 752.4576283171824116, -405.0783235625954148, 317.7880784355627952 ) ) ;
#28075 = LINE ( 'NONE', #24154, #40258 ) ;
#28074 = CARTESIAN_POINT ( 'NONE',  ( -598.8365100919716042, 256.5000000000001705, -199.9999999999899671 ) ) ;
#28077 = EDGE_CURVE ( 'NONE', #32451, #34298, #29082, .T. ) ;
#28078 = EDGE_LOOP ( 'NONE', ( #39680, #38581 ) ) ;
#28079 = CARTESIAN_POINT ( 'NONE',  ( 793.9708237608222134, -358.9181544815160123, -319.2295555964448681 ) ) ;
#28080 = CARTESIAN_POINT ( 'NONE',  ( 762.1405469898971887, -361.5436935675103882, -357.8594530101015607 ) ) ;
#28081 = CARTESIAN_POINT ( 'NONE',  ( 752.7379699480933368, -156.0090635724256742, -361.9858362298580232 ) ) ;
#28082 = CARTESIAN_POINT ( 'NONE',  ( 760.0363995740630116, -34.91815448151697154, 368.7758568127991907 ) ) ;
#28084 = CARTESIAN_POINT ( 'NONE',  ( 919.9999999999993179, 219.9999999999998863, 360.0000000000000000 ) ) ;
#28083 = CARTESIAN_POINT ( 'NONE',  ( 989.9999999999992042, 62.85347435602256638, -357.4246812887967053 ) ) ;
#28085 = CARTESIAN_POINT ( 'NONE',  ( 754.9735926884551418, -282.3510508353230080, -340.5236548041000333 ) ) ;
#28086 = CARTESIAN_POINT ( 'NONE',  ( 762.3223304703356007, -439.5436935675101040, -322.3223304703362828 ) ) ;
#28087 = CARTESIAN_POINT ( 'NONE',  ( 762.1177392798416577, -138.5545181178802636, -309.8865473780659272 ) ) ;
#28088 = LINE ( 'NONE', #14239, #33744 ) ;
#28090 = EDGE_CURVE ( 'NONE', #39064, #42371, #33540, .T. ) ;
#28089 = CARTESIAN_POINT ( 'NONE',  ( 51.16348990802859475, 230.0000000000000284, -199.9999999999945146 ) ) ;
#28091 = EDGE_CURVE ( 'NONE', #37323, #29612, #31280, .T. ) ;
#28092 = CARTESIAN_POINT ( 'NONE',  ( 799.2566176426618085, -360.0090635724250774, 324.0069404352559559 ) ) ;
#28093 = CARTESIAN_POINT ( 'NONE',  ( 749.5768839229115201, -324.5545181178796952, 358.0661480581553064 ) ) ;
#28094 = CARTESIAN_POINT ( 'NONE',  ( 746.8695393053151292, -197.9073299311472169, -327.6429770376306578 ) ) ;
#28095 = DIRECTION ( 'NONE',  ( 0.000000000000000000, 0.000000000000000000, -1.000000000000000000 ) ) ;
#28096 = DIRECTION ( 'NONE',  ( 0.000000000000000000, 0.000000000000000000, 1.000000000000000000 ) ) ;
#28097 = CARTESIAN_POINT ( 'NONE',  ( 807.2620300519052989, -144.0090635724257027, 318.0141637701419768 ) ) ;
#28098 = CARTESIAN_POINT ( 'NONE',  ( 766.5853460496234675, -109.9874144716873019, -372.3518521366060554 ) ) ;
#28099 = CARTESIAN_POINT ( 'NONE',  ( 782.4968714119720516, -322.8164208402377540, -305.0891759886411023 ) ) ;
#28100 = DIRECTION ( 'NONE',  ( -1.000000000000000000, -0.000000000000000000, -0.000000000000000000 ) ) ;
#28101 = DIRECTION ( 'NONE',  ( -1.000000000000000000, 0.000000000000000000, 0.000000000000000000 ) ) ;
#28102 = CARTESIAN_POINT ( 'NONE',  ( 801.9419747391806368, -186.4527844766017779, 351.9812246680014027 ) ) ;
#28103 = ORIENTED_EDGE ( 'NONE', *, *, #42420, .T. ) ;
#28104 = CARTESIAN_POINT ( 'NONE',  ( 752.7379699480933368, -444.0090635724249069, 361.9858362298580232 ) ) ;
#28105 = CARTESIAN_POINT ( 'NONE',  ( 813.2346286133761168, -365.2601417444137155, -328.9521613784389160 ) ) ;
#28106 = CARTESIAN_POINT ( 'NONE',  ( 748.9653473494363425, -146.6346026584200217, -356.9462024416521331 ) ) ;
#28107 = CARTESIAN_POINT ( 'NONE',  ( 763.0537975583475827, -408.4527844766009252, -371.0346526505627480 ) ) ;
#28109 = EDGE_CURVE ( 'NONE', #33219, #17388, #32744, .T. ) ;
#28108 = CARTESIAN_POINT ( 'NONE',  ( 0.000000000000000000, 0.000000000000000000, 350.0000000000000000 ) ) ;
#28110 = CARTESIAN_POINT ( 'NONE',  ( 813.2346286133761168, -5.260141744414903897, 328.9521613784389160 ) ) ;
#28111 = ORIENTED_EDGE ( 'NONE', *, *, #37641, .F. ) ;
#28112 = CARTESIAN_POINT ( 'NONE',  ( 778.2165204200184689, -262.8164208402379245, 364.9363028652563230 ) ) ;
#28113 = VECTOR ( 'NONE', #15097, 1000.000000000000000 ) ;
#28114 = CARTESIAN_POINT ( 'NONE',  ( 746.7653713866222915, -185.2601417444143692, -351.0478386215610271 ) ) ;
#28115 = DIRECTION ( 'NONE',  ( 0.000000000000000000, -0.6594541114781790059, 0.7517448203044204691 ) ) ;
#28116 = CARTESIAN_POINT ( 'NONE',  ( 759.8311093483677041, -310.1692326535048778, 310.9282345327691814 ) ) ;
#28117 = CARTESIAN_POINT ( 'NONE',  ( 804.6798772138710092, -135.7255117493291721, 334.6312213355106451 ) ) ;
#28118 = ORIENTED_EDGE ( 'NONE', *, *, #25160, .F. ) ;
#28119 = CARTESIAN_POINT ( 'NONE',  ( 762.1405469898971887, -313.5436935675102745, 357.8594530101015607 ) ) ;
#28120 = CARTESIAN_POINT ( 'NONE',  ( 814.5518280994195948, -15.72551174932958951, -332.4837098697145734 ) ) ;
#28121 = DIRECTION ( 'NONE',  ( -0.000000000000000000, 1.000000000000000000, -0.000000000000000000 ) ) ;
#28122 = EDGE_LOOP ( 'NONE', ( #20449, #37027 ) ) ;
#28123 = CARTESIAN_POINT ( 'NONE',  ( 745.5313806188320314, -423.2817908451521589, -333.7943932421247268 ) ) ;
#28124 = ORIENTED_EDGE ( 'NONE', *, *, #43023, .T. ) ;
#28125 = EDGE_CURVE ( 'NONE', #37078, #29447, #5141, .T. ) ;
#28126 = CARTESIAN_POINT ( 'NONE',  ( 795.1360043628807261, -20.08914811296592973, 360.2193346964456282 ) ) ;
#28127 = CARTESIAN_POINT ( 'NONE',  ( 781.7834795799800531, -274.8164208402378108, -315.0636971347436202 ) ) ;
#28129 = CARTESIAN_POINT ( 'NONE',  ( 771.2368401574024119, -253.4419599262323572, 374.2805881961240857 ) ) ;
#28128 = CARTESIAN_POINT ( 'NONE',  ( 749.2812353651451076, -366.4527844766012095, 323.2262854647983090 ) ) ;
#28130 = EDGE_CURVE ( 'NONE', #30797, #44478, #41602, .T. ) ;
#28131 = CARTESIAN_POINT ( 'NONE',  ( 746.0683387631852383, -67.44195992623289726, 331.3260364891676204 ) ) ;
#28132 = CARTESIAN_POINT ( 'NONE',  ( 763.0428371773158460, -251.4636090269709143, -358.7617431975195359 ) ) ;
#28133 = CARTESIAN_POINT ( 'NONE',  ( 771.1735550268778070, -249.1800572038742416, -316.3353852180827630 ) ) ;
#28134 = CARTESIAN_POINT ( 'NONE',  ( 804.4286716492782716, -449.3618753856918602, -345.3141322388244703 ) ) ;
#28135 = CARTESIAN_POINT ( 'NONE',  ( 754.8072714833581358, -124.8164208402383508, -338.1981804954720587 ) ) ;
#28136 = CARTESIAN_POINT ( 'NONE',  ( 800.0135310231082713, -230.0891481129652618, 325.0180583372163028 ) ) ;
#28137 = CARTESIAN_POINT ( 'NONE',  ( 792.2312462859673587, -395.9073299311465348, 307.2067596250082602 ) ) ;
#28139 = DIRECTION ( 'NONE',  ( -0.000000000000000000, -0.000000000000000000, 1.000000000000000000 ) ) ;
#28138 = LINE ( 'NONE', #17067, #33690 ) ;
#28140 = CARTESIAN_POINT ( 'NONE',  ( 802.2119215644370342, -54.00906357242601530, -367.5423716828165084 ) ) ;
#28141 = DIRECTION ( 'NONE',  ( -1.000000000000000000, 0.000000000000000000, 0.000000000000000000 ) ) ;
#28143 = EDGE_CURVE ( 'NONE', #35726, #33524, #43704, .T. ) ;
#28142 = CARTESIAN_POINT ( 'NONE',  ( 989.9999999999992042, -428.4497686941065808, -352.6378164459125060 ) ) ;
#28144 = CARTESIAN_POINT ( 'NONE',  ( 779.4763451958990572, -272.7363362996981095, 365.0264073115438919 ) ) ;
#28145 = CARTESIAN_POINT ( 'NONE',  ( 791.9812246680005501, -116.6346026584201780, 361.9419747391813189 ) ) ;
#28146 = PRODUCT_DEFINITION ( 'UNKNOWN', '', #31201, #34424 ) ;
#28147 = ORIENTED_EDGE ( 'NONE', *, *, #15051, .F. ) ;
#28148 = CARTESIAN_POINT ( 'NONE',  ( 801.5560724626406000, -24.55451811788064020, -326.7756240680316182 ) ) ;
#28149 = AXIS2_PLACEMENT_3D ( 'NONE', #21280, #39776, #28898 ) ;
#28150 = CARTESIAN_POINT ( 'NONE',  ( 787.4397851343537695, -93.72551174932934259, -374.2001403089903988 ) ) ;
#28151 = CARTESIAN_POINT ( 'NONE',  ( 755.8398074228967971, -307.4419599262320730, 333.4516893846970333 ) ) ;
#28152 = DIRECTION ( 'NONE',  ( 0.000000000000000000, 0.000000000000000000, 1.000000000000000000 ) ) ;
#28153 = CARTESIAN_POINT ( 'NONE',  ( 746.4236121716829757, -39.82724539060786384, 328.8385539511384650 ) ) ;
#28154 = CARTESIAN_POINT ( 'NONE',  ( 777.4774526936600978, -250.2709662947832783, -304.7301800767027657 ) ) ;
#28155 = CARTESIAN_POINT ( 'NONE',  ( 746.8695393053150156, -173.9073299311472169, 327.6429770376306010 ) ) ;
#28156 = CARTESIAN_POINT ( 'NONE',  ( 800.0135310231082713, -86.08914811296573077, 325.0180583372163028 ) ) ;
#28157 = DIRECTION ( 'NONE',  ( -0.000000000000000000, -0.000000000000000000, 1.000000000000000000 ) ) ;
#28158 = CARTESIAN_POINT ( 'NONE',  ( 795.6651683502461765, -274.7146871989594388, -371.3240766477733814 ) ) ;
#28159 = CARTESIAN_POINT ( 'NONE',  ( 762.1177392798416577, -450.5545181178793541, 309.8865473780659272 ) ) ;
#28160 = CARTESIAN_POINT ( 'NONE',  ( 787.5162901302840055, -323.3618753856923149, -305.4481719005792684 ) ) ;
#28161 = CARTESIAN_POINT ( 'NONE',  ( 879.9999999999992042, 240.0000000000000853, -360.0000000000000000 ) ) ;
#28162 = CARTESIAN_POINT ( 'NONE',  ( 754.8983024940795303, -354.8965053807774552, 336.9254006560228163 ) ) ;
#28163 = CARTESIAN_POINT ( 'NONE',  ( 759.0252816721024374, -48.99823902205675807, 368.0189434323527280 ) ) ;
#28164 = CARTESIAN_POINT ( 'NONE',  ( 781.7834795799800531, -370.8164208402375834, -315.0636971347436202 ) ) ;
#28165 = CARTESIAN_POINT ( 'NONE',  ( 775.9200461376533440, -47.80559628986931386, 315.3028492785443291 ) ) ;
#28166 = CARTESIAN_POINT ( 'NONE',  ( 744.9990715423526808, -42.35105083532388193, -341.2370466360926002 ) ) ;
#28167 = CARTESIAN_POINT ( 'NONE',  ( 763.2154366446407039, -189.6237781080507148, -321.4292242960311228 ) ) ;
#28168 = CARTESIAN_POINT ( 'NONE',  ( 805.9055244015594326, -195.6237781080506863, 315.8990559732753240 ) ) ;
#28169 = CARTESIAN_POINT ( 'NONE',  ( 805.1927285166399315, -16.81642084023867412, 341.8018195045277707 ) ) ;
#28170 = ORIENTED_EDGE ( 'NONE', *, *, #15926, .F. ) ;
#28171 = CARTESIAN_POINT ( 'NONE',  ( 759.2295555964440155, -184.1692326535052757, -353.9708237608231229 ) ) ;
#28172 = CARTESIAN_POINT ( 'NONE',  ( 801.9419747391806368, -210.4527844766016926, 351.9812246680014027 ) ) ;
#28173 = CARTESIAN_POINT ( 'NONE',  ( 752.4576283171824116, -21.07832356259667250, -317.7880784355627952 ) ) ;
#28174 = CARTESIAN_POINT ( 'NONE',  ( 802.1676090361155502, -326.6346026584194533, 327.8955696845344505 ) ) ;
#28175 = AXIS2_PLACEMENT_3D ( 'NONE', #12802, #16504, #6100 ) ;
#28176 = CARTESIAN_POINT ( 'NONE',  ( 799.9999999999993179, 197.3292319334027241, 273.4704985657796783 ) ) ;
#28177 = ORIENTED_EDGE ( 'NONE', *, *, #2078, .T. ) ;
#28178 = CARTESIAN_POINT ( 'NONE',  ( 758.6633372737375112, -68.53286901714197654, 326.9102291470432533 ) ) ;
#28179 = CARTESIAN_POINT ( 'NONE',  ( 781.2370466360911223, -308.7363362996979390, -304.9990715423533629 ) ) ;
#28180 = CARTESIAN_POINT ( 'NONE',  ( 767.7687537140311633, -239.9073299311470748, 372.7932403749916830 ) ) ;
#28181 = CARTESIAN_POINT ( 'NONE',  ( 768.8385539511368734, 0.7398582555850804487, 306.4236121716840557 ) ) ;
#28182 = CARTESIAN_POINT ( 'NONE',  ( 769.9779781133707957, -139.0999726633348530, -316.7813123517150871 ) ) ;
#28183 = CARTESIAN_POINT ( 'NONE',  ( 803.4237431249931660, -159.1800572038746111, -331.2633955100225194 ) ) ;
#28184 = CARTESIAN_POINT ( 'NONE',  ( 802.1676090361155502, -350.6346026584193396, -327.8955696845344505 ) ) ;
#28185 = ORIENTED_EDGE ( 'NONE', *, *, #8376, .F. ) ;
#28186 = CARTESIAN_POINT ( 'NONE',  ( 812.7932403749906598, -279.1800572038741848, 327.7687537140311633 ) ) ;
#28187 = DIRECTION ( 'NONE',  ( -0.000000000000000000, 1.000000000000000000, -0.000000000000000000 ) ) ;
#28188 = CARTESIAN_POINT ( 'NONE',  ( 801.3366627262608972, -344.5328690171410813, 353.0897708529566899 ) ) ;
#28189 = LINE ( 'NONE', #17811, #13057 ) ;
#28190 = CARTESIAN_POINT ( 'NONE',  ( 804.1105419155481968, -147.8272453906075157, 347.6308680596136469 ) ) ;
#28191 = CARTESIAN_POINT ( 'NONE',  ( 803.6646147819161570, -17.90732993114776406, 348.8264449731210561 ) ) ;
#28192 = VERTEX_POINT ( 'NONE', #8386 ) ;
#28193 = CARTESIAN_POINT ( 'NONE',  ( 813.5763878283155464, -387.8272453906067767, -351.1614460488615350 ) ) ;
#28194 = DIRECTION ( 'NONE',  ( -0.000000000000000000, 1.000000000000000000, -0.000000000000000000 ) ) ;
#28195 = CARTESIAN_POINT ( 'NONE',  ( 783.7953271457878373, -224.1908817542436623, 375.1787889125761239 ) ) ;
#28196 = CARTESIAN_POINT ( 'NONE',  ( 755.0488828828309806, -185.8055962898689302, 344.1219089521771934 ) ) ;
#28197 = CARTESIAN_POINT ( 'NONE',  ( 801.9419747391806368, -378.4527844766011526, -351.9812246680014027 ) ) ;
#28198 = FILL_AREA_STYLE ('',( #14126 ) ) ;
#28199 = CARTESIAN_POINT ( 'NONE',  ( 754.7162404726377645, -230.7363362996981664, -339.4709603349214717 ) ) ;
#28200 = CARTESIAN_POINT ( 'NONE',  ( 777.4774526936600978, -10.27096629478414691, 304.7301800767027657 ) ) ;
#28201 = CARTESIAN_POINT ( 'NONE',  ( 754.9967657858570647, -73.54369356751118403, 365.0032342141425374 ) ) ;
#28202 = CARTESIAN_POINT ( 'NONE',  ( 829.9999999999992042, 430.0000000000002842, -320.0000000000000568 ) ) ;
#28203 = CARTESIAN_POINT ( 'NONE',  ( 744.7301800767020268, -412.8164208402373561, -337.4774526936615189 ) ) ;
#28204 = DIRECTION ( 'NONE',  ( 0.000000000000000000, -6.938893903907241197E-16, 1.000000000000000000 ) ) ;
#28205 = CARTESIAN_POINT ( 'NONE',  ( 764.1737431748507561, -346.3726999360614514, 371.6461892240376415 ) ) ;
#28206 = DIRECTION ( 'NONE',  ( 0.000000000000000000, 1.000000000000000000, 0.000000000000000000 ) ) ;
#28207 = CARTESIAN_POINT ( 'NONE',  ( 787.4397851343537695, -333.7255117493286320, 374.2001403089903988 ) ) ;
#28208 = CARTESIAN_POINT ( 'NONE',  ( 801.1904061080336987, -44.08914811296584446, -368.3070685750235498 ) ) ;
#28209 = CARTESIAN_POINT ( 'NONE',  ( 805.1927285166397041, -280.8164208402378677, -341.8018195045277707 ) ) ;
#28210 = FACE_OUTER_BOUND ( 'NONE', #32215, .T. ) ;
#28211 = CARTESIAN_POINT ( 'NONE',  ( 756.3353852180819104, -413.9073299311465348, 331.1735550268788302 ) ) ;
#28212 = CARTESIAN_POINT ( 'NONE',  ( 783.0745993439762742, -152.1908817542438612, 365.1016975059196739 ) ) ;
#28213 = CARTESIAN_POINT ( 'NONE',  ( 815.3608509340175488, -26.73633629969882008, -341.2497674668889545 ) ) ;
#28214 = CARTESIAN_POINT ( 'NONE',  ( 794.1144889064781864, -82.16923265350558836, -360.9840315886528401 ) ) ;
#28215 = CARTESIAN_POINT ( 'NONE',  ( 748.3538107759620743, -112.7146871989600356, 355.8262568251490165 ) ) ;
#28216 = CARTESIAN_POINT ( 'NONE',  ( 758.0580252608178853, -390.4527844766011526, 328.0187753319985404 ) ) ;
#28217 = CARTESIAN_POINT ( 'NONE',  ( 799.9999999999993179, 205.0000000000000568, -350.0000000000000000 ) ) ;
#28218 = CARTESIAN_POINT ( 'NONE',  ( 774.6858677611749044, 14.27448825067031812, -315.5713283507209894 ) ) ;
#28219 = ORIENTED_EDGE ( 'NONE', *, *, #33989, .T. ) ;
#28220 = CARTESIAN_POINT ( 'NONE',  ( 778.1981804954714335, -82.27096629478388934, -314.8072714833589885 ) ) ;
#28221 = CARTESIAN_POINT ( 'NONE',  ( 776.9566956441375396, -396.8965053807772847, -364.8461984189686405 ) ) ;
#28223 = CARTESIAN_POINT ( 'NONE',  ( 785.3687786644885591, -227.3618753856925423, 315.3201227861280813 ) ) ;
#28222 = CARTESIAN_POINT ( 'NONE',  ( 762.1405469898971887, -241.5436935675106156, 357.8594530101015607 ) ) ;
#28224 = CIRCLE ( 'NONE', #1673, 10.00000000000000888 ) ;
#28225 = CARTESIAN_POINT ( 'NONE',  ( 751.2241431872005251, -400.1692326535045936, -359.9636004259367610 ) ) ;
#28226 = CARTESIAN_POINT ( 'NONE',  ( 805.0032342141412300, 10.45630643248850866, 314.9967657858571783 ) ) ;
#28227 = CARTESIAN_POINT ( 'NONE',  ( 772.4999999999993179, -512.9681489794448908, -350.0000000000000000 ) ) ;
#28228 = VERTEX_POINT ( 'NONE', #29624 ) ;
#28229 = CARTESIAN_POINT ( 'NONE',  ( 800.2193346964447755, -426.9982390220554862, 355.1360043628815788 ) ) ;
#28230 = ORIENTED_EDGE ( 'NONE', *, *, #26142, .T. ) ;
#28231 = CARTESIAN_POINT ( 'NONE',  ( 754.9967657858570647, -241.5436935675106156, -365.0032342141425374 ) ) ;
#28232 = CARTESIAN_POINT ( 'NONE',  ( 772.4837098697145166, -143.3618753856927697, 374.5518280994205611 ) ) ;
#28233 = ORIENTED_EDGE ( 'NONE', *, *, #31749, .F. ) ;
#28234 = CARTESIAN_POINT ( 'NONE',  ( 758.0580252608178853, -246.4527844766016074, -328.0187753319985404 ) ) ;
#28235 = ORIENTED_EDGE ( 'NONE', *, *, #5817, .T. ) ;
#28236 = CARTESIAN_POINT ( 'NONE',  ( 785.3687786644884454, -347.3618753856922012, -315.3201227861279676 ) ) ;
#28237 = CARTESIAN_POINT ( 'NONE',  ( 767.8955696845333705, -24.45278447660229304, -362.1676090361162323 ) ) ;
#28238 = CARTESIAN_POINT ( 'NONE',  ( 760.5453621957607311, -213.0783235625960401, 323.8424801807151425 ) ) ;
#28239 = CARTESIAN_POINT ( 'NONE',  ( 758.7867965644027208, 16.45630643248849267, 318.7867965644036872 ) ) ;
#28240 = CARTESIAN_POINT ( 'NONE',  ( 767.9999999999992042, 205.0000000000000568, -360.0000000000000000 ) ) ;
#28241 = ORIENTED_EDGE ( 'NONE', *, *, #11776, .T. ) ;
#28242 = CARTESIAN_POINT ( 'NONE',  ( 797.8594530101008786, -13.54369356751140785, -322.1405469898980982 ) ) ;
#28243 = FACE_BOUND ( 'NONE', #40912, .T. ) ;
#28244 = EDGE_LOOP ( 'NONE', ( #17353, #18198, #22256, #33242 ) ) ;
#28245 = CARTESIAN_POINT ( 'NONE',  ( 797.8822607201568644, -270.5545181178798657, -370.1134526219340160 ) ) ;
#28247 = CARTESIAN_POINT ( 'NONE',  ( 804.9363028652555840, -256.2709662947834204, -338.2165204200192079 ) ) ;
#28246 = DIRECTION ( 'NONE',  ( 1.000000000000000000, 0.000000000000000000, 0.000000000000000000 ) ) ;
#28248 = CARTESIAN_POINT ( 'NONE',  ( 804.1601925771018387, -391.4419599262317888, -346.5483106153029098 ) ) ;
#28249 = DIRECTION ( 'NONE',  ( 1.000000000000000000, 0.000000000000000000, 0.000000000000000000 ) ) ;
#28250 = CARTESIAN_POINT ( 'NONE',  ( 805.2837595273609850, -122.7363362996985074, -340.5290396650784714 ) ) ;
#28251 = AXIS2_PLACEMENT_3D ( 'NONE', #5041, #2241, #44286 ) ;
#28252 = DIRECTION ( 'NONE',  ( -0.000000000000000000, 1.000000000000000000, -0.000000000000000000 ) ) ;
#28253 = CARTESIAN_POINT ( 'NONE',  ( 759.8311093483677041, 1.830767346494167391, -310.9282345327691814 ) ) ;
#28254 = CARTESIAN_POINT ( 'NONE',  ( 800.9747183278959710, -324.9982390220559409, -311.9810565676471583 ) ) ;
#28255 = CARTESIAN_POINT ( 'NONE',  ( 799.9999999999993179, 205.0000000000000568, -339.9999999999999432 ) ) ;
#28256 = CARTESIAN_POINT ( 'NONE',  ( 755.3201227861273992, -3.725511749329622813, 345.3687786644892981 ) ) ;
#28257 = CARTESIAN_POINT ( 'NONE',  ( 771.1735550268778070, -81.18005720387481006, -316.3353852180827630 ) ) ;
#28258 = DIRECTION ( 'NONE',  ( 0.000000000000000000, 0.000000000000000000, 1.000000000000000000 ) ) ;
#28259 = CARTESIAN_POINT ( 'NONE',  ( 795.8262568251477660, -262.3726999360617924, 308.3538107759623585 ) ) ;
#28260 = CARTESIAN_POINT ( 'NONE',  ( 814.8230680027162407, -197.8055962898688733, -333.7305795820267917 ) ) ;
#28261 = CARTESIAN_POINT ( 'NONE',  ( 812.7932403749906598, -207.1800572038744406, 327.7687537140311633 ) ) ;
#28262 = CARTESIAN_POINT ( 'NONE',  ( 813.1304606946830518, -449.9073299311463643, -352.3570229623690580 ) ) ;
#28263 = LINE ( 'NONE', #42609, #1118 ) ;
#28264 = CARTESIAN_POINT ( 'NONE',  ( 803.4237431249931660, -279.1800572038741848, 331.2633955100225194 ) ) ;
#28265 = CARTESIAN_POINT ( 'NONE',  ( 800.9840315886518738, -100.9181544815167513, 354.1144889064786412 ) ) ;
#28266 = CARTESIAN_POINT ( 'NONE',  ( 763.2154366446407039, 26.37622189194863509, -321.4292242960311228 ) ) ;
#28267 = DIRECTION ( 'NONE',  ( 0.000000000000000000, 0.000000000000000000, 1.000000000000000000 ) ) ;
#28268 = PRESENTATION_LAYER_ASSIGNMENT (  '', '', ( #20883 ) ) ;
#28269 = DIRECTION ( 'NONE',  ( 1.000000000000000000, 0.000000000000000000, 0.000000000000000000 ) ) ;
#28271 = CARTESIAN_POINT ( 'NONE',  ( 771.1735550268778070, -369.1800572038739574, 316.3353852180827630 ) ) ;
#28270 = CARTESIAN_POINT ( 'NONE',  ( 784.0799538623451781, -131.8055962898690439, 364.6971507214555572 ) ) ;
#28272 = ORIENTED_EDGE ( 'NONE', *, *, #45291, .T. ) ;
#28273 = CARTESIAN_POINT ( 'NONE',  ( 769.1273215169530886, -310.7146871989593251, -317.4527132478988847 ) ) ;
#28274 = CARTESIAN_POINT ( 'NONE',  ( 755.3201227861273992, -99.72551174932928575, 345.3687786644892981 ) ) ;
#28275 = CARTESIAN_POINT ( 'NONE',  ( 752.4576283171824116, -285.0783235625958127, -317.7880784355627952 ) ) ;
#28276 = DIRECTION ( 'NONE',  ( 0.000000000000000000, -0.9238795325112892920, 0.3826834323650836756 ) ) ;
#28277 = CARTESIAN_POINT ( 'NONE',  ( 786.2056067578752163, -419.8055962898681059, 374.4686193811670023 ) ) ;
#28278 = EDGE_CURVE ( 'NONE', #3171, #19734, #43933, .T. ) ;
#28279 = VERTEX_POINT ( 'NONE', #5589 ) ;
#28280 = CARTESIAN_POINT ( 'NONE',  ( 792.1044303154645831, -324.4527844766013231, 317.8323909638837677 ) ) ;
#28281 = CARTESIAN_POINT ( 'NONE',  ( 804.1601925771018387, -55.44195992623293989, -346.5483106153029098 ) ) ;
#28282 = CARTESIAN_POINT ( 'NONE',  ( 797.6776695296629214, -163.5436935675109567, -357.6776695296636603 ) ) ;
#28283 = CARTESIAN_POINT ( 'NONE',  ( 778.2165204200184689, -214.8164208402380666, -364.9363028652563230 ) ) ;
#28284 = CARTESIAN_POINT ( 'NONE',  ( 778.2165204200184689, -406.8164208402375266, 364.9363028652563230 ) ) ;
#28285 = EDGE_CURVE ( 'NONE', #14449, #15624, #43483, .T. ) ;
#28286 = CARTESIAN_POINT ( 'NONE',  ( 772.5602148656447525, -153.7255117493291721, -305.7998596910095443 ) ) ;
#28287 = VECTOR ( 'NONE', #29915, 1000.000000000000000 ) ;
#28288 = CARTESIAN_POINT ( 'NONE',  ( 794.9819416627830151, -132.9982390220564810, -319.9864689768909898 ) ) ;
#28289 = VERTEX_POINT ( 'NONE', #26385 ) ;
#28290 = CARTESIAN_POINT ( 'NONE',  ( 773.4516893846965786, -379.6454272087886466, -315.8398074228977066 ) ) ;
#28291 = CARTESIAN_POINT ( 'NONE',  ( 763.8424801807145741, -426.0090635724247932, 320.5453621957614700 ) ) ;
#28292 = CARTESIAN_POINT ( 'NONE',  ( 805.0264073115434940, -126.3510508353236048, 339.4763451958999099 ) ) ;
#28293 = B_SPLINE_CURVE_WITH_KNOTS ( 'NONE', 3,
 ( #29101, #28648, #8306, #4606, #18701, #36249, #233, #25636, #10871, #39270, #21476, #4836, #15252, #18939, #21949, #32792, #14572, #14328, #699, #29340, #1144, #43412, #11090, #18024, #42726, #28406, #7625, #43185, #21702, #32102, #22158, #39515, #15013, #42505, #11780, #39053 ),
 .UNSPECIFIED., .F., .F.,
 ( 4, 2, 2, 2, 2, 2, 2, 2, 2, 2, 2, 2, 2, 2, 2, 2, 2, 4 ),
 ( 0.0008252806733485880007, 0.001104729680136533072, 0.001384178686924478251, 0.001943076700500593040, 0.002501974714076708045, 0.003060872727652823484, 0.004178668754804788950, 0.005296464781956755283, 0.007532056836260687949, 0.009767648890564618880, 0.01423883299917248421, 0.01871001710778034607, 0.02094560916208429782, 0.02318120121638824610, 0.02765238532499614266, 0.02988797737930003542, 0.03212356943360392819, 0.03659475354221209537 ),
 .UNSPECIFIED. ) ;
#28296 = CARTESIAN_POINT ( 'NONE',  ( 795.6651683502461765, -394.7146871989591546, 371.3240766477733814 ) ) ;
#28295 = DIRECTION ( 'NONE',  ( 0.000000000000000000, -1.000000000000000000, 0.000000000000000000 ) ) ;
#28294 = DIRECTION ( 'NONE',  ( 1.000000000000000000, 0.000000000000000000, -0.000000000000000000 ) ) ;
#28297 = VERTEX_POINT ( 'NONE', #12524 ) ;
#28298 = CARTESIAN_POINT ( 'NONE',  ( 779.4763451958990572, -392.7363362996977116, -365.0264073115438919 ) ) ;
#28299 = CARTESIAN_POINT ( 'NONE',  ( 797.6776695296629214, -355.5436935675103882, -357.6776695296636603 ) ) ;
#28300 = CARTESIAN_POINT ( 'NONE',  ( 805.6418435158337843, -173.4636090269710849, -363.8556311672236916 ) ) ;
#28301 = CARTESIAN_POINT ( 'NONE',  ( 748.6759233522253680, -16.37269993606248519, 324.3348316497537098 ) ) ;
#28302 = CIRCLE ( 'NONE', #25377, 10.00000000000000888 ) ;
#28304 = DIRECTION ( 'NONE',  ( -1.880165489482579047E-16, -1.000000000000000000, -0.000000000000000000 ) ) ;
#28303 = DIRECTION ( 'NONE',  ( 0.000000000000000000, 0.000000000000000000, 1.000000000000000000 ) ) ;
#28305 = CARTESIAN_POINT ( 'NONE',  ( 772.3691319403857278, -287.2601417444140566, -315.8894580844506663 ) ) ;
#28306 = CARTESIAN_POINT ( 'NONE',  ( 758.0580252608178853, -438.4527844766009821, -328.0187753319985404 ) ) ;
#28307 = CARTESIAN_POINT ( 'NONE',  ( 757.7880784355613741, -138.0090635724257311, -312.4576283171834916 ) ) ;
#28308 = DIRECTION ( 'NONE',  ( 0.000000000000000000, 0.000000000000000000, 1.000000000000000000 ) ) ;
#28309 = DIRECTION ( 'NONE',  ( 0.000000000000000000, 0.000000000000000000, 1.000000000000000000 ) ) ;
#28310 = CARTESIAN_POINT ( 'NONE',  ( 783.0745993439762742, -368.1908817542433212, 365.1016975059196739 ) ) ;
#28311 = CARTESIAN_POINT ( 'NONE',  ( 783.7953271457878373, -344.1908817542433212, 375.1787889125761239 ) ) ;
#28312 = CARTESIAN_POINT ( 'NONE',  ( 759.0252816721024374, -192.9982390220562820, -368.0189434323527280 ) ) ;
#28313 = DIRECTION ( 'NONE',  ( -0.000000000000000000, -0.7517448203044211352, -0.6594541114781783397 ) ) ;
#28314 = CARTESIAN_POINT ( 'NONE',  ( -728.8365100919714905, 258.0940000000001646, -193.8809999999890863 ) ) ;
#28315 = SHAPE_REPRESENTATION ( 'Lower Fixed Bed Shear Blade', ( #26858 ), #32791 ) ;
#28316 = CARTESIAN_POINT ( 'NONE',  ( 764.1737431748507561, -154.3726999360620198, 371.6461892240376415 ) ) ;
#28317 = CARTESIAN_POINT ( 'NONE',  ( 791.1614460488616487, -83.26014174441466764, -373.5763878283158874 ) ) ;
#28318 = CARTESIAN_POINT ( 'NONE',  ( 755.2512626584698410, -127.5436935675110561, 315.2512626584710915 ) ) ;
#28319 = CARTESIAN_POINT ( 'NONE',  ( 748.9653473494363425, -338.6346026584195101, -356.9462024416521331 ) ) ;
#28320 = LINE ( 'NONE', #42661, #41070 ) ;
#28321 = LINE ( 'NONE', #162, #10953 ) ;
#28322 = CARTESIAN_POINT ( 'NONE',  ( 771.1735550268778070, -201.1800572038744690, 316.3353852180827630 ) ) ;
#28323 = AXIS2_PLACEMENT_3D ( 'NONE', #43042, #14663, #8394 ) ;
#28324 = CARTESIAN_POINT ( 'NONE',  ( 796.9571628226829034, 0.5363909730283709099, 321.2382568024804641 ) ) ;
#28325 = CARTESIAN_POINT ( 'NONE',  ( 805.9055244015594326, -411.6237781080499758, -315.8990559732753240 ) ) ;
#28326 = CARTESIAN_POINT ( 'NONE',  ( 772.4837098697144029, -431.3618753856918033, -374.5518280994205611 ) ) ;
#28327 = LINE ( 'NONE', #23715, #30579 ) ;
#28328 = CARTESIAN_POINT ( 'NONE',  ( 795.6651683502461765, 13.28531280103958423, 371.3240766477733814 ) ) ;
#28329 = VERTEX_POINT ( 'NONE', #8838 ) ;
#28330 = EDGE_CURVE ( 'NONE', #36107, #19341, #3219, .T. ) ;
#28331 = CARTESIAN_POINT ( 'NONE',  ( 815.1787889125755555, -198.8965053807779384, -343.7953271457877804 ) ) ;
#28332 = CARTESIAN_POINT ( 'NONE',  ( 813.9316612368132837, -295.4419599262320730, 348.6739635108323228 ) ) ;
#28333 = CARTESIAN_POINT ( 'NONE',  ( 767.8955696845334842, -120.4527844766019768, 362.1676090361161755 ) ) ;
#28334 = VERTEX_POINT ( 'NONE', #1444 ) ;
#28335 = AXIS2_PLACEMENT_3D ( 'NONE', #45467, #2962, #13826 ) ;
#28336 = EDGE_CURVE ( 'NONE', #22935, #16659, #6913, .T. ) ;
#28337 = CARTESIAN_POINT ( 'NONE',  ( 778.2165204200184689, -310.8164208402377540, 364.9363028652563230 ) ) ;
#28338 = ADVANCED_FACE ( 'NONE', ( #23119, #19680, #25922, #40270 ), #8624, .F. ) ;
#28339 = VECTOR ( 'NONE', #30601, 1000.000000000000000 ) ;
#28340 = CARTESIAN_POINT ( 'NONE',  ( 796.9462024416508257, -60.45278447660215448, -308.9653473494370246 ) ) ;
#28342 = AXIS2_PLACEMENT_3D ( 'NONE', #10793, #3641, #38983 ) ;
#28341 = CARTESIAN_POINT ( 'NONE',  ( 810.7187646348534145, -66.45278447660216159, 356.7737145352016341 ) ) ;
#28343 = EDGE_LOOP ( 'NONE', ( #39183, #19208, #42641, #42631, #27106, #968, #18774, #24441, #29229, #5874, #40794 ) ) ;
#28344 = CARTESIAN_POINT ( 'NONE',  ( 814.4686193811664907, -459.2817908451519884, -346.2056067578752732 ) ) ;
#28345 = ORIENTED_EDGE ( 'NONE', *, *, #33741, .T. ) ;
#28346 = ITEM_DEFINED_TRANSFORMATION ( 'NONE', 'NONE', #245,  #26858 ) ;
#28347 = CARTESIAN_POINT ( 'NONE',  ( 767.8955696845333705, -24.45278447660229304, 362.1676090361162323 ) ) ;
#28348 = CARTESIAN_POINT ( 'NONE',  ( 800.2193346964447755, -306.9982390220558273, -355.1360043628815788 ) ) ;
#28350 = CARTESIAN_POINT ( 'NONE',  ( 803.8556311672234642, -273.6237781080504305, 365.6418435158340117 ) ) ;
#28349 = CARTESIAN_POINT ( 'NONE',  ( 751.9810565676468741, -386.0891481129647786, 360.9747183278973921 ) ) ;
#28351 = CARTESIAN_POINT ( 'NONE',  ( 815.1787889125755555, -78.89650538077832209, 343.7953271457877804 ) ) ;
#28352 = CARTESIAN_POINT ( 'NONE',  ( 766.9102291470427417, -306.5545181178797520, -318.6633372737382501 ) ) ;
#28353 = CARTESIAN_POINT ( 'NONE',  ( 765.0180583372156207, -240.9982390220561683, -360.0135310231089534 ) ) ;
#28354 = CARTESIAN_POINT ( 'NONE',  ( 764.8639956371174549, -440.0891481129645513, -319.7806653035542581 ) ) ;
#28355 = CARTESIAN_POINT ( 'NONE',  ( 755.0636971347428243, -124.2709662947837899, -341.7834795799807353 ) ) ;
#28356=STYLED_ITEM('',(#45751),#1937);
#28357 = EDGE_CURVE ( 'NONE', #43845, #19525, #28293, .T. ) ;
#28358 = DIRECTION ( 'NONE',  ( 0.000000000000000000, 0.000000000000000000, -1.000000000000000000 ) ) ;
#28359 = CARTESIAN_POINT ( 'NONE',  ( 812.7932403749906598, -399.1800572038738437, 327.7687537140311633 ) ) ;
#28360 = VECTOR ( 'NONE', #21342, 1000.000000000000000 ) ;
#28362 = DIRECTION ( 'NONE',  ( 0.7071067811857625340, 0.000000000000000000, -0.7071067811873326114 ) ) ;
#28361 = CARTESIAN_POINT ( 'NONE',  ( -829.9999999999992042, 529.9999999999997726, -320.0000000000000000 ) ) ;
#28363 = EDGE_CURVE ( 'NONE', #15194, #20750, #4708, .T. ) ;
#28364 = CARTESIAN_POINT ( 'NONE',  ( 745.1792804349281596, -38.19088175424422360, -343.7566961878542884 ) ) ;
#28365 = DIRECTION ( 'NONE',  ( 0.000000000000000000, 0.000000000000000000, -1.000000000000000000 ) ) ;
#28366 = LINE ( 'NONE', #42237, #28971 ) ;
#28367 = CARTESIAN_POINT ( 'NONE',  ( 790.9844846989617508, -262.3726999360617924, 317.2208543904092721 ) ) ;
#28368 = CARTESIAN_POINT ( 'NONE',  ( 804.9363028652555840, -112.2709662947838325, 338.2165204200192079 ) ) ;
#28369 = EDGE_LOOP ( 'NONE', ( #23629, #27208, #34034, #16192 ) ) ;
#28370 = CARTESIAN_POINT ( 'NONE',  ( 759.0159684113467620, -16.91815448151702839, -325.8855110935213020 ) ) ;
#28371 = CARTESIAN_POINT ( 'NONE',  ( 755.2512626584698410, -103.5436935675111272, -315.2512626584710915 ) ) ;
#28372 = CARTESIAN_POINT ( 'NONE',  ( 803.8651313633788504, -293.2601417444139429, 332.4468031744301015 ) ) ;
#28373 = DIRECTION ( 'NONE',  ( 0.000000000000000000, -0.000000000000000000, -1.000000000000000000 ) ) ;
#28374 = AXIS2_PLACEMENT_3D ( 'NONE', #43826, #26512, #12886 ) ;
#28375 = CARTESIAN_POINT ( 'NONE',  ( 811.3240766477731540, -52.37269993606237506, 355.6651683502462902 ) ) ;
#28376 = CARTESIAN_POINT ( 'NONE',  ( 801.1904061080336987, -236.0891481129651766, -368.3070685750235498 ) ) ;
#28377 = CIRCLE ( 'NONE', #18804, 30.00000000000002842 ) ;
#28378 = CARTESIAN_POINT ( 'NONE',  ( 745.0891759886404770, -172.2709662947836478, 342.4968714119734159 ) ) ;
#28379 = CARTESIAN_POINT ( 'NONE',  ( 797.8594530101008786, -85.54369356751118403, 322.1405469898980982 ) ) ;
#28380 = CYLINDRICAL_SURFACE ( 'NONE', #21773, 2.749999999999863665 ) ;
#28381 = CARTESIAN_POINT ( 'NONE',  ( 795.6651683502461765, -298.7146871989593251, -371.3240766477733814 ) ) ;
#28382 = EDGE_CURVE ( 'NONE', #25632, #12844, #36035, .T. ) ;
#28383 = CARTESIAN_POINT ( 'NONE',  ( 745.5313806188320314, -447.2817908451521021, 333.7943932421247268 ) ) ;
#28384 = CARTESIAN_POINT ( 'NONE',  ( 814.9108240113580450, -328.2709662947831362, -337.5031285880265273 ) ) ;
#28385 = DIRECTION ( 'NONE',  ( 0.000000000000000000, 0.000000000000000000, -1.000000000000000000 ) ) ;
#28386 = CARTESIAN_POINT ( 'NONE',  ( 801.3366627262608972, -368.5328690171409676, 353.0897708529566899 ) ) ;
#28387 = CARTESIAN_POINT ( 'NONE',  ( 758.8095938919644823, -32.08914811296589420, 311.6929314249762797 ) ) ;
#28388 = CARTESIAN_POINT ( 'NONE',  ( 800.0135310231082713, -398.0891481129647218, -325.0180583372163028 ) ) ;
#28389 = EDGE_CURVE ( 'NONE', #34942, #10012, #25851, .T. ) ;
#28390 = AXIS2_PLACEMENT_3D ( 'NONE', #45100, #27526, #14138 ) ;
#28391 = CARTESIAN_POINT ( 'NONE',  ( 804.9511171171677688, -53.80559628986930676, 335.8780910478229202 ) ) ;
#28392 = CARTESIAN_POINT ( 'NONE',  ( 765.0180583372156207, -192.9982390220562820, -360.0135310231089534 ) ) ;
#28393 = VECTOR ( 'NONE', #15507, 1000.000000000000000 ) ;
#28394 = CARTESIAN_POINT ( 'NONE',  ( 811.6461892240364477, -76.71468719896012090, -324.1737431748509835 ) ) ;
#28395 = CARTESIAN_POINT ( 'NONE',  ( 793.4146539503750546, -193.9874144716870319, 307.6481478633938877 ) ) ;
#28396 = CARTESIAN_POINT ( 'NONE',  ( 755.0636971347428243, -4.270966294784170003, 341.7834795799807353 ) ) ;
#28397 = VECTOR ( 'NONE', #37229, 1000.000000000000000 ) ;
#28398 = CARTESIAN_POINT ( 'NONE',  ( 766.7756240680305382, -374.5328690171410813, 361.5560724626415663 ) ) ;
#28399 = VERTEX_POINT ( 'NONE', #39959 ) ;
#28400 = CARTESIAN_POINT ( 'NONE',  ( 756.7813123517142913, -211.9874144716869750, -329.9779781133712504 ) ) ;
#28401 = EDGE_CURVE ( 'NONE', #42322, #29615, #18489, .T. ) ;
#28402 = CARTESIAN_POINT ( 'NONE',  ( 795.1360043628807261, -188.0891481129653187, 360.2193346964456282 ) ) ;
#28403 = CARTESIAN_POINT ( 'NONE',  ( 781.2497674668890113, -36.35105083532390324, -375.3608509340180603 ) ) ;
#28404 = CARTESIAN_POINT ( 'NONE',  ( 762.3223304703356007, -343.5436935675103314, 322.3223304703362828 ) ) ;
#28405 = AXIS2_PLACEMENT_3D ( 'NONE', #16628, #38736, #34152 ) ;
#28406 = CARTESIAN_POINT ( 'NONE',  ( 801.4587497624105481, -452.9681489794446634, -353.8271441104080282 ) ) ;
#28407 = DIRECTION ( 'NONE',  ( 0.000000000000000000, 0.000000000000000000, 1.000000000000000000 ) ) ;
#28408 = SHAPE_REPRESENTATION ( 'Treadle Extension Return Springs', ( #26858 ), #7704 ) ;
#28409 = ORIENTED_EDGE ( 'NONE', *, *, #21897, .F. ) ;
#28410 = CARTESIAN_POINT ( 'NONE',  ( 799.4546378042377910, -57.07832356259658013, 356.1575198192848006 ) ) ;
#28411 = CARTESIAN_POINT ( 'NONE',  ( 757.7880784355613741, -354.0090635724250774, -312.4576283171834916 ) ) ;
#28412 = CIRCLE ( 'NONE', #22498, 7.999999999999896083 ) ;
#28413 = CARTESIAN_POINT ( 'NONE',  ( 772.5602148656447525, -249.7255117493288594, 305.7998596910095443 ) ) ;
#28414 = CARTESIAN_POINT ( 'NONE',  ( 745.1769319972822814, 6.194403710130517382, 346.2694204179732083 ) ) ;
#28415 = CARTESIAN_POINT ( 'NONE',  ( 804.4086373105744769, -145.6454272087893287, -333.3843516231986541 ) ) ;
#28416 = CARTESIAN_POINT ( 'NONE',  ( 759.7806653035534055, -150.9982390220563957, -324.8639956371180801 ) ) ;
#28417 = CARTESIAN_POINT ( 'NONE',  ( 756.3353852180820240, -341.9073299311466485, -331.1735550268787733 ) ) ;
#28418 = ORIENTED_EDGE ( 'NONE', *, *, #3255, .F. ) ;
#28419 = CARTESIAN_POINT ( 'NONE',  ( 787.5162901302840055, -275.3618753856923149, 305.4481719005792684 ) ) ;
#28420 = CARTESIAN_POINT ( 'NONE',  ( 779.9999999999992042, -452.9681489794448339, -329.9999999999999432 ) ) ;
#28421 = CARTESIAN_POINT ( 'NONE',  ( 793.9708237608222134, -214.9181544815164386, 319.2295555964448681 ) ) ;
#28422 = CARTESIAN_POINT ( 'NONE',  ( 779.4709603349208464, -336.3510508353228943, 314.7162404726379918 ) ) ;
#28423 = DIRECTION ( 'NONE',  ( 0.000000000000000000, 0.000000000000000000, -1.000000000000000000 ) ) ;
#28424 = CARTESIAN_POINT ( 'NONE',  ( 801.5560724626406000, -168.5545181178802352, 326.7756240680316182 ) ) ;
#28425 = CARTESIAN_POINT ( 'NONE',  ( 756.5762568750052424, -3.180057203875080063, 348.7366044899774238 ) ) ;
#28426 = ORIENTED_EDGE ( 'NONE', *, *, #32534, .T. ) ;
#28427 = CARTESIAN_POINT ( 'NONE',  ( 760.0363995740630116, -394.9181544815158418, -368.7758568127991907 ) ) ;
#28428 = AXIS2_PLACEMENT_3D ( 'NONE', #44908, #40982, #40135 ) ;
#28429 = CARTESIAN_POINT ( 'NONE',  ( 782.5225473063383106, 1.729033705215812233, -375.2698199232970637 ) ) ;
#28430 = CARTESIAN_POINT ( 'NONE',  ( 815.3608509340175488, -218.7363362996982232, 341.2497674668889545 ) ) ;
#28431 = CARTESIAN_POINT ( 'NONE',  ( 794.1144889064781864, -370.1692326535045936, 360.9840315886528401 ) ) ;
#28432 = CARTESIAN_POINT ( 'NONE',  ( 757.2208543904082489, -184.7146871989598083, 350.9844846989624330 ) ) ;
#28433 = VECTOR ( 'NONE', #9396, 1000.000000000000114 ) ;
#28434 = CARTESIAN_POINT ( 'NONE',  ( 781.7834795799800531, -346.8164208402376971, -315.0636971347436202 ) ) ;
#28435 = CARTESIAN_POINT ( 'NONE',  ( 802.1676090361156639, 9.365397341579420498, 327.8955696845344505 ) ) ;
#28436 = CYLINDRICAL_SURFACE ( 'NONE', #27419, 24.99999999999991118 ) ;
#28437 = CARTESIAN_POINT ( 'NONE',  ( 796.9571628226829034, -215.4636090269709712, -321.2382568024804641 ) ) ;
#28438 = VECTOR ( 'NONE', #7318, 1000.000000000000000 ) ;
#28439 = CARTESIAN_POINT ( 'NONE',  ( 813.1304606946830518, -17.90732993114776406, 352.3570229623690580 ) ) ;
#28440 = CARTESIAN_POINT ( 'NONE',  ( 787.5162901302840055, -83.36187538569296862, 305.4481719005792684 ) ) ;
#28441 = DIRECTION ( 'NONE',  ( 0.000000000000000000, 0.000000000000000000, -1.000000000000000000 ) ) ;
#28442 = CARTESIAN_POINT ( 'NONE',  ( 754.9967657858570647, -409.5436935675101608, -365.0032342141425943 ) ) ;
#28443 = FACE_OUTER_BOUND ( 'NONE', #9674, .T. ) ;
#28444 = AXIS2_PLACEMENT_3D ( 'NONE', #17617, #43177, #36025 ) ;
#28445 = CARTESIAN_POINT ( 'NONE',  ( 799.9636004259356241, -358.9181544815160123, 311.2241431872006956 ) ) ;
#28446 = DIRECTION ( 'NONE',  ( 0.000000000000000000, -0.000000000000000000, -1.000000000000000000 ) ) ;
#28447 = CARTESIAN_POINT ( 'NONE',  ( 748.9653473494363425, -338.6346026584195101, 356.9462024416521331 ) ) ;
#28448 = CARTESIAN_POINT ( 'NONE',  ( 805.0032342141412300, -61.54369356751124087, -314.9967657858571783 ) ) ;
#28449 = CARTESIAN_POINT ( 'NONE',  ( 800.2193346964447755, -282.9982390220558841, -355.1360043628815788 ) ) ;
#28450 = AXIS2_PLACEMENT_3D ( 'NONE', #8671, #1485, #22735 ) ;
#28451 = CARTESIAN_POINT ( 'NONE',  ( 939.9999999999993179, -600.0000000000001137, -350.0000000000000000 ) ) ;
#28452 = CARTESIAN_POINT ( 'NONE',  ( 756.5762568750052424, -435.1800572038737869, 348.7366044899774238 ) ) ;
#28453 = CARTESIAN_POINT ( 'NONE',  ( 755.3028492785439312, -207.2817908451527842, 335.9200461376539693 ) ) ;
#28454 = CARTESIAN_POINT ( 'NONE',  ( 807.2620300519052989, -72.00906357242594424, -318.0141637701419768 ) ) ;
#28455 = CARTESIAN_POINT ( 'NONE',  ( 756.7813123517142913, -67.98741447168742980, -329.9779781133712504 ) ) ;
#28456 = CARTESIAN_POINT ( 'NONE',  ( 812.6845335610512393, -103.9874144716873161, 353.5525998758768651 ) ) ;
#28457 = CARTESIAN_POINT ( 'NONE',  ( 788.7366044899766848, -419.9073299311465348, 316.5762568750059813 ) ) ;
#28458 = CARTESIAN_POINT ( 'NONE',  ( 800.0135310231082713, 9.910851887033969021, -325.0180583372163028 ) ) ;
#28460 = VERTEX_POINT ( 'NONE', #22369 ) ;
#28459 = CARTESIAN_POINT ( 'NONE',  ( 802.7791456095903868, -100.7146871989600356, -329.0155153010375102 ) ) ;
#28461 = CARTESIAN_POINT ( 'NONE',  ( 804.6798772138708955, -111.7255117493293000, -334.6312213355107019 ) ) ;
#28462 = CARTESIAN_POINT ( 'NONE',  ( 759.2295555964440155, -400.1692326535045936, -353.9708237608231229 ) ) ;
#28464 = CARTESIAN_POINT ( 'NONE',  ( 804.9363028652555840, -232.2709662947834488, 338.2165204200192079 ) ) ;
#28463 = CARTESIAN_POINT ( 'NONE',  ( 778.1981804954714335, -226.2709662947834204, 314.8072714833589885 ) ) ;
#28465 = EDGE_LOOP ( 'NONE', ( #9085, #26197, #29349, #38370 ) ) ;
#28466 = CARTESIAN_POINT ( 'NONE',  ( 801.9858362298568863, -411.0783235625954717, -312.7379699480935642 ) ) ;
#28467 = DIRECTION ( 'NONE',  ( 0.000000000000000000, 0.000000000000000000, -1.000000000000000000 ) ) ;
#28468 = ORIENTED_EDGE ( 'NONE', *, *, #8094, .T. ) ;
#28469 = CARTESIAN_POINT ( 'NONE',  ( 759.7806653035534055, -414.9982390220555430, 324.8639956371180801 ) ) ;
#28470 = CONICAL_SURFACE ( 'NONE', #14473, 8.025000000000003908, 0.7853981633974482790 ) ;
#28471 = VERTEX_POINT ( 'NONE', #32343 ) ;
#28472 = SHAPE_REPRESENTATION_RELATIONSHIP ( 'NONE' , 'NONE' ,  #26911, #32092 ) ;
#28473 = CARTESIAN_POINT ( 'NONE',  ( 801.1904061080336987, -236.0891481129651766, -368.3070685750235498 ) ) ;
#28474 = CARTESIAN_POINT ( 'NONE',  ( 814.2001403089898304, -161.3618753856927697, 347.4397851343538264 ) ) ;
#28475 = CARTESIAN_POINT ( 'NONE',  ( 769.9779781133707957, -283.0999726633344267, 316.7813123517150871 ) ) ;
#28476 = CARTESIAN_POINT ( 'NONE',  ( 757.2208543904082489, -376.7146871989592682, 350.9844846989624330 ) ) ;
#28477 = ORIENTED_EDGE ( 'NONE', *, *, #728, .T. ) ;
#28478 = CARTESIAN_POINT ( 'NONE',  ( 804.9363028652555840, -256.2709662947834204, -338.2165204200192079 ) ) ;
#28479 = ORIENTED_EDGE ( 'NONE', *, *, #4345, .F. ) ;
#28480 = CARTESIAN_POINT ( 'NONE',  ( 759.9864689768902508, -362.0891481129648923, -354.9819416627836404 ) ) ;
#28481 = CARTESIAN_POINT ( 'NONE',  ( 755.3201227861273992, -3.725511749329622813, -345.3687786644892981 ) ) ;
#28482 = VECTOR ( 'NONE', #8756, 1000.000000000000000 ) ;
#28483 = CARTESIAN_POINT ( 'NONE',  ( 798.7617431975189675, -243.6237781080504590, 323.0428371773161871 ) ) ;
#28484 = CARTESIAN_POINT ( 'NONE',  ( 746.4999999999993179, -365.3551492539851893, -18.13243251470705886 ) ) ;
#28485 = DIRECTION ( 'NONE',  ( -0.000000000000000000, 1.000000000000000000, -0.000000000000000000 ) ) ;
#28486 = VECTOR ( 'NONE', #16151, 1000.000000000000000 ) ;
#28487 = PRODUCT ( 'MAS-320', 'MAS-320', '', ( #37203 ) ) ;
#28488 = ORIENTED_EDGE ( 'NONE', *, *, #33660, .F. ) ;
#28489 = CARTESIAN_POINT ( 'NONE',  ( 756.5762568750052424, -27.18005720387500901, -348.7366044899774238 ) ) ;
#28490 = FACE_OUTER_BOUND ( 'NONE', #19253, .T. ) ;
#28491 = DIRECTION ( 'NONE',  ( 1.000000000000000000, 0.000000000000000000, 0.000000000000000000 ) ) ;
#28492 = ORIENTED_EDGE ( 'NONE', *, *, #39309, .T. ) ;
#28493 = CARTESIAN_POINT ( 'NONE',  ( 807.2620300519052989, -264.0090635724253616, -318.0141637701419768 ) ) ;
#28494 = CARTESIAN_POINT ( 'NONE',  ( 791.0478386215596629, -141.8272453906075157, 306.7653713866226326 ) ) ;
#28496 = CARTESIAN_POINT ( 'NONE',  ( 764.8639956371174549, -248.0891481129651481, -319.7806653035542013 ) ) ;
#28495 = DIRECTION ( 'NONE',  ( 1.000000000000000000, -1.880165489482579047E-16, 0.000000000000000000 ) ) ;
#28497 = CARTESIAN_POINT ( 'NONE',  ( 803.8651313633788504, -389.2601417444136018, -332.4468031744301015 ) ) ;
#28498 = DIRECTION ( 'NONE',  ( 1.000000000000000000, -0.000000000000000000, -0.000000000000000000 ) ) ;
#28499 = CARTESIAN_POINT ( 'NONE',  ( 802.9823548866075953, -121.0999726633348956, -330.0799878456151077 ) ) ;
#28500 = CARTESIAN_POINT ( 'NONE',  ( 750.9282345327678740, -376.9181544815159555, 319.8311093483690115 ) ) ;
#28501 = LINE ( 'NONE', #42599, #37964 ) ;
#28502 = CARTESIAN_POINT ( 'NONE',  ( 814.8230680027162407, 18.19440371013048008, -333.7305795820267917 ) ) ;
#28503 = CARTESIAN_POINT ( 'NONE',  ( 763.0537975583476964, -312.4527844766013800, -371.0346526505628617 ) ) ;
#28504 = CARTESIAN_POINT ( 'NONE',  ( 998.9999999999992042, 249.9999999999998863, 359.0000000000000000 ) ) ;
#28505 = CARTESIAN_POINT ( 'NONE',  ( 800.0135310231082713, -14.08914811296595460, 325.0180583372163028 ) ) ;
#28506 = VECTOR ( 'NONE', #40025, 1000.000000000000000 ) ;
#28507 = CARTESIAN_POINT ( 'NONE',  ( 760.0363995740630116, -250.9181544815163534, 368.7758568127991907 ) ) ;
#28508 = CARTESIAN_POINT ( 'NONE',  ( 754.0944755984390895, -207.6237781080506295, -364.1009440267246760 ) ) ;
#28509 = CARTESIAN_POINT ( 'NONE',  ( 777.5031285880264704, -214.8164208402380666, 374.9108240113588408 ) ) ;
#28510 = CARTESIAN_POINT ( 'NONE',  ( 808.3070685750230950, -426.9982390220554862, -361.1904061080339261 ) ) ;
#28511 = AXIS2_PLACEMENT_3D ( 'NONE', #38907, #15490, #4253 ) ;
#28512 = DIRECTION ( 'NONE',  ( 0.000000000000000000, -0.3835384033298676054, 0.9235249282889855804 ) ) ;
#28513 = CARTESIAN_POINT ( 'NONE',  ( 794.9819416627830151, -324.9982390220559409, 319.9864689768909898 ) ) ;
#28514 = CIRCLE ( 'NONE', #32978, 30.00000000000008171 ) ;
#28515 = CARTESIAN_POINT ( 'NONE',  ( 796.9571628226829034, -95.46360902697132644, 321.2382568024804641 ) ) ;
#28516 = CARTESIAN_POINT ( 'NONE',  ( 800.9840315886518738, -76.91815448151683654, 354.1144889064786412 ) ) ;
#28517 = CARTESIAN_POINT ( 'NONE',  ( 755.8398074228967971, 4.558040073766884248, -333.4516893846970333 ) ) ;
#28518 = CARTESIAN_POINT ( 'NONE',  ( 701.1634899080286232, 259.9999999999999432, -191.9749999999990848 ) ) ;
#28519 = DIRECTION ( 'NONE',  ( -0.000000000000000000, -0.000000000000000000, 1.000000000000000000 ) ) ;
#28521 = CARTESIAN_POINT ( 'NONE',  ( 803.4237431249931660, -351.1800572038740142, 331.2633955100225194 ) ) ;
#28520 = CARTESIAN_POINT ( 'NONE',  ( 805.1016975059191054, -150.8965053807781089, 343.0745993439771837 ) ) ;
#28522 = ORIENTED_EDGE ( 'NONE', *, *, #23732, .F. ) ;
#28523 = AXIS2_PLACEMENT_3D ( 'NONE', #10309, #35246, #38042 ) ;
#28524 = CARTESIAN_POINT ( 'NONE',  ( 775.9200461376533440, -311.8055962898685038, -315.3028492785443291 ) ) ;
#28525 = CARTESIAN_POINT ( 'NONE',  ( 757.8323909638827445, -146.6346026584200217, 352.1044303154654358 ) ) ;
#28526 = CARTESIAN_POINT ( 'NONE',  ( 746.0683387631852383, -307.4419599262320730, -331.3260364891676204 ) ) ;
#28527 = DIRECTION ( 'NONE',  ( 0.000000000000000000, 0.000000000000000000, -1.000000000000000000 ) ) ;
#28528 = CARTESIAN_POINT ( 'NONE',  ( 759.8311093483677041, -430.1692326535043094, 310.9282345327691814 ) ) ;
#28529 = ORIENTED_EDGE ( 'NONE', *, *, #21559, .F. ) ;
#28530 = CARTESIAN_POINT ( 'NONE',  ( 781.8018195045266339, -310.2709662947832499, 365.1927285166406705 ) ) ;
#28531 = CARTESIAN_POINT ( 'NONE',  ( 798.7617431975189675, -75.62377810805104161, -323.0428371773161871 ) ) ;
#28532 = CARTESIAN_POINT ( 'NONE',  ( 785.3687786644884454, -155.3618753856927128, -315.3201227861279676 ) ) ;
#28533 = CARTESIAN_POINT ( 'NONE',  ( 802.1676090361156639, -206.6346026584198512, -327.8955696845344505 ) ) ;
#28534 = CARTESIAN_POINT ( 'NONE',  ( 791.9812246680005501, -404.6346026584193396, 361.9419747391813189 ) ) ;
#28535 = CARTESIAN_POINT ( 'NONE',  ( 759.0252816721024374, -144.9982390220564525, -368.0189434323527280 ) ) ;
#28536 = EDGE_LOOP ( 'NONE', ( #24521, #32241 ) ) ;
#28537 = CARTESIAN_POINT ( 'NONE',  ( 756.5762568750052424, -147.1800572038746395, -348.7366044899774238 ) ) ;
#28538 = ORIENTED_EDGE ( 'NONE', *, *, #5460, .T. ) ;
#28539 = VECTOR ( 'NONE', #16208, 1000.000000000000000 ) ;
#28540 = CARTESIAN_POINT ( 'NONE',  ( 759.0159684113467620, -400.9181544815159555, -325.8855110935213020 ) ) ;
#28541 = CARTESIAN_POINT ( 'NONE',  ( 766.9102291470427417, -450.5545181178793541, 318.6633372737382501 ) ) ;
#28542 = CARTESIAN_POINT ( 'NONE',  ( 755.0488828828309806, -137.8055962898690154, 344.1219089521771934 ) ) ;
#28543 = CIRCLE ( 'NONE', #16010, 10.00000000000000888 ) ;
#28546 = CARTESIAN_POINT ( 'NONE',  ( 778.7502325331095108, -384.3510508353227806, 304.6391490659818828 ) ) ;
#28545 = DIRECTION ( 'NONE',  ( -0.000000000000000000, 1.000000000000000000, -0.000000000000000000 ) ) ;
#28544 = CARTESIAN_POINT ( 'NONE',  ( 767.9999999999992042, 178.9475563372491251, 320.0000000000000000 ) ) ;
#28547 = ORIENTED_EDGE ( 'NONE', *, *, #26868, .F. ) ;
#28548 = CARTESIAN_POINT ( 'NONE',  ( 755.8894580844503253, -399.8272453906067767, -332.3691319403863531 ) ) ;
#28549 = CYLINDRICAL_SURFACE ( 'NONE', #8574, 9.999999999999980460 ) ;
#28550 = VECTOR ( 'NONE', #15647, 1000.000000000000000 ) ;
#28551 = CARTESIAN_POINT ( 'NONE',  ( 762.1177392798416577, -162.5545181178802352, -309.8865473780659272 ) ) ;
#28552 = CARTESIAN_POINT ( 'NONE',  ( 781.2370466360911223, -20.73633629969883430, 304.9990715423533629 ) ) ;
#28553 = AXIS2_PLACEMENT_3D ( 'NONE', #27069, #45080, #13658 ) ;
#28555 = DIRECTION ( 'NONE',  ( 0.000000000000000000, 0.000000000000000000, 1.000000000000000000 ) ) ;
#28554 = DIRECTION ( 'NONE',  ( 0.000000000000000000, 0.000000000000000000, 1.000000000000000000 ) ) ;
#28556 = CARTESIAN_POINT ( 'NONE',  ( 757.2208543904082489, -304.7146871989594388, -350.9844846989624330 ) ) ;
#28557 = CARTESIAN_POINT ( 'NONE',  ( -200.7583438952259485, 394.6698570112193920, -224.9999999999999716 ) ) ;
#28558 = CARTESIAN_POINT ( 'NONE',  ( 805.6418435158337843, -173.4636090269710849, -363.8556311672236916 ) ) ;
#28559 = DIRECTION ( 'NONE',  ( 0.000000000000000000, 0.000000000000000000, 1.000000000000000000 ) ) ;
#28560 = FACE_BOUND ( 'NONE', #35800, .T. ) ;
#28561 = CIRCLE ( 'NONE', #3500, 2.749999999999919176 ) ;
#28562 = CARTESIAN_POINT ( 'NONE',  ( 798.5707757039680246, -365.4636090269705164, 356.7845633553585003 ) ) ;
#28563 = CARTESIAN_POINT ( 'NONE',  ( 810.4231160770870019, -336.5545181178796952, 321.9338519418446936 ) ) ;
#28564 = CARTESIAN_POINT ( 'NONE',  ( 748.9653473494365699, -194.6346026584199080, -356.9462024416520762 ) ) ;
#28565 = EDGE_CURVE ( 'NONE', #911, #38644, #14795, .T. ) ;
#28566 = CARTESIAN_POINT ( 'NONE',  ( 999.9999999999992042, -590.0000000000001137, -350.0000000000000000 ) ) ;
#28567 = CARTESIAN_POINT ( 'NONE',  ( 785.3687786644884454, 12.63812461430668321, -315.3201227861279676 ) ) ;
#28568 = CARTESIAN_POINT ( 'NONE',  ( 747.6481478633932056, -157.0999726633347962, 353.4146539503763620 ) ) ;
#28569 = CARTESIAN_POINT ( 'NONE',  ( 800.1688906516307043, -82.16923265350558836, -369.0717654672308186 ) ) ;
#28570 = CARTESIAN_POINT ( 'NONE',  ( 772.5602148656447525, -105.7255117493293000, 305.7998596910095443 ) ) ;
#28571 = CARTESIAN_POINT ( 'NONE',  ( 796.7737145352015204, -356.6346026584193964, -370.7187646348536987 ) ) ;
#28572 = EDGE_CURVE ( 'NONE', #42341, #2204, #3290, .T. ) ;
#28573 = FACE_OUTER_BOUND ( 'NONE', #21417, .T. ) ;
#28574 = DIRECTION ( 'NONE',  ( 0.000000000000000000, -0.9235249282889858025, 0.3835384033298669948 ) ) ;
#28575 = CARTESIAN_POINT ( 'NONE',  ( 805.1927285166397041, -208.8164208402380666, 341.8018195045277707 ) ) ;
#28576 = CARTESIAN_POINT ( 'NONE',  ( 804.1105419155481968, -3.827245390607979303, 347.6308680596136469 ) ) ;
#28577 = CARTESIAN_POINT ( 'NONE',  ( 744.8212110874229666, -402.8965053807773415, -336.2046728542121627 ) ) ;
#28578 = VECTOR ( 'NONE', #18915, 1000.000000000000000 ) ;
#28579 = CARTESIAN_POINT ( 'NONE',  ( 751.6929314249748586, -414.9982390220555430, -318.8095938919659034 ) ) ;
#28580 = CARTESIAN_POINT ( 'NONE',  ( 939.9999999999993179, -426.1357934546398383, 350.0000000000000000 ) ) ;
#28581 = CARTESIAN_POINT ( 'NONE',  ( 771.2368401574024119, -13.44195992623305713, 374.2805881961240857 ) ) ;
#28582 = VERTEX_POINT ( 'NONE', #7871 ) ;
#28583 = VECTOR ( 'NONE', #2932, 1000.000000000000000 ) ;
#28584 = CARTESIAN_POINT ( 'NONE',  ( 793.4146539503750546, -193.9874144716870319, -307.6481478633938877 ) ) ;
#28585 = CARTESIAN_POINT ( 'NONE',  ( -115.7583438952258774, -600.0000000000000000, -244.9999999999999716 ) ) ;
#28586 = CARTESIAN_POINT ( 'NONE',  ( 745.1769319972822814, -305.8055962898684470, 346.2694204179732083 ) ) ;
#28587 = CARTESIAN_POINT ( 'NONE',  ( 781.8018195045267476, -118.2709662947838041, 365.1927285166407273 ) ) ;
#28588 = ORIENTED_EDGE ( 'NONE', *, *, #40244, .T. ) ;
#28589 = AXIS2_PLACEMENT_3D ( 'NONE', #1256, #7293, #17905 ) ;
#28590 = CARTESIAN_POINT ( 'NONE',  ( 754.8072714833581358, -316.8164208402377540, 338.1981804954720587 ) ) ;
#28591 = CARTESIAN_POINT ( 'NONE',  ( 772.5602148656447525, -33.72551174932952733, -305.7998596910095443 ) ) ;
#28592 = EDGE_CURVE ( 'NONE', #19341, #25954, #11555, .T. ) ;
#28593 = CARTESIAN_POINT ( 'NONE',  ( 745.0891759886404770, -76.27096629478394618, 342.4968714119734159 ) ) ;
#28594 = ORIENTED_EDGE ( 'NONE', *, *, #8298, .T. ) ;
#28595 = CARTESIAN_POINT ( 'NONE',  ( 760.0363995740630116, -442.9181544815157849, -368.7758568127991907 ) ) ;
#28596 = ORIENTED_EDGE ( 'NONE', *, *, #4927, .T. ) ;
#28597 = PRODUCT_CONTEXT ( 'NONE', #16041, 'mechanical' ) ;
#28598 = CARTESIAN_POINT ( 'NONE',  ( 785.3687786644884454, -35.36187538569316047, 315.3201227861279676 ) ) ;
#28599 = CARTESIAN_POINT ( 'NONE',  ( 764.8639956371174549, -296.0891481129650629, -319.7806653035542013 ) ) ;
#28601 = CARTESIAN_POINT ( 'NONE',  ( 749.8865473780648472, -284.5328690171412518, 322.1177392798429082 ) ) ;
#28600 = CARTESIAN_POINT ( 'NONE',  ( 815.2698199232962679, -400.8164208402374697, 342.5225473063383674 ) ) ;
#28602 = CARTESIAN_POINT ( 'NONE',  ( 748.3538107759620743, -88.71468719896009247, 355.8262568251490165 ) ) ;
#28603 = CARTESIAN_POINT ( 'NONE',  ( 800.9840315886518738, -292.9181544815162397, -354.1144889064786412 ) ) ;
#28604 = CARTESIAN_POINT ( 'NONE',  ( 771.1735550268778070, -273.1800572038742985, -316.3353852180827630 ) ) ;
#28605 = CARTESIAN_POINT ( 'NONE',  ( 797.6776695296629214, -451.5436935675099903, -357.6776695296636603 ) ) ;
#28606 = CARTESIAN_POINT ( 'NONE',  ( 788.7366044899766848, -107.9073299311474727, -316.5762568750059813 ) ) ;
#28607 = DIRECTION ( 'NONE',  ( -1.880165489482579047E-16, -1.000000000000000000, -0.000000000000000000 ) ) ;
#28608 = ORIENTED_EDGE ( 'NONE', *, *, #2975, .T. ) ;
#28609 = CARTESIAN_POINT ( 'NONE',  ( 796.7737145352015204, -380.6346026584192828, 370.7187646348536987 ) ) ;
#28611 = DIRECTION ( 'NONE',  ( -1.058954862565134068E-16, 0.6438296778008191223, 0.7651688349527137056 ) ) ;
#28610 = CARTESIAN_POINT ( 'NONE',  ( 187.1337867209877857, -416.7569064942979935, 212.5753187112033231 ) ) ;
#28612 = CARTESIAN_POINT ( 'NONE',  ( 776.2046728542105711, -92.19088175424406018, -304.8212110874238761 ) ) ;
#28613 = CARTESIAN_POINT ( 'NONE',  ( 786.4999999999993179, -30.07539427629363260, 756.1153575698150462 ) ) ;
#28614 = DIRECTION ( 'NONE',  ( 0.000000000000000000, 0.000000000000000000, -1.000000000000000000 ) ) ;
#28615 = EDGE_CURVE ( 'NONE', #30209, #25624, #23283, .T. ) ;
#28616 = CARTESIAN_POINT ( 'NONE',  ( 763.0428371773158460, -251.4636090269709143, 358.7617431975195359 ) ) ;
#28617 = CARTESIAN_POINT ( 'NONE',  ( 794.9819416627830151, -156.9982390220564241, 319.9864689768909898 ) ) ;
#28618 = VERTEX_POINT ( 'NONE', #44080 ) ;
#28619 = CARTESIAN_POINT ( 'NONE',  ( 769.9779781133707957, -43.09997266333511590, -316.7813123517150871 ) ) ;
#28620 = CARTESIAN_POINT ( 'NONE',  ( 812.7932403749906598, -111.1800572038747532, -327.7687537140311633 ) ) ;
#28621 = CARTESIAN_POINT ( 'NONE',  ( 772.3691319403857278, -311.2601417444139429, 315.8894580844506663 ) ) ;
#28622 = VECTOR ( 'NONE', #7458, 1000.000000000000000 ) ;
#28623 = CARTESIAN_POINT ( 'NONE',  ( -858.8365100919713768, 260.0000000000002274, -199.9999999999881481 ) ) ;
#28624 = CARTESIAN_POINT ( 'NONE',  ( 812.3518521366052028, -49.09997266333511590, 326.5853460496235243 ) ) ;
#28625 = CARTESIAN_POINT ( 'NONE',  ( 759.9864689768902508, -194.0891481129654039, 354.9819416627836404 ) ) ;
#28626 = CARTESIAN_POINT ( 'NONE',  ( 777.4774526936600978, -226.2709662947834204, -304.7301800767027657 ) ) ;
#28627 = EDGE_CURVE ( 'NONE', #42219, #5125, #26129, .T. ) ;
#28628 = EDGE_CURVE ( 'NONE', #7001, #40012, #16360, .T. ) ;
#28629 = CARTESIAN_POINT ( 'NONE',  ( 788.7366044899766848, -83.90732993114754379, 316.5762568750059813 ) ) ;
#28630 = DIRECTION ( 'NONE',  ( 0.000000000000000000, 1.000000000000000000, 1.110223024625155554E-15 ) ) ;
#28631 = CARTESIAN_POINT ( 'NONE',  ( 813.2346286133761168, -293.2601417444139429, -328.9521613784389160 ) ) ;
#28632 = CARTESIAN_POINT ( 'NONE',  ( 814.4686193811664907, -459.2817908451519884, 346.2056067578752732 ) ) ;
#28633 = CARTESIAN_POINT ( 'NONE',  ( 745.7998596910086917, -317.3618753856922581, -332.5602148656461168 ) ) ;
#28634 = CARTESIAN_POINT ( 'NONE',  ( 757.2208543904082489, -376.7146871989592682, 350.9844846989624330 ) ) ;
#28635 = CARTESIAN_POINT ( 'NONE',  ( 800.9747183278959710, -60.99823902205671544, 311.9810565676471583 ) ) ;
#28636 = CARTESIAN_POINT ( 'NONE',  ( 792.1044303154645831, -372.4527844766010958, -317.8323909638837677 ) ) ;
#28637 = CARTESIAN_POINT ( 'NONE',  ( 802.7791456095903868, -52.71468719896020616, 329.0155153010375102 ) ) ;
#28638 = CARTESIAN_POINT ( 'NONE',  ( 793.4146539503750546, -97.98741447168734453, -307.6481478633938877 ) ) ;
#28639 = EDGE_CURVE ( 'NONE', #9195, #22885, #44541, .T. ) ;
#28640 = CARTESIAN_POINT ( 'NONE',  ( 803.8556311672234642, -201.6237781080506863, 365.6418435158340117 ) ) ;
#28641 = CARTESIAN_POINT ( 'NONE',  ( 800.0135310231082713, -14.08914811296595460, 325.0180583372163028 ) ) ;
#28642 = EDGE_CURVE ( 'NONE', #17401, #37455, #40414, .T. ) ;
#28643 = EDGE_LOOP ( 'NONE', ( #45586, #26746, #34229, #19248 ) ) ;
#28644 = CARTESIAN_POINT ( 'NONE',  ( 765.8855110935204493, -190.1692326535052189, -319.0159684113471599 ) ) ;
#28645 = CARTESIAN_POINT ( 'NONE',  ( 785.3141322388236176, -213.7255117493289731, 364.4286716492789537 ) ) ;
#28646 = CARTESIAN_POINT ( 'NONE',  ( 751.2241431872005251, -16.16923265350578021, -359.9636004259367610 ) ) ;
#28647 = CARTESIAN_POINT ( 'NONE',  ( 754.8072714833583632, -316.8164208402377540, 338.1981804954721156 ) ) ;
#28648 = CARTESIAN_POINT ( 'NONE',  ( 809.5171784329539832, -452.9681489794445497, -335.1922280983832252 ) ) ;
#28649 = CARTESIAN_POINT ( 'NONE',  ( -28.63011601220122415, 22.32581219114657856, 895.6886905569881492 ) ) ;
#28650 = ORIENTED_EDGE ( 'NONE', *, *, #38277, .F. ) ;
#28651 = CARTESIAN_POINT ( 'NONE',  ( 773.3843516231979720, -37.44195992623299674, 364.4086373105754433 ) ) ;
#28652 = CARTESIAN_POINT ( 'NONE',  ( 786.2694204179717872, -357.2817908451523294, -305.1769319972829067 ) ) ;
#28653 = VECTOR ( 'NONE', #34349, 1000.000000000000000 ) ;
#28654 = CARTESIAN_POINT ( 'NONE',  ( 814.9108240113580450, -304.2709662947832499, 337.5031285880265273 ) ) ;
#28655 = CARTESIAN_POINT ( 'NONE',  ( 758.0141637701419768, 8.921676437403235127, 367.2620300519063790 ) ) ;
#28656 = CARTESIAN_POINT ( 'NONE',  ( 799.2566176426618085, -192.0090635724255606, -324.0069404352559559 ) ) ;
#28657 = CARTESIAN_POINT ( 'NONE',  ( 800.2193346964447755, -162.9982390220563673, -355.1360043628815788 ) ) ;
#28658 = CARTESIAN_POINT ( 'NONE',  ( 755.0636971347428243, -364.2709662947830793, -341.7834795799807353 ) ) ;
#28659 = ORIENTED_EDGE ( 'NONE', *, *, #27158, .T. ) ;
#28660 = CARTESIAN_POINT ( 'NONE',  ( 745.0891759886404770, -292.2709662947831930, 342.4968714119734159 ) ) ;
#28661 = ADVANCED_FACE ( 'NONE', ( #15476 ), #5279, .T. ) ;
#28662 = CARTESIAN_POINT ( 'NONE',  ( 998.9999999999992042, 478.9999999999999432, 0.000000000000000000 ) ) ;
#28663 = CARTESIAN_POINT ( 'NONE',  ( 790.8726784830453198, -346.7146871989592682, 362.5472867521010585 ) ) ;
#28664 = CARTESIAN_POINT ( 'NONE',  ( 998.9999999999992042, 249.9999999999998863, 200.9999999999999432 ) ) ;
#28665 = EDGE_CURVE ( 'NONE', #21254, #17123, #37143, .T. ) ;
#28666 = CARTESIAN_POINT ( 'NONE',  ( 802.5472867521000353, -172.3726999360619914, 350.8726784830461156 ) ) ;
#28667 = CARTESIAN_POINT ( 'NONE',  ( 802.1676090361156639, -38.63460265842041252, 327.8955696845344505 ) ) ;
#28668 = ORIENTED_EDGE ( 'NONE', *, *, #23757, .T. ) ;
#28669 = CARTESIAN_POINT ( 'NONE',  ( 797.8822607201568644, -414.5545181178795247, -370.1134526219340160 ) ) ;
#28670 = CARTESIAN_POINT ( 'NONE',  ( 804.7487373415286811, 4.456306432488530866, -364.7487373415288516 ) ) ;
#28671 = CARTESIAN_POINT ( 'NONE',  ( 776.2046728542105711, -260.1908817542435486, 304.8212110874238761 ) ) ;
#28672 = CARTESIAN_POINT ( 'NONE',  ( 756.7813123517142913, -187.9874144716870603, 329.9779781133712504 ) ) ;
#28673 = CARTESIAN_POINT ( 'NONE',  ( 803.6646147819161570, -353.9073299311467053, -348.8264449731210561 ) ) ;
#28674 = CARTESIAN_POINT ( 'NONE',  ( 791.9812246680005501, 3.365397341579444479, 361.9419747391813189 ) ) ;
#28675 = CARTESIAN_POINT ( 'NONE',  ( 776.9254006560222479, -212.1908817542436623, -314.8983024940802125 ) ) ;
#28676 = ADVANCED_FACE ( 'NONE', ( #22831 ), #19828, .T. ) ;
#28677 = EDGE_CURVE ( 'NONE', #8754, #23583, #5481, .T. ) ;
#28678 = CARTESIAN_POINT ( 'NONE',  ( 745.4481719005789273, -27.72551174932954510, 347.5162901302853129 ) ) ;
#28679 = CARTESIAN_POINT ( 'NONE',  ( 801.1904061080336987, -92.08914811296568814, 368.3070685750235498 ) ) ;
#28680 = FACE_OUTER_BOUND ( 'NONE', #31430, .T. ) ;
#28681 = CARTESIAN_POINT ( 'NONE',  ( 804.7487373415286811, -403.5436935675101608, -364.7487373415288516 ) ) ;
#28682 = PRESENTATION_STYLE_ASSIGNMENT (( #42986 ) ) ;
#28683 = AXIS2_PLACEMENT_3D ( 'NONE', #38168, #45319, #34690 ) ;
#28684 = CARTESIAN_POINT ( 'NONE',  ( 744.6391490659812007, -350.7363362996978253, 338.7502325331110455 ) ) ;
#28685 = CYLINDRICAL_SURFACE ( 'NONE', #37503, 2.749999999999863665 ) ;
#28686 = CARTESIAN_POINT ( 'NONE',  ( 814.5518280994195948, -327.7255117493285184, 332.4837098697145734 ) ) ;
#28687 = CARTESIAN_POINT ( 'NONE',  ( 811.0346526505616112, -38.63460265842041252, -323.0537975583477532 ) ) ;
#28688 = CARTESIAN_POINT ( 'NONE',  ( 755.0636971347428243, -292.2709662947831930, -341.7834795799807353 ) ) ;
#28689 = CARTESIAN_POINT ( 'NONE',  ( 701.1634899080286232, 259.9999999999999432, -197.2499999999991758 ) ) ;
#28690 = CARTESIAN_POINT ( 'NONE',  ( 768.0187753319979720, -440.6346026584191122, 318.0580252608186242 ) ) ;
#28691 = CARTESIAN_POINT ( 'NONE',  ( 776.9254006560222479, -188.1908817542437760, 314.8983024940802125 ) ) ;
#28692 = CARTESIAN_POINT ( 'NONE',  ( 776.2046728542105711, -68.19088175424413123, -304.8212110874238761 ) ) ;
#28693 = CARTESIAN_POINT ( 'NONE',  ( 755.0488828828309806, -89.80559628986918597, -344.1219089521771934 ) ) ;
#28694 = CARTESIAN_POINT ( 'NONE',  ( 793.4146539503750546, -97.98741447168734453, 307.6481478633938877 ) ) ;
#28695 = CARTESIAN_POINT ( 'NONE',  ( 774.6858677611749044, -417.7255117493283478, 315.5713283507209894 ) ) ;
#28696 = ADVANCED_FACE ( 'NONE', ( #37606, #2040 ), #43842, .F. ) ;
#28697 = CARTESIAN_POINT ( 'NONE',  ( 791.9812246680005501, 3.365397341579444479, -361.9419747391813189 ) ) ;
#28698 = ORIENTED_EDGE ( 'NONE', *, *, #38814, .T. ) ;
#28699 = CARTESIAN_POINT ( 'NONE',  ( 804.9363028652555840, -88.27096629478390355, -338.2165204200192079 ) ) ;
#28700 = CARTESIAN_POINT ( 'NONE',  ( 754.8983024940795303, -402.8965053807773415, -336.9254006560228163 ) ) ;
#28702 = CARTESIAN_POINT ( 'NONE',  ( 781.7834795799800531, -226.8164208402380098, 315.0636971347436202 ) ) ;
#28701 = CARTESIAN_POINT ( 'NONE',  ( 785.3141322388236176, -213.7255117493289731, 364.4286716492789537 ) ) ;
#28703 = CARTESIAN_POINT ( 'NONE',  ( 758.0141637701419768, -399.0783235625955285, -367.2620300519063790 ) ) ;
#28704 = PLANE ( 'NONE',  #5012 ) ;
#28705 = ORIENTED_EDGE ( 'NONE', *, *, #16570, .T. ) ;
#28706 = CARTESIAN_POINT ( 'NONE',  ( 791.9812246680005501, -428.6346026584192259, 361.9419747391813189 ) ) ;
#28707 = ORIENTED_EDGE ( 'NONE', *, *, #3269, .F. ) ;
#28708 =( LENGTH_UNIT ( ) NAMED_UNIT ( * ) SI_UNIT ( .MILLI., .METRE. ) );
#28709 = CARTESIAN_POINT ( 'NONE',  ( 772.4837098697144029, -263.3618753856924855, -374.5518280994205611 ) ) ;
#28710 = CARTESIAN_POINT ( 'NONE',  ( 759.0252816721024374, -168.9982390220563673, 368.0189434323527280 ) ) ;
#28711 = CARTESIAN_POINT ( 'NONE',  ( 761.4292242960306112, -257.4636090269708575, 323.2154366446414429 ) ) ;
#28712 = CARTESIAN_POINT ( 'NONE',  ( 760.5453621957607311, -381.0783235625954717, 323.8424801807151425 ) ) ;
#28713 = ORIENTED_EDGE ( 'NONE', *, *, #19085, .F. ) ;
#28714 = CARTESIAN_POINT ( 'NONE',  ( 802.5472867521000353, -76.37269993606228979, -350.8726784830461156 ) ) ;
#28715 = CARTESIAN_POINT ( 'NONE',  ( 813.2346286133761168, -197.2601417444143124, 328.9521613784389160 ) ) ;
#28716 = CARTESIAN_POINT ( 'NONE',  ( 765.0180583372156207, -240.9982390220561683, -360.0135310231089534 ) ) ;
#28717 = ORIENTED_EDGE ( 'NONE', *, *, #30033, .F. ) ;
#28718 = AXIS2_PLACEMENT_3D ( 'NONE', #10159, #24923, #28385 ) ;
#28719 = CARTESIAN_POINT ( 'NONE',  ( 768.0187753319979720, -344.6346026584195101, -318.0580252608186242 ) ) ;
#28720 = CARTESIAN_POINT ( 'NONE',  ( 803.4237431249931660, -39.18005720387496638, -331.2633955100225194 ) ) ;
#28721 = EDGE_CURVE ( 'NONE', #15902, #29488, #12901, .T. ) ;
#28722 = CARTESIAN_POINT ( 'NONE',  ( 800.7704444035546203, -244.1692326535050768, 326.0291762391768771 ) ) ;
#28723 = LINE ( 'NONE', #11162, #30711 ) ;
#28724 = LINE ( 'NONE', #32421, #39617 ) ;
#28725 = ORIENTED_EDGE ( 'NONE', *, *, #11140, .F. ) ;
#28726 = CARTESIAN_POINT ( 'NONE',  ( 755.5713283507202505, -29.36187538569318178, -334.6858677611754729 ) ) ;
#28727 = DIRECTION ( 'NONE',  ( 0.000000000000000000, 0.000000000000000000, 1.000000000000000000 ) ) ;
#28728 = CARTESIAN_POINT ( 'NONE',  ( -78.83651009197140525, 258.0940000000000509, -193.8809999999935769 ) ) ;
#28729 = ORIENTED_EDGE ( 'NONE', *, *, #14961, .F. ) ;
#28730 = CARTESIAN_POINT ( 'NONE',  ( 786.2694204179717872, -261.2817908451526705, -305.1769319972829067 ) ) ;
#28731 = CARTESIAN_POINT ( 'NONE',  ( 771.3260364891663130, -163.6454272087893003, 306.0683387631859773 ) ) ;
#28733 = CARTESIAN_POINT ( 'NONE',  ( 756.3353852180819104, -245.9073299311469896, -331.1735550268788302 ) ) ;
#28732 = CARTESIAN_POINT ( 'NONE',  ( 959.5497976682736407, 239.9999999999998863, -209.9999999999999716 ) ) ;
#28734 = CARTESIAN_POINT ( 'NONE',  ( 769.0155153010367712, -106.3726999360621903, -362.7791456095907279 ) ) ;
#28735 = EDGE_CURVE ( 'NONE', #38147, #17814, #29113, .T. ) ;
#28736 = CARTESIAN_POINT ( 'NONE',  ( 795.8262568251477660, -382.3726999360613945, 308.3538107759623585 ) ) ;
#28737 = DIRECTION ( 'NONE',  ( 1.892425610156518354E-16, 1.000000000000000000, -0.000000000000000000 ) ) ;
#28738 = CARTESIAN_POINT ( 'NONE',  ( 814.9108240113580450, -328.2709662947831362, -337.5031285880265273 ) ) ;
#28739 = CARTESIAN_POINT ( 'NONE',  ( 181.1634899080285948, 230.0000000000000000, -197.2499999999955662 ) ) ;
#28740 = CARTESIAN_POINT ( 'NONE',  ( 757.8323909638827445, -26.63460265842045871, 352.1044303154654358 ) ) ;
#28741 = CARTESIAN_POINT ( 'NONE',  ( 804.1009440267234822, -263.4636090269708006, 314.0944755984392600 ) ) ;
#28742 = CARTESIAN_POINT ( 'NONE',  ( 746.0683387631852383, -211.4419599262324709, -331.3260364891676204 ) ) ;
#28743 = CARTESIAN_POINT ( 'NONE',  ( 759.0252816721024374, -216.9982390220562252, 368.0189434323527280 ) ) ;
#28744 = CARTESIAN_POINT ( 'NONE',  ( 751.9810565676468741, -434.0891481129646081, -360.9747183278973921 ) ) ;
#28745 = DIRECTION ( 'NONE',  ( -0.000000000000000000, -0.000000000000000000, 1.000000000000000000 ) ) ;
#28746 = CARTESIAN_POINT ( 'NONE',  ( 785.3141322388236176, -309.7255117493287457, 364.4286716492789537 ) ) ;
#28747 = CARTESIAN_POINT ( 'NONE',  ( 779.4763451958990572, -80.73633629969864955, 365.0264073115438919 ) ) ;
#28748 = CARTESIAN_POINT ( 'NONE',  ( 769.9779781133707957, -91.09997266333496668, 316.7813123517150871 ) ) ;
#28749 = CARTESIAN_POINT ( 'NONE',  ( 764.0069404352550464, 8.921676437403235127, -359.2566176426627180 ) ) ;
#28750 = VECTOR ( 'NONE', #42335, 1000.000000000000000 ) ;
#28751 = DIRECTION ( 'NONE',  ( -1.000000000000000000, -4.625929269271485914E-16, -0.000000000000000000 ) ) ;
#28752 = DIRECTION ( 'NONE',  ( 1.000000000000000000, 0.000000000000000000, 0.000000000000000000 ) ) ;
#28754 = CARTESIAN_POINT ( 'NONE',  ( 785.3687786644884454, -347.3618753856922012, 315.3201227861279676 ) ) ;
#28753 = CARTESIAN_POINT ( 'NONE',  ( 761.2382568024794409, -159.6237781080508285, 356.9571628226838129 ) ) ;
#28755 = ORIENTED_EDGE ( 'NONE', *, *, #34585, .F. ) ;
#28756 = CARTESIAN_POINT ( 'NONE',  ( 803.8651313633788504, -293.2601417444139429, -332.4468031744301015 ) ) ;
#28757 = CARTESIAN_POINT ( 'NONE',  ( 771.1735550268778070, -129.1800572038746111, 316.3353852180827630 ) ) ;
#28758 = CARTESIAN_POINT ( 'NONE',  ( 771.2368401574024119, -301.4419599262320730, -374.2805881961240857 ) ) ;
#28759 = CARTESIAN_POINT ( 'NONE',  ( 831.1634899080286232, 239.9999999999998863, -199.9999999999999432 ) ) ;
#28760 = CARTESIAN_POINT ( 'NONE',  ( 773.7943932421234194, -431.8055962898681059, 305.5313806188329409 ) ) ;
#28761 = EDGE_LOOP ( 'NONE', ( #668, #18993 ) ) ;
#28762 = CARTESIAN_POINT ( 'NONE',  ( 797.6776695296629214, -331.5436935675104451, 357.6776695296636603 ) ) ;
#28763 = CARTESIAN_POINT ( 'NONE',  ( 786.6156483768007774, -73.44195992623286884, -315.5913626894246136 ) ) ;
#28764 = CARTESIAN_POINT ( 'NONE',  ( 759.7806653035534055, -174.9982390220563673, -324.8639956371180801 ) ) ;
#28765 = CARTESIAN_POINT ( 'NONE',  ( 767.8955696845333705, -192.4527844766016926, -362.1676090361162323 ) ) ;
#28766 = CARTESIAN_POINT ( 'NONE',  ( 762.3223304703356007, -439.5436935675101040, 322.3223304703362828 ) ) ;
#28767 = CARTESIAN_POINT ( 'NONE',  ( 755.2512626584698410, -151.5436935675109851, -315.2512626584710915 ) ) ;
#28768 = ORIENTED_EDGE ( 'NONE', *, *, #36127, .F. ) ;
#28769 = CARTESIAN_POINT ( 'NONE',  ( 785.3687786644885591, -155.3618753856927697, -315.3201227861280813 ) ) ;
#28770 = VERTEX_POINT ( 'NONE', #40625 ) ;
#28771 = CARTESIAN_POINT ( 'NONE',  ( 759.0159684113467620, -376.9181544815159555, -325.8855110935213020 ) ) ;
#28772 = CARTESIAN_POINT ( 'NONE',  ( 768.0187753319979720, -8.634602658420517329, 318.0580252608186242 ) ) ;
#28773 = CARTESIAN_POINT ( 'NONE',  ( 814.9108240113580450, -232.2709662947834488, 337.5031285880265273 ) ) ;
#28774 = CARTESIAN_POINT ( 'NONE',  ( 776.9566956441375396, -108.8965053807782084, 364.8461984189686405 ) ) ;
#28777 = CARTESIAN_POINT ( 'NONE',  ( 807.5423716828161105, -393.0783235625954717, 362.2119215644372048 ) ) ;
#28776 = DIRECTION ( 'NONE',  ( 0.000000000000000000, 0.000000000000000000, 1.000000000000000000 ) ) ;
#28775 = CARTESIAN_POINT ( 'NONE',  ( 939.9999999999993179, -590.0000000000001137, 350.0000000000000000 ) ) ;
#28778 = ORIENTED_EDGE ( 'NONE', *, *, #4722, .T. ) ;
#28779 = CARTESIAN_POINT ( 'NONE',  ( 763.0428371773158460, -395.4636090269705164, -358.7617431975195359 ) ) ;
#28780 = CARTESIAN_POINT ( 'NONE',  ( 784.9999999999992042, 240.0000000000000284, -275.0000000000000000 ) ) ;
#28781 = CARTESIAN_POINT ( 'NONE',  ( 757.7880784355613741, -186.0090635724255890, -312.4576283171834916 ) ) ;
#28782 = CARTESIAN_POINT ( 'NONE',  ( 768.9521613784389729, -33.82724539060788516, 373.2346286133773106 ) ) ;
#28784 = CARTESIAN_POINT ( 'NONE',  ( -208.8365100919714052, 256.5000000000001137, -197.2499999999927809 ) ) ;
#28783 = FACE_OUTER_BOUND ( 'NONE', #13467, .T. ) ;
#28785 = CARTESIAN_POINT ( 'NONE',  ( 803.2186876482843445, -343.9874144716865771, -350.0220218866286928 ) ) ;
#28786 = FACE_OUTER_BOUND ( 'NONE', #8435, .T. ) ;
#28787 = CARTESIAN_POINT ( 'NONE',  ( 812.3518521366052028, -193.0999726633346256, -326.5853460496235243 ) ) ;
#28788 = DIRECTION ( 'NONE',  ( -0.000000000000000000, 1.000000000000000000, -0.000000000000000000 ) ) ;
#28789 = DIRECTION ( 'NONE',  ( 0.000000000000000000, -1.000000000000000000, 0.000000000000000000 ) ) ;
#28790 = CARTESIAN_POINT ( 'NONE',  ( 804.6971507214547046, -363.2817908451523294, 344.0799538623459739 ) ) ;
#28791 = CARTESIAN_POINT ( 'NONE',  ( 778.7629533639073998, -320.7363362996979390, 375.0009284576466371 ) ) ;
#28792 = CARTESIAN_POINT ( 'NONE',  ( 782.5225473063383106, -214.2709662947834772, -375.2698199232970637 ) ) ;
#28793 = DIRECTION ( 'NONE',  ( 0.000000000000000000, -0.000000000000000000, -1.000000000000000000 ) ) ;
#28794 = CARTESIAN_POINT ( 'NONE',  ( 758.0580252608178853, -30.45278447660226817, -328.0187753319985404 ) ) ;
#28795 = CARTESIAN_POINT ( 'NONE',  ( 786.2694204179717872, -141.2817908451530400, 305.1769319972829067 ) ) ;
#28796 = CARTESIAN_POINT ( 'NONE',  ( 813.2346286133761168, -101.2601417444146250, -328.9521613784389160 ) ) ;
#28797 = CARTESIAN_POINT ( 'NONE',  ( 812.7932403749906598, -111.1800572038747532, 327.7687537140311633 ) ) ;
#28798 = CARTESIAN_POINT ( 'NONE',  ( 813.1304606946830518, -329.9073299311467053, -352.3570229623690580 ) ) ;
#28799 = LINE ( 'NONE', #11244, #7723 ) ;
#28800 = CARTESIAN_POINT ( 'NONE',  ( 786.4999999999993179, -544.8427095258973623, -350.0000000000000000 ) ) ;
#28801 = CARTESIAN_POINT ( 'NONE',  ( 803.6646147819161570, -209.9073299311470748, 348.8264449731210561 ) ) ;
#28802 = CARTESIAN_POINT ( 'NONE',  ( 793.9708237608222134, 1.081845518482914104, 319.2295555964448681 ) ) ;
#28803 = CARTESIAN_POINT ( 'NONE',  ( 813.9316612368132837, -415.4419599262318457, -348.6739635108323228 ) ) ;
#28804 = CARTESIAN_POINT ( 'NONE',  ( 746.8695393053150156, -413.9073299311465348, -327.6429770376306010 ) ) ;
#28805 = CARTESIAN_POINT ( 'NONE',  ( -26.63011601220122060, -110.5936016518799221, 750.6326042729449455 ) ) ;
#28806 = CARTESIAN_POINT ( 'NONE',  ( 764.3348316497523456, -46.71468719896022748, 308.6759233522265617 ) ) ;
#28807 = ORIENTED_EDGE ( 'NONE', *, *, #22728, .T. ) ;
#28808 = CARTESIAN_POINT ( 'NONE',  ( 778.2165204200184689, -118.8164208402383508, -364.9363028652563230 ) ) ;
#28809 = CARTESIAN_POINT ( 'NONE',  ( 754.8072714833581358, -28.81642084023863148, 338.1981804954720587 ) ) ;
#28810 = CARTESIAN_POINT ( 'NONE',  ( 807.5423716828161105, -177.0783235625961538, -362.2119215644372048 ) ) ;
#28811 = CARTESIAN_POINT ( 'NONE',  ( 815.0009284576459549, -294.3510508353230648, 338.7629533639073429 ) ) ;
#28812 = CARTESIAN_POINT ( 'NONE',  ( 797.8594530101009923, -157.5436935675109282, 322.1405469898982119 ) ) ;
#28813 = ORIENTED_EDGE ( 'NONE', *, *, #13974, .F. ) ;
#28814 = CARTESIAN_POINT ( 'NONE',  ( 797.8594530101008786, -349.5436935675102745, 322.1405469898980982 ) ) ;
#28815 = CARTESIAN_POINT ( 'NONE',  ( 751.9810565676468741, -50.08914811296584446, -360.9747183278973921 ) ) ;
#28816 = CARTESIAN_POINT ( 'NONE',  ( 796.7737145352015204, -68.63460265842033436, 370.7187646348536987 ) ) ;
#28817 = VERTEX_POINT ( 'NONE', #16133 ) ;
#28818 = CARTESIAN_POINT ( 'NONE',  ( 796.2681130854250569, -462.7578698805381237, -371.0719813302654870 ) ) ;
#28819 = VERTEX_POINT ( 'NONE', #33911 ) ;
#28820 = CONTEXT_DEPENDENT_SHAPE_REPRESENTATION ( #29932, #30663 ) ;
#28822 = CARTESIAN_POINT ( 'NONE',  ( 755.8894580844503253, -327.8272453906069472, 332.3691319403863531 ) ) ;
#28821 = CARTESIAN_POINT ( 'NONE',  ( 774.6312213355099630, -71.36187538569302546, 364.6798772138717482 ) ) ;
#28823 = CARTESIAN_POINT ( 'NONE',  ( 795.1360043628807261, -284.0891481129650629, -360.2193346964456282 ) ) ;
#28825 = CARTESIAN_POINT ( 'NONE',  ( 758.0141637701419768, -279.0783235625958127, 367.2620300519063790 ) ) ;
#28824 = CARTESIAN_POINT ( 'NONE',  ( 792.2312462859673587, -395.9073299311465348, 307.2067596250082602 ) ) ;
#28826 = CARTESIAN_POINT ( 'NONE',  ( 751.2241431872005251, -64.16923265350563099, 359.9636004259367610 ) ) ;
#28827 = CARTESIAN_POINT ( 'NONE',  ( 757.0176451133909268, -301.0999726633342561, -349.9200121543848354 ) ) ;
#28828 = CARTESIAN_POINT ( 'NONE',  ( 795.1360043628807261, -284.0891481129650629, -360.2193346964456282 ) ) ;
#28829 = LINE ( 'NONE', #31606, #3938 ) ;
#28830 = CARTESIAN_POINT ( 'NONE',  ( 785.3687786644884454, -107.3618753856928976, -315.3201227861279676 ) ) ;
#28831 = ADVANCED_FACE ( 'NONE', ( #26304 ), #11997, .T. ) ;
#28832 = DIRECTION ( 'NONE',  ( -0.000000000000000000, 1.000000000000000000, -0.000000000000000000 ) ) ;
#28833 = ORIENTED_EDGE ( 'NONE', *, *, #40526, .F. ) ;
#28834 = CARTESIAN_POINT ( 'NONE',  ( 814.2001403089898304, -377.3618753856920875, 347.4397851343538264 ) ) ;
#28835 = CARTESIAN_POINT ( 'NONE',  ( 939.9999999999993179, -600.0000000000001137, -360.0000000000000000 ) ) ;
#28836 = CARTESIAN_POINT ( 'NONE',  ( 807.2620300519052989, -96.00906357242585898, -318.0141637701419768 ) ) ;
#28837 = DIRECTION ( 'NONE',  ( -1.000000000000000000, -0.000000000000000000, 0.000000000000000000 ) ) ;
#28838 = PLANE ( 'NONE',  #20082 ) ;
#28839 = CARTESIAN_POINT ( 'NONE',  ( 757.0176451133909268, -277.0999726633344267, 349.9200121543848354 ) ) ;
#28840 = CARTESIAN_POINT ( 'NONE',  ( 800.0135310231082713, -158.0891481129655176, 325.0180583372163028 ) ) ;
#28841 = ORIENTED_EDGE ( 'NONE', *, *, #317, .F. ) ;
#28842 = CARTESIAN_POINT ( 'NONE',  ( 783.0745993439762742, -32.19088175424425913, -365.1016975059196739 ) ) ;
#28843 = CARTESIAN_POINT ( 'NONE',  ( 792.3570229623691148, -117.1800572038747106, -373.1304606946836770 ) ) ;
#28844 = CARTESIAN_POINT ( 'NONE',  ( 801.3366627262608972, -320.5328690171411949, 353.0897708529566899 ) ) ;
#28845 = DIRECTION ( 'NONE',  ( 0.000000000000000000, -1.000000000000000000, 0.000000000000000000 ) ) ;
#28846 = CARTESIAN_POINT ( 'NONE',  ( 809.0717654672305343, -52.91815448151692891, 360.1688906516309885 ) ) ;
#28847 = CARTESIAN_POINT ( 'NONE',  ( 804.7487373415286811, -235.5436935675107293, -364.7487373415288516 ) ) ;
#28848 = CARTESIAN_POINT ( 'NONE',  ( 763.0537975583475827, -192.4527844766016926, 371.0346526505627480 ) ) ;
#28849 = CARTESIAN_POINT ( 'NONE',  ( 771.2633955100217236, -119.9073299311474443, 363.4237431249939618 ) ) ;
#28850 = CARTESIAN_POINT ( 'NONE',  ( -786.4999999999993179, -512.9681489794448908, -339.9999999999999432 ) ) ;
#28851 = CARTESIAN_POINT ( 'NONE',  ( 795.6651683502461765, -322.7146871989593819, -371.3240766477733814 ) ) ;
#28852 = CARTESIAN_POINT ( 'NONE',  ( 815.3608509340175488, -434.7363362996975980, 341.2497674668889545 ) ) ;
#28853 = CARTESIAN_POINT ( 'NONE',  ( 814.5518280994195948, -327.7255117493285184, -332.4837098697145734 ) ) ;
#28854 = DIRECTION ( 'NONE',  ( 0.000000000000000000, 0.000000000000000000, -1.000000000000000000 ) ) ;
#28855 = CARTESIAN_POINT ( 'NONE',  ( 756.7813123517142913, -355.9874144716865203, 329.9779781133712504 ) ) ;
#28856 = CARTESIAN_POINT ( 'NONE',  ( 814.9108240113580450, -64.27096629478397460, 337.5031285880265273 ) ) ;
#28857 = CARTESIAN_POINT ( 'NONE',  ( 756.5762568750052424, -411.1800572038738437, -348.7366044899774238 ) ) ;
#28858 = CARTESIAN_POINT ( 'NONE',  ( 757.2208543904082489, -40.71468719896024879, 350.9844846989624330 ) ) ;
#28859 = CARTESIAN_POINT ( 'NONE',  ( 756.3353852180819104, -197.9073299311472169, -331.1735550268788302 ) ) ;
#28860 = CARTESIAN_POINT ( 'NONE',  ( 758.0141637701419768, -87.07832356259646645, -367.2620300519063790 ) ) ;
#28861 = CARTESIAN_POINT ( 'NONE',  ( 813.2346286133761168, -197.2601417444143124, 328.9521613784389160 ) ) ;
#28862 = CARTESIAN_POINT ( 'NONE',  ( 765.0180583372156207, -48.99823902205675807, 360.0135310231089534 ) ) ;
#28863 = ORIENTED_EDGE ( 'NONE', *, *, #12245, .F. ) ;
#28864 = CARTESIAN_POINT ( 'NONE',  ( 775.9200461376533440, -239.8055962898687028, -315.3028492785443291 ) ) ;
#28865 = CARTESIAN_POINT ( 'NONE',  ( 768.0187753319979720, -200.6346026584199365, 318.0580252608186242 ) ) ;
#28866 = EDGE_CURVE ( 'NONE', #23953, #20728, #26987, .T. ) ;
#28867 = CARTESIAN_POINT ( 'NONE',  ( 745.1769319972822814, -41.80559628986934229, -346.2694204179732083 ) ) ;
#28868 = CARTESIAN_POINT ( 'NONE',  ( 755.0636971347428243, -340.2709662947831362, 341.7834795799807353 ) ) ;
#28869 = DIRECTION ( 'NONE',  ( 0.000000000000000000, -1.000000000000000000, 0.000000000000000000 ) ) ;
#28870 = DIRECTION ( 'NONE',  ( -0.000000000000000000, 1.000000000000000000, -0.000000000000000000 ) ) ;
#28871 = ORIENTED_EDGE ( 'NONE', *, *, #29650, .F. ) ;
#28872 = CARTESIAN_POINT ( 'NONE',  ( 803.8651313633788504, -53.26014174441475291, 332.4468031744301015 ) ) ;
#28873 = CARTESIAN_POINT ( 'NONE',  ( 795.8262568251477660, -334.3726999360615082, -308.3538107759623585 ) ) ;
#28874 = ADVANCED_FACE ( 'NONE', ( #9439 ), #8538, .T. ) ;
#28875 = CARTESIAN_POINT ( 'NONE',  ( 767.7687537140311633, -287.9073299311468759, 372.7932403749916830 ) ) ;
#28876 = CARTESIAN_POINT ( 'NONE',  ( 795.6651683502461765, 13.28531280103958423, 371.3240766477733814 ) ) ;
#28877 = CARTESIAN_POINT ( 'NONE',  ( 769.0155153010367712, -178.3726999360619629, -362.7791456095907279 ) ) ;
#28878 = CARTESIAN_POINT ( 'NONE',  ( 768.0187753319979720, -176.6346026584199933, -318.0580252608186242 ) ) ;
#28879 = CARTESIAN_POINT ( 'NONE',  ( 771.2633955100217236, -359.9073299311467053, -363.4237431249939618 ) ) ;
#28880 = EDGE_CURVE ( 'NONE', #42700, #18319, #22605, .T. ) ;
#28881 = ORIENTED_EDGE ( 'NONE', *, *, #22448, .T. ) ;
#28882 = CARTESIAN_POINT ( 'NONE',  ( 808.0189434323515343, -302.0891481129650629, 319.0252816721025511 ) ) ;
#28883 = CARTESIAN_POINT ( 'NONE',  ( 51.16348990802859475, 258.0940000000000509, -199.9999999999945146 ) ) ;
#28884 = SHAPE_REPRESENTATION ( 'MirrorSlot', ( #26858 ), #7608 ) ;
#28885 = CARTESIAN_POINT ( 'NONE',  ( 763.2154366446407039, -357.6237781080501463, 321.4292242960311228 ) ) ;
#28886 = LINE ( 'NONE', #10643, #35935 ) ;
#28887 = CARTESIAN_POINT ( 'NONE',  ( 757.0176451133909268, -157.0999726633347962, 349.9200121543848354 ) ) ;
#28888 = CARTESIAN_POINT ( 'NONE',  ( 778.1981804954714335, -58.27096629478398171, 314.8072714833589885 ) ) ;
#28889 = ORIENTED_EDGE ( 'NONE', *, *, #17866, .F. ) ;
#28890 = CARTESIAN_POINT ( 'NONE',  ( 791.0478386215596629, -405.8272453906067199, -306.7653713866226326 ) ) ;
#28891 = CARTESIAN_POINT ( 'NONE',  ( 755.2512626584698410, 16.45630643248848912, -315.2512626584710915 ) ) ;
#28892 = CARTESIAN_POINT ( 'NONE',  ( 748.6759233522253680, -256.3726999360617924, 324.3348316497537098 ) ) ;
#28893 = CARTESIAN_POINT ( 'NONE',  ( 755.8398074228967971, -211.4419599262324709, 333.4516893846970333 ) ) ;
#28894 = CARTESIAN_POINT ( 'NONE',  ( 756.3353852180819104, -365.9073299311465917, -331.1735550268788302 ) ) ;
#28895 = CYLINDRICAL_SURFACE ( 'NONE', #10598, 18.00000000000001421 ) ;
#28896 = EDGE_CURVE ( 'NONE', #28228, #37728, #25639, .T. ) ;
#28897 = CARTESIAN_POINT ( 'NONE',  ( 787.5531968255692163, -453.8272453906066630, 316.1348686366205811 ) ) ;
#28898 = DIRECTION ( 'NONE',  ( 1.000000000000000000, 0.000000000000000000, 0.000000000000000000 ) ) ;
#28899 = CARTESIAN_POINT ( 'NONE',  ( 763.8424801807145741, -258.0090635724253616, -320.5453621957614700 ) ) ;
#28900 = CARTESIAN_POINT ( 'NONE',  ( 749.2812353651451076, -6.452784476602343666, 323.2262854647983090 ) ) ;
#28901 = ADVANCED_FACE ( 'NONE', ( #6653 ), #41773, .T. ) ;
#28902 = CARTESIAN_POINT ( 'NONE',  ( 744.7301800767019131, -100.8164208402383792, 337.4774526936615757 ) ) ;
#28903 = FACE_OUTER_BOUND ( 'NONE', #20098, .T. ) ;
#28904 = PLANE ( 'NONE',  #4066 ) ;
#28905 = SURFACE_STYLE_FILL_AREA ( #15046 ) ;
#28906 = CARTESIAN_POINT ( 'NONE',  ( 747.6481478633932056, -397.0999726633340288, 353.4146539503763620 ) ) ;
#28907 = LINE ( 'NONE', #18976, #17643 ) ;
#28908 = CARTESIAN_POINT ( 'NONE',  ( 811.0346526505616112, -326.6346026584193396, 323.0537975583477532 ) ) ;
#28909 = CARTESIAN_POINT ( 'NONE',  ( 803.4237431249931660, -327.1800572038741279, -331.2633955100225194 ) ) ;
#28910 = FACE_OUTER_BOUND ( 'NONE', #7233, .T. ) ;
#28911 = CARTESIAN_POINT ( 'NONE',  ( 792.1044303154645831, -444.4527844766009821, 317.8323909638837677 ) ) ;
#28912 = AXIS2_PLACEMENT_3D ( 'NONE', #33, #27300, #2819 ) ;
#28913 = CARTESIAN_POINT ( 'NONE',  ( 798.5707757039680246, -173.4636090269710849, 356.7845633553585003 ) ) ;
#28914 = CARTESIAN_POINT ( 'NONE',  ( 807.2620300519052989, -48.00906357242602951, -318.0141637701419768 ) ) ;
#28915 = CARTESIAN_POINT ( 'NONE',  ( 776.9566956441375396, -84.89650538077830788, -364.8461984189686405 ) ) ;
#28916 = CARTESIAN_POINT ( 'NONE',  ( 771.2368401574024119, -85.44195992623282621, 374.2805881961240857 ) ) ;
#28917 = FACE_OUTER_BOUND ( 'NONE', #8158, .T. ) ;
#28918 = EDGE_CURVE ( 'NONE', #17814, #346, #2494, .T. ) ;
#28919 = AXIS2_PLACEMENT_3D ( 'NONE', #2716, #34348, #34583 ) ;
#28920 = CARTESIAN_POINT ( 'NONE',  ( 761.9338519418445230, -158.5328690171417065, 370.4231160770881957 ) ) ;
#28921 = CARTESIAN_POINT ( 'NONE',  ( 785.3141322388236176, 2.274488250670355871, -364.4286716492789537 ) ) ;
#28923 = ORIENTED_EDGE ( 'NONE', *, *, #21631, .T. ) ;
#28922 = CARTESIAN_POINT ( 'NONE',  ( 755.0488828828309806, -113.8055962898691149, -344.1219089521771934 ) ) ;
#28924 = CARTESIAN_POINT ( 'NONE',  ( 801.9419747391806368, -90.45278447660209054, -351.9812246680014027 ) ) ;
#28925 = ADVANCED_FACE ( 'NONE', ( #23957 ), #45698, .T. ) ;
#28926 = CARTESIAN_POINT ( 'NONE',  ( 760.5453621957607311, -405.0783235625954148, -323.8424801807151425 ) ) ;
#28928 = CARTESIAN_POINT ( 'NONE',  ( 762.1405469898973024, -241.5436935675106440, 357.8594530101016176 ) ) ;
#28927 = CARTESIAN_POINT ( 'NONE',  ( 755.3201227861273992, -267.7255117493286320, 345.3687786644892981 ) ) ;
#28929 = CARTESIAN_POINT ( 'NONE',  ( -26.63011601220122060, -513.1383975375929367, -369.9999999999999432 ) ) ;
#28930 = ORIENTED_EDGE ( 'NONE', *, *, #23320, .T. ) ;
#28931 = CARTESIAN_POINT ( 'NONE',  ( 758.0580252608178853, -438.4527844766009821, 328.0187753319985404 ) ) ;
#28932 = ORIENTED_EDGE ( 'NONE', *, *, #1261, .F. ) ;
#28933 = EDGE_CURVE ( 'NONE', #10119, #13600, #23726, .T. ) ;
#28934 = EDGE_CURVE ( 'NONE', #5389, #30216, #6188, .T. ) ;
#28935 = CARTESIAN_POINT ( 'NONE',  ( 748.9653473494365699, -170.6346026584199933, 356.9462024416520762 ) ) ;
#28936 = CARTESIAN_POINT ( 'NONE',  ( 775.8780910478218402, -249.2817908451526421, 364.9511171171680530 ) ) ;
#28937 = VERTEX_POINT ( 'NONE', #41999 ) ;
#28938 = CARTESIAN_POINT ( 'NONE',  ( 804.1105419155481968, -75.82724539060775726, -347.6308680596136469 ) ) ;
#28939 = CARTESIAN_POINT ( 'NONE',  ( 744.9990715423526808, -234.3510508353232638, 341.2370466360926002 ) ) ;
#28940 = CARTESIAN_POINT ( 'NONE',  ( 791.9812246680005501, -236.6346026584198228, -361.9419747391813189 ) ) ;
#28941 = ORIENTED_EDGE ( 'NONE', *, *, #38237, .T. ) ;
#28942 = CARTESIAN_POINT ( 'NONE',  ( 781.8018195045266339, -382.2709662947828519, -365.1927285166406705 ) ) ;
#28943 = CARTESIAN_POINT ( 'NONE',  ( 788.7366044899766848, -35.90732993114770011, -316.5762568750059813 ) ) ;
#28944 = CARTESIAN_POINT ( 'NONE',  ( 773.3843516231979720, -253.4419599262323572, 364.4086373105754433 ) ) ;
#28945 = LINE ( 'NONE', #1882, #43285 ) ;
#28946 = CARTESIAN_POINT ( 'NONE',  ( 771.1735550268778070, -9.180057203875058747, -316.3353852180827630 ) ) ;
#28947 = DIRECTION ( 'NONE',  ( -1.880165489482579047E-16, -1.000000000000000000, -0.000000000000000000 ) ) ;
#28948 = VERTEX_POINT ( 'NONE', #38077 ) ;
#28949 = CARTESIAN_POINT ( 'NONE',  ( 747.6481478633932056, -325.0999726633342561, -353.4146539503763620 ) ) ;
#28950 = AXIS2_PLACEMENT_3D ( 'NONE', #45141, #3333, #38215 ) ;
#28951 = EDGE_CURVE ( 'NONE', #30414, #8827, #20577, .T. ) ;
#28952 = CARTESIAN_POINT ( 'NONE',  ( 755.8990559732751535, -179.4636090269710849, 365.9055244015606831 ) ) ;
#28954 = CARTESIAN_POINT ( 'NONE',  ( 759.7806653035534055, -270.9982390220561115, -324.8639956371180801 ) ) ;
#28953 = CARTESIAN_POINT ( 'NONE',  ( 999.9999999999992042, 248.9999999999998863, 200.9999999999999432 ) ) ;
#28955 = EDGE_CURVE ( 'NONE', #9099, #30459, #30544, .T. ) ;
#28956 = CARTESIAN_POINT ( 'NONE',  ( 914.9999999999992042, 99.99999999999984368, 360.0000000000000000 ) ) ;
#28957 = CARTESIAN_POINT ( 'NONE',  ( 772.4468031744293057, -153.8272453906075157, -363.8651313633793620 ) ) ;
#28958 = EDGE_CURVE ( 'NONE', #21104, #39743, #16835, .T. ) ;
#28959 = CARTESIAN_POINT ( 'NONE',  ( 767.6429770376289525, -9.180057203875058747, 306.8695393053162093 ) ) ;
#28960 = CARTESIAN_POINT ( 'NONE',  ( 759.9999999999992042, -512.9681489794448908, 370.0000000000000000 ) ) ;
#28961 = CARTESIAN_POINT ( 'NONE',  ( 763.0537975583476964, -336.4527844766012663, -371.0346526505628617 ) ) ;
#28962 = CARTESIAN_POINT ( 'NONE',  ( 759.9999999999992042, 205.0000000000000568, -319.9999999999999432 ) ) ;
#28963 = CARTESIAN_POINT ( 'NONE',  ( 803.4237431249931660, -15.18005720387504631, 331.2633955100225194 ) ) ;
#28964 = CARTESIAN_POINT ( 'NONE',  ( 781.2370466360911223, -284.7363362996979390, 304.9990715423533629 ) ) ;
#28965 = CARTESIAN_POINT ( 'NONE',  ( 749.8865473780648472, -212.5328690171415076, -322.1177392798429082 ) ) ;
#28966 = CARTESIAN_POINT ( 'NONE',  ( 777.5031285880264704, -238.8164208402379813, 374.9108240113588408 ) ) ;
#28967 = CARTESIAN_POINT ( 'NONE',  ( 792.2269492836462632, -443.1233509495419298, -372.8191558162650949 ) ) ;
#28968 = CARTESIAN_POINT ( 'NONE',  ( 779.9999999999993179, -513.1383975375929367, -367.9999999999999432 ) ) ;
#28969 = CARTESIAN_POINT ( 'NONE',  ( 779.9999999999992042, 126.4563064324884465, 350.0000000000000000 ) ) ;
#28970 = CARTESIAN_POINT ( 'NONE',  ( 755.0636971347428243, -316.2709662947832499, 341.7834795799807353 ) ) ;
#28971 = VECTOR ( 'NONE', #21913, 1000.000000000000000 ) ;
#28972 = EDGE_CURVE ( 'NONE', #9876, #16943, #1047, .T. ) ;
#28973 = CARTESIAN_POINT ( 'NONE',  ( 766.9102291470427417, -90.55451811788041994, 318.6633372737382501 ) ) ;
#28974 = CARTESIAN_POINT ( 'NONE',  ( 760.5453621957607311, 2.921676437403253779, -323.8424801807151425 ) ) ;
#28975 = CYLINDRICAL_SURFACE ( 'NONE', #7065, 7.999999999999896083 ) ;
#28976 = EDGE_CURVE ( 'NONE', #44542, #16836, #20515, .T. ) ;
#28977 = LINE ( 'NONE', #7729, #22534 ) ;
#28979 = CARTESIAN_POINT ( 'NONE',  ( 800.0135310231082713, -374.0891481129647786, 325.0180583372163028 ) ) ;
#28978 = CARTESIAN_POINT ( 'NONE',  ( 790.8726784830453198, -154.7146871989598935, 362.5472867521010585 ) ) ;
#28980 = ORIENTED_EDGE ( 'NONE', *, *, #22881, .F. ) ;
#28981 = EDGE_CURVE ( 'NONE', #2255, #8421, #42218, .T. ) ;
#28982 = CARTESIAN_POINT ( 'NONE',  ( 794.1144889064781864, -298.1692326535049347, -360.9840315886528401 ) ) ;
#28983 = CARTESIAN_POINT ( 'NONE',  ( 748.3538107759620743, -280.7146871989594956, -355.8262568251490165 ) ) ;
#28984 = DIRECTION ( 'NONE',  ( -1.000000000000000000, 0.000000000000000000, 0.000000000000000000 ) ) ;
#28985 = CARTESIAN_POINT ( 'NONE',  ( 793.9861285913068514, -442.9180389616178672, 372.1637643035757606 ) ) ;
#28986 = ORIENTED_EDGE ( 'NONE', *, *, #13710, .T. ) ;
#28987 = CARTESIAN_POINT ( 'NONE',  ( 762.1405469898971887, -313.5436935675102745, 357.8594530101015607 ) ) ;
#28988 = CARTESIAN_POINT ( 'NONE',  ( 755.0488828828309806, -65.80559628986925702, -344.1219089521771934 ) ) ;
#28989 = CARTESIAN_POINT ( 'NONE',  ( 791.9812246680005501, -428.6346026584192259, 361.9419747391813189 ) ) ;
#28990 = ADVANCED_FACE ( 'NONE', ( #6872 ), #13361, .T. ) ;
#28991 = CARTESIAN_POINT ( 'NONE',  ( 796.7737145352015204, -164.6346026584200217, -370.7187646348536987 ) ) ;
#28992 = ORIENTED_EDGE ( 'NONE', *, *, #25594, .T. ) ;
#28993 = CARTESIAN_POINT ( 'NONE',  ( 785.3141322388236176, -141.7255117493291721, -364.4286716492789537 ) ) ;
#28994 = ORIENTED_EDGE ( 'NONE', *, *, #14254, .T. ) ;
#28995 = CARTESIAN_POINT ( 'NONE',  ( 783.0745993439762742, -416.1908817542430938, -365.1016975059196739 ) ) ;
#28996 = CARTESIAN_POINT ( 'NONE',  ( 795.1360043628807261, 3.910851887033985896, 360.2193346964456282 ) ) ;
#28997 = CARTESIAN_POINT ( 'NONE',  ( 759.2295555964440155, -112.1692326535054889, 353.9708237608231229 ) ) ;
#29000 = CARTESIAN_POINT ( 'NONE',  ( 751.2241431872005251, -376.1692326535046504, 359.9636004259367610 ) ) ;
#28999 = CARTESIAN_POINT ( 'NONE',  ( -911.9749999999993406, 219.9999999999998863, 350.0000000000000000 ) ) ;
#28998 = DIRECTION ( 'NONE',  ( 0.000000000000000000, -1.000000000000000000, 0.000000000000000000 ) ) ;
#29001 = VERTEX_POINT ( 'NONE', #7611 ) ;
#29002 = CARTESIAN_POINT ( 'NONE',  ( 775.8780910478218402, -393.2817908451522726, -364.9511171171680530 ) ) ;
#29003 = LINE ( 'NONE', #43318, #27740 ) ;
#29004 = AXIS2_PLACEMENT_3D ( 'NONE', #36387, #4749, #15388 ) ;
#29005 = CARTESIAN_POINT ( 'NONE',  ( 757.7880784355613741, -210.0090635724255321, -312.4576283171834916 ) ) ;
#29006 =( GEOMETRIC_REPRESENTATION_CONTEXT ( 3 ) GLOBAL_UNCERTAINTY_ASSIGNED_CONTEXT ( ( #34873 ) ) GLOBAL_UNIT_ASSIGNED_CONTEXT ( ( #11832, #18085, #11149 ) ) REPRESENTATION_CONTEXT ( 'NONE', 'WORKASPACE' ) );
#29007 = CARTESIAN_POINT ( 'NONE',  ( 745.1792804349281596, -62.19088175424416676, 343.7566961878542884 ) ) ;
#29009 = DIRECTION ( 'NONE',  ( 1.000000000000000000, -0.000000000000000000, -0.000000000000000000 ) ) ;
#29008 = DIRECTION ( 'NONE',  ( 0.000000000000000000, 0.000000000000000000, 1.000000000000000000 ) ) ;
#29010 = CARTESIAN_POINT ( 'NONE',  ( 759.2295555964440155, -328.1692326535048210, -353.9708237608231229 ) ) ;
#29011 = CARTESIAN_POINT ( 'NONE',  ( 786.4999999999993179, -496.5085659523897448, -356.8883017825714319 ) ) ;
#29012 = CARTESIAN_POINT ( 'NONE',  ( 745.7194118038753459, -181.6454272087892434, -348.7631598425976449 ) ) ;
#29013 = DIRECTION ( 'NONE',  ( 0.000000000000000000, 0.000000000000000000, 1.000000000000000000 ) ) ;
#29014 = DIRECTION ( 'NONE',  ( 0.000000000000000000, -0.6594541114781782287, 0.7517448203044211352 ) ) ;
#29015 = CARTESIAN_POINT ( 'NONE',  ( 761.4292242960306112, -401.4636090269704027, 323.2154366446414429 ) ) ;
#29016 = CARTESIAN_POINT ( 'NONE',  ( 749.2812353651451076, -222.4527844766016642, -323.2262854647983090 ) ) ;
#29017 = CARTESIAN_POINT ( 'NONE',  ( -598.8365100919716042, 240.0000000000001705, -202.7499999999898250 ) ) ;
#29018 = CARTESIAN_POINT ( 'NONE',  ( 797.8594530101008786, -13.54369356751140785, -322.1405469898980982 ) ) ;
#29019 = PRESENTATION_LAYER_ASSIGNMENT (  '', '', ( #16474 ) ) ;
#29020 = CARTESIAN_POINT ( 'NONE',  ( 797.8822607201568644, -150.5545181178802352, 370.1134526219340160 ) ) ;
#29021 = CARTESIAN_POINT ( 'NONE',  ( 813.9316612368132837, -103.4419599262327836, -348.6739635108323228 ) ) ;
#29022 = CARTESIAN_POINT ( 'NONE',  ( 805.0032342141412300, -109.5436935675110988, 314.9967657858571783 ) ) ;
#29023 = CARTESIAN_POINT ( 'NONE',  ( 811.0346526505616112, -350.6346026584192828, -323.0537975583477532 ) ) ;
#29024 = DIRECTION ( 'NONE',  ( -0.000000000000000000, -0.000000000000000000, 1.000000000000000000 ) ) ;
#29025 = CARTESIAN_POINT ( 'NONE',  ( 115.7583438952258774, 430.0000000000002842, -244.9999999999999716 ) ) ;
#29026 = CARTESIAN_POINT ( 'NONE',  ( 771.2633955100217236, -215.9073299311471317, 363.4237431249939618 ) ) ;
#29027 = CARTESIAN_POINT ( 'NONE',  ( 764.1737431748507561, -442.3726999360611103, 371.6461892240376415 ) ) ;
#29028 = CARTESIAN_POINT ( 'NONE',  ( 786.2056067578752163, -419.8055962898681059, -374.4686193811670023 ) ) ;
#29029 = CARTESIAN_POINT ( 'NONE',  ( 810.7187646348534145, -426.4527844766010389, -356.7737145352016341 ) ) ;
#29030 = CARTESIAN_POINT ( 'NONE',  ( -37.63011601220122770, -355.4967352946684969, -16.45562775363632113 ) ) ;
#29031 = CARTESIAN_POINT ( 'NONE',  ( 746.0683387631852383, -19.44195992623303937, 331.3260364891676204 ) ) ;
#29032 = VERTEX_POINT ( 'NONE', #11302 ) ;
#29033 = CARTESIAN_POINT ( 'NONE',  ( 760.5453621957607311, -189.0783235625961822, -323.8424801807151425 ) ) ;
#29034 = CIRCLE ( 'NONE', #37121, 2.749999999999808153 ) ;
#29035 = CARTESIAN_POINT ( 'NONE',  ( 771.1735550268778070, -9.180057203875058747, 316.3353852180827630 ) ) ;
#29036 = CARTESIAN_POINT ( 'NONE',  ( 813.9316612368132837, -199.4419599262324709, -348.6739635108323228 ) ) ;
#29037 =( NAMED_UNIT ( * ) PLANE_ANGLE_UNIT ( ) SI_UNIT ( $, .RADIAN. ) );
#29038 = CARTESIAN_POINT ( 'NONE',  ( 744.8212110874229666, -330.8965053807774552, 336.2046728542121627 ) ) ;
#29039 = CARTESIAN_POINT ( 'NONE',  ( 755.5713283507202505, -149.3618753856928265, 334.6858677611754729 ) ) ;
#29040 = VECTOR ( 'NONE', #29786, 1000.000000000000000 ) ;
#29041 = ORIENTED_EDGE ( 'NONE', *, *, #39154, .T. ) ;
#29042 = CARTESIAN_POINT ( 'NONE',  ( 786.2056067578752163, -419.8055962898681059, 374.4686193811670023 ) ) ;
#29043 = CARTESIAN_POINT ( 'NONE',  ( 762.1405469898971887, -145.5436935675109851, -357.8594530101015607 ) ) ;
#29044 = CARTESIAN_POINT ( 'NONE',  ( 762.3223304703356007, -343.5436935675103314, 322.3223304703362828 ) ) ;
#29045 = CARTESIAN_POINT ( 'NONE',  ( 811.0346526505616112, -38.63460265842041252, -323.0537975583477532 ) ) ;
#29046 = ORIENTED_EDGE ( 'NONE', *, *, #37087, .F. ) ;
#29047 = CARTESIAN_POINT ( 'NONE',  ( 786.2694204179717872, -429.2817908451521021, -305.1769319972829067 ) ) ;
#29048 = ORIENTED_EDGE ( 'NONE', *, *, #9431, .T. ) ;
#29049 = CARTESIAN_POINT ( 'NONE',  ( 802.9823548866075953, -337.0999726633342561, -330.0799878456151077 ) ) ;
#29050 = AXIS2_PLACEMENT_3D ( 'NONE', #15545, #12312, #26155 ) ;
#29052 = CARTESIAN_POINT ( 'NONE',  ( 761.4292242960306112, -377.4636090269704596, 323.2154366446414429 ) ) ;
#29051 = CARTESIAN_POINT ( 'NONE',  ( 765.0180583372156207, -48.99823902205675807, 360.0135310231089534 ) ) ;
#29053 = CARTESIAN_POINT ( 'NONE',  ( 778.1981804954714335, -298.2709662947830793, -314.8072714833589885 ) ) ;
#29055 = CARTESIAN_POINT ( 'NONE',  ( 771.2368401574024119, -301.4419599262320730, 374.2805881961240857 ) ) ;
#29054 = CARTESIAN_POINT ( 'NONE',  ( 808.3070685750232087, -378.9982390220557136, 361.1904061080339829 ) ) ;
#29056 = CARTESIAN_POINT ( 'NONE',  ( 798.0661480581538854, -74.53286901714196233, 309.5768839229118043 ) ) ;
#29057 = CARTESIAN_POINT ( 'NONE',  ( 783.0745993439762742, -296.1908817542434917, -365.1016975059196739 ) ) ;
#29058 = CARTESIAN_POINT ( 'NONE',  ( 797.6776695296629214, -283.5436935675105019, -357.6776695296636603 ) ) ;
#29059 = FACE_BOUND ( 'NONE', #11630, .T. ) ;
#29060 = CARTESIAN_POINT ( 'NONE',  ( 774.6858677611749044, -105.7255117493293000, -315.5713283507209894 ) ) ;
#29061 = CARTESIAN_POINT ( 'NONE',  ( -784.4999999999993179, -355.4967352946684969, -16.45562775363623587 ) ) ;
#29062 = EDGE_LOOP ( 'NONE', ( #6160, #25415, #18536, #7112 ) ) ;
#29063 = CARTESIAN_POINT ( 'NONE',  ( 772.5602148656447525, -441.7255117493282910, 305.7998596910095443 ) ) ;
#29065 = DIRECTION ( 'NONE',  ( 0.000000000000000000, 0.000000000000000000, 1.000000000000000000 ) ) ;
#29064 = CARTESIAN_POINT ( 'NONE',  ( 999.9999999999992042, -599.0000000000001137, 360.0000000000000000 ) ) ;
#29066 = CARTESIAN_POINT ( 'NONE',  ( 783.7953271457878373, -80.19088175424411702, -375.1787889125761239 ) ) ;
#29067 = LINE ( 'NONE', #19128, #44772 ) ;
#29068 = CARTESIAN_POINT ( 'NONE',  ( -200.7583438952259485, 394.6698570112193920, -274.9999999999999432 ) ) ;
#29069 = CARTESIAN_POINT ( 'NONE',  ( 769.9779781133707957, -283.0999726633344267, 316.7813123517150871 ) ) ;
#29070 = CARTESIAN_POINT ( 'NONE',  ( 800.2193346964447755, -162.9982390220563673, 355.1360043628815788 ) ) ;
#29071 = ORIENTED_EDGE ( 'NONE', *, *, #15946, .F. ) ;
#29072 = AXIS2_PLACEMENT_3D ( 'NONE', #21625, #35708, #28793 ) ;
#29073 = VECTOR ( 'NONE', #32657, 1000.000000000000000 ) ;
#29074 = CARTESIAN_POINT ( 'NONE',  ( 745.0891759886404770, -100.2709662947838609, -342.4968714119734159 ) ) ;
#29075 = CARTESIAN_POINT ( 'NONE',  ( 757.2208543904082489, -328.7146871989592682, 350.9844846989624330 ) ) ;
#29076 = DIRECTION ( 'NONE',  ( -0.000000000000000000, 1.000000000000000000, -0.000000000000000000 ) ) ;
#29077 = CARTESIAN_POINT ( 'NONE',  ( 814.8207195650702488, -26.19088175424427334, 336.2433038121456548 ) ) ;
#29078 = CARTESIAN_POINT ( 'NONE',  ( 745.0891759886404770, -244.2709662947834204, -342.4968714119734159 ) ) ;
#29079 = CARTESIAN_POINT ( 'NONE',  ( 800.2193346964447755, -114.9982390220565236, 355.1360043628815788 ) ) ;
#29080 = CARTESIAN_POINT ( 'NONE',  ( -928.0249999999991815, 219.9999999999998863, 339.9999999999999432 ) ) ;
#29081 = CARTESIAN_POINT ( 'NONE',  ( 756.1443688327750579, -309.6237781080502600, -314.3581564841659315 ) ) ;
#29082 = CIRCLE ( 'NONE', #17268, 18.00000000000001421 ) ;
#29083 = CARTESIAN_POINT ( 'NONE',  ( 815.3608509340175488, -458.7363362996973706, 341.2497674668889545 ) ) ;
#29084 = CARTESIAN_POINT ( 'NONE',  ( 804.7487373415286811, -307.5436935675104451, -364.7487373415288516 ) ) ;
#29085 = DIRECTION ( 'NONE',  ( -1.000000000000000000, -0.000000000000000000, 0.000000000000000000 ) ) ;
#29086 = CARTESIAN_POINT ( 'NONE',  ( 759.2295555964440155, -400.1692326535045936, 353.9708237608231229 ) ) ;
#29087 = ORIENTED_EDGE ( 'NONE', *, *, #8323, .T. ) ;
#29088 = CARTESIAN_POINT ( 'NONE',  ( 788.7366044899766848, -419.9073299311465348, -316.5762568750059813 ) ) ;
#29089 = CARTESIAN_POINT ( 'NONE',  ( 755.5713283507202505, -221.3618753856925707, -334.6858677611754729 ) ) ;
#29090 = EDGE_CURVE ( 'NONE', #16032, #17925, #40156, .T. ) ;
#29091 = CARTESIAN_POINT ( 'NONE',  ( 756.1443688327750579, -93.62377810805098477, -314.3581564841659315 ) ) ;
#29092 = CARTESIAN_POINT ( 'NONE',  ( 879.9999999999992042, 429.9999999999999432, -244.9999999999999716 ) ) ;
#29093 = CARTESIAN_POINT ( 'NONE',  ( 751.2241431872005251, -232.1692326535051620, 359.9636004259367610 ) ) ;
#29094 = CARTESIAN_POINT ( 'NONE',  ( 785.3687786644885591, -35.36187538569316047, 315.3201227861280813 ) ) ;
#29095 = EDGE_LOOP ( 'NONE', ( #24467, #13258, #34655, #33624 ) ) ;
#29096 = CARTESIAN_POINT ( 'NONE',  ( 795.9930595647434757, -243.0783235625959833, -320.7433823573372820 ) ) ;
#29097 = CARTESIAN_POINT ( 'NONE',  ( 755.0636971347428243, -220.2709662947834772, 341.7834795799807353 ) ) ;
#29098 = CIRCLE ( 'NONE', #7081, 4.999999999999984901 ) ;
#29099 = CARTESIAN_POINT ( 'NONE',  ( 761.9338519418445230, -62.53286901714199786, -370.4231160770881957 ) ) ;
#29100 = CARTESIAN_POINT ( 'NONE',  ( 805.1927285166399315, -352.8164208402375266, 341.8018195045277707 ) ) ;
#29101 = CARTESIAN_POINT ( 'NONE',  ( 809.6099558218720631, -452.9681489794449476, -335.1781210895659342 ) ) ;
#29102 = AXIS2_PLACEMENT_3D ( 'NONE', #32138, #22192, #11590 ) ;
#29103 = ORIENTED_EDGE ( 'NONE', *, *, #36433, .T. ) ;
#29104 = CARTESIAN_POINT ( 'NONE',  ( 766.4474001241216001, -331.0999726633342561, -307.3154664389482491 ) ) ;
#29105 = CARTESIAN_POINT ( 'NONE',  ( 811.0346526505617248, -278.6346026584196807, 323.0537975583478101 ) ) ;
#29106 = CARTESIAN_POINT ( 'NONE',  ( 749.8865473780648472, 3.467130982857797417, 322.1177392798429082 ) ) ;
#29107 = CARTESIAN_POINT ( 'NONE',  ( 779.4763451958990572, -176.7363362996983369, -365.0264073115438919 ) ) ;
#29108 = CARTESIAN_POINT ( 'NONE',  ( 805.1927285166397041, -184.8164208402380950, -341.8018195045277707 ) ) ;
#29109 = CARTESIAN_POINT ( 'NONE',  ( 800.2193346964446619, -378.9982390220557136, -355.1360043628816925 ) ) ;
#29110 = ORIENTED_EDGE ( 'NONE', *, *, #30033, .T. ) ;
#29111 = ORIENTED_EDGE ( 'NONE', *, *, #1776, .F. ) ;
#29112 = CARTESIAN_POINT ( 'NONE',  ( 796.9462024416508257, -324.4527844766013231, 308.9653473494370246 ) ) ;
#29113 = CIRCLE ( 'NONE', #11406, 19.99999999999990763 ) ;
#29114 = DIRECTION ( 'NONE',  ( 0.000000000000000000, -1.000000000000000000, 0.000000000000000000 ) ) ;
#29115 = CARTESIAN_POINT ( 'NONE',  ( 805.2837595273609850, -218.7363362996982232, 340.5290396650784714 ) ) ;
#29116 = DIRECTION ( 'NONE',  ( 1.000000000000000000, 0.000000000000000000, 0.000000000000000000 ) ) ;
#29117 = VECTOR ( 'NONE', #29024, 1000.000000000000000 ) ;
#29118 = CARTESIAN_POINT ( 'NONE',  ( 775.8780910478218402, -153.2817908451529831, 364.9511171171680530 ) ) ;
#29119 = CARTESIAN_POINT ( 'NONE',  ( 757.8323909638827445, -50.63460265842036989, 352.1044303154654358 ) ) ;
#29120 = ORIENTED_EDGE ( 'NONE', *, *, #27209, .F. ) ;
#29121 = CARTESIAN_POINT ( 'NONE',  ( 786.2694204179717872, -405.2817908451522158, -305.1769319972829067 ) ) ;
#29122 = CARTESIAN_POINT ( 'NONE',  ( 800.9747183278959710, -12.99823902205686821, -311.9810565676471583 ) ) ;
#29123 = CARTESIAN_POINT ( 'NONE',  ( 750.9282345327678740, -280.9181544815162965, 319.8311093483690115 ) ) ;
#29124 = CARTESIAN_POINT ( 'NONE',  ( 794.1144889064781864, -226.1692326535051052, 360.9840315886528401 ) ) ;
#29125 = CARTESIAN_POINT ( 'NONE',  ( 802.1676090361156639, -374.6346026584192828, -327.8955696845344505 ) ) ;
#29126 = CARTESIAN_POINT ( 'NONE',  ( 778.2165204200184689, 1.183579159761269040, 364.9363028652563230 ) ) ;
#29127 = CARTESIAN_POINT ( 'NONE',  ( 779.4763451958990572, -248.7363362996981380, -365.0264073115438919 ) ) ;
#29128 = CLOSED_SHELL ( 'NONE', ( #21034, #22096, #33971, #20518, #17054, #14871, #19086, #43542, #11670, #4089, #21250, #39277, #3213, #26975 ) ) ;
#29129 = CARTESIAN_POINT ( 'NONE',  ( 814.9108240113580450, -40.27096629478405987, 337.5031285880265273 ) ) ;
#29130 = CARTESIAN_POINT ( 'NONE',  ( 763.0537975583475827, -96.45278447660203369, 371.0346526505627480 ) ) ;
#29131 = CARTESIAN_POINT ( 'NONE',  ( 701.1634899080286232, 259.9999999999999432, -199.9999999999990337 ) ) ;
#29132 = VECTOR ( 'NONE', #31165, 1000.000000000000000 ) ;
#29133 = CARTESIAN_POINT ( 'NONE',  ( 187.1337867209877857, 62.79977829742938411, -207.3621835540872951 ) ) ;
#29134 = AXIS2_PLACEMENT_3D ( 'NONE', #33111, #1448, #15549 ) ;
#29135 = CARTESIAN_POINT ( 'NONE',  ( 744.6391490659812007, -374.7363362996978253, 338.7502325331110455 ) ) ;
#29136 = DIRECTION ( 'NONE',  ( 1.880165489482579047E-16, 1.000000000000000000, -0.000000000000000000 ) ) ;
#29137 = CARTESIAN_POINT ( 'NONE',  ( 772.5602148656447525, -345.7255117493285184, 305.7998596910095443 ) ) ;
#29138 = ADVANCED_FACE ( 'NONE', ( #25144 ), #36458, .F. ) ;
#29139 = CARTESIAN_POINT ( 'NONE',  ( 774.6858677611749044, -321.7255117493286320, -315.5713283507209894 ) ) ;
#29140 = DIRECTION ( 'NONE',  ( -0.000000000000000000, 1.000000000000000000, -0.000000000000000000 ) ) ;
#29141 = CARTESIAN_POINT ( 'NONE',  ( 755.0636971347428243, -412.2709662947829088, 341.7834795799807353 ) ) ;
#29142 = CARTESIAN_POINT ( 'NONE',  ( 769.0155153010367712, -202.3726999360618777, 362.7791456095907279 ) ) ;
#29143 = CARTESIAN_POINT ( 'NONE',  ( 771.3260364891663130, -67.64542720878958448, -306.0683387631859773 ) ) ;
#29144 = CARTESIAN_POINT ( 'NONE',  ( 801.3366627262608972, -104.5328690171418913, -353.0897708529566899 ) ) ;
#29145 = CARTESIAN_POINT ( 'NONE',  ( 756.1443688327750579, -93.62377810805098477, 314.3581564841659315 ) ) ;
#29146 = CARTESIAN_POINT ( 'NONE',  ( 759.9864689768902508, -434.0891481129646081, 354.9819416627836404 ) ) ;
#29147 = CIRCLE ( 'NONE', #32071, 2.749999999999919176 ) ;
#29148 = CARTESIAN_POINT ( 'NONE',  ( 791.9812246680005501, -44.63460265842040542, -361.9419747391813189 ) ) ;
#29150 = ORIENTED_EDGE ( 'NONE', *, *, #3233, .F. ) ;
#29149 = CARTESIAN_POINT ( 'NONE',  ( 802.7791456095903868, -148.7146871989598935, -329.0155153010375102 ) ) ;
#29151 = CARTESIAN_POINT ( 'NONE',  ( 767.8955696845333705, -96.45278447660203369, -362.1676090361162323 ) ) ;
#29152 = AXIS2_PLACEMENT_3D ( 'NONE', #26505, #42985, #11350 ) ;
#29153 = CARTESIAN_POINT ( 'NONE',  ( 801.3366627262608972, -416.5328690171409107, -353.0897708529566899 ) ) ;
#29155 = CARTESIAN_POINT ( 'NONE',  ( 754.8072714833583632, -268.8164208402378677, 338.1981804954721156 ) ) ;
#29154 = CARTESIAN_POINT ( 'NONE',  ( 771.2633955100217236, -263.9073299311469327, 363.4237431249939618 ) ) ;
#29156 = CARTESIAN_POINT ( 'NONE',  ( 919.9999999999993179, 154.9999999999998863, 339.9999999999999432 ) ) ;
#29157 = VERTEX_POINT ( 'NONE', #7854 ) ;
#29158 = CARTESIAN_POINT ( 'NONE',  ( 803.2186876482843445, 16.01258552831230375, 350.0220218866286928 ) ) ;
#29159 = EDGE_LOOP ( 'NONE', ( #17650, #17212, #7013, #28725 ) ) ;
#29160 = CARTESIAN_POINT ( 'NONE',  ( 796.7737145352015204, -188.6346026584199365, 370.7187646348536987 ) ) ;
#29161 = VECTOR ( 'NONE', #29140, 1000.000000000000000 ) ;
#29162 = CARTESIAN_POINT ( 'NONE',  ( 804.8461984189677878, -266.1908817542435486, 336.9566956441385628 ) ) ;
#29163 = ORIENTED_EDGE ( 'NONE', *, *, #40496, .F. ) ;
#29164 = CARTESIAN_POINT ( 'NONE',  ( 793.9708237608222134, -70.91815448151683654, -319.2295555964448681 ) ) ;
#29165 = CARTESIAN_POINT ( 'NONE',  ( 749.8865473780648472, -212.5328690171415076, 322.1177392798429082 ) ) ;
#29166 = CARTESIAN_POINT ( 'NONE',  ( 768.0187753319979720, -272.6346026584196807, -318.0580252608186242 ) ) ;
#29167 = VECTOR ( 'NONE', #35536, 1000.000000000000000 ) ;
#29168 = ORIENTED_EDGE ( 'NONE', *, *, #29862, .T. ) ;
#29169 = CARTESIAN_POINT ( 'NONE',  ( 801.9419747391806368, -402.4527844766010389, -351.9812246680014027 ) ) ;
#29170 = CARTESIAN_POINT ( 'NONE',  ( 794.9819416627830151, -60.99823902205671544, -319.9864689768909898 ) ) ;
#29171 = VECTOR ( 'NONE', #45259, 1000.000000000000000 ) ;
#29172 = CARTESIAN_POINT ( 'NONE',  ( 784.0799538623451781, -275.8055962898685038, 364.6971507214555572 ) ) ;
#29173 = DIRECTION ( 'NONE',  ( 0.000000000000000000, 0.000000000000000000, 1.000000000000000000 ) ) ;
#29174 = CARTESIAN_POINT ( 'NONE',  ( -468.8365100919714337, 260.0000000000001705, -197.2499999999910187 ) ) ;
#29175 = CARTESIAN_POINT ( 'NONE',  ( 746.4236121716829757, -15.82724539060794200, -328.8385539511384650 ) ) ;
#29176 = CARTESIAN_POINT ( 'NONE',  ( 779.9999999999992042, 16.45630643248849267, -350.0000000000000000 ) ) ;
#29177 = VERTEX_POINT ( 'NONE', #29327 ) ;
#29178 = CARTESIAN_POINT ( 'NONE',  ( 814.2805881961230625, -313.6454272087888171, -331.2368401574024119 ) ) ;
#29179 = AXIS2_PLACEMENT_3D ( 'NONE', #33060, #43876, #39986 ) ;
#29180 = CARTESIAN_POINT ( 'NONE',  ( 809.0717654672305343, -172.9181544815165239, 360.1688906516309885 ) ) ;
#29181 = VECTOR ( 'NONE', #36404, 1000.000000000000000 ) ;
#29183 = CARTESIAN_POINT ( 'NONE',  ( 774.6858677611749044, -273.7255117493288026, -315.5713283507209894 ) ) ;
#29182 = DIRECTION ( 'NONE',  ( 1.000000000000000000, 0.000000000000000000, 0.000000000000000000 ) ) ;
#29184 = CARTESIAN_POINT ( 'NONE',  ( 779.9999999999992042, -452.9681489794448339, 339.9999999999999432 ) ) ;
#29185 = CARTESIAN_POINT ( 'NONE',  ( 802.9823548866075953, -145.0999726633347677, -330.0799878456151077 ) ) ;
#29186 = VECTOR ( 'NONE', #3590, 1000.000000000000000 ) ;
#29187 = EDGE_CURVE ( 'NONE', #1032, #8959, #8292, .T. ) ;
#29188 = CARTESIAN_POINT ( 'NONE',  ( 815.2698199232961542, -16.81642084023866701, 342.5225473063383106 ) ) ;
#29189 = AXIS2_PLACEMENT_3D ( 'NONE', #13340, #41982, #41750 ) ;
#29190 = DIRECTION ( 'NONE',  ( 1.880165489482579047E-16, 1.000000000000000000, -0.000000000000000000 ) ) ;
#29191 = CARTESIAN_POINT ( 'NONE',  ( 767.7687537140311633, -335.9073299311468190, -372.7932403749916830 ) ) ;
#29192 = DIRECTION ( 'NONE',  ( 0.000000000000000000, 0.000000000000000000, 1.000000000000000000 ) ) ;
#29193 = CARTESIAN_POINT ( 'NONE',  ( 756.5762568750052424, -3.180057203875080063, 348.7366044899774238 ) ) ;
#29194 = CARTESIAN_POINT ( 'NONE',  ( 813.5763878283155464, -291.8272453906071746, 351.1614460488615350 ) ) ;
#29195 = CARTESIAN_POINT ( 'NONE',  ( 781.2497674668890113, -228.3510508353232922, -375.3608509340180603 ) ) ;
#29196 = CARTESIAN_POINT ( 'NONE',  ( 800.9747183278959710, -228.9982390220561683, 311.9810565676471583 ) ) ;
#29197 = CARTESIAN_POINT ( 'NONE',  ( 754.9967657858570647, -1.543693567511449150, -365.0032342141425374 ) ) ;
#29198 = EDGE_CURVE ( 'NONE', #39517, #6318, #12846, .T. ) ;
#29199 = EDGE_CURVE ( 'NONE', #10985, #40969, #14782, .T. ) ;
#29200 = DIRECTION ( 'NONE',  ( 0.000000000000000000, -0.6755902076156505842, -0.7372773368101328550 ) ) ;
#29201 = ORIENTED_EDGE ( 'NONE', *, *, #10884, .F. ) ;
#29202 = CARTESIAN_POINT ( 'NONE',  ( 757.8323909638827445, -314.6346026584194533, 352.1044303154654358 ) ) ;
#29203 = VECTOR ( 'NONE', #13727, 1000.000000000000000 ) ;
#29204 = CARTESIAN_POINT ( 'NONE',  ( 799.2566176426618085, -96.00906357242585898, 324.0069404352559559 ) ) ;
#29205 = CARTESIAN_POINT ( 'NONE',  ( 786.6156483768007774, -25.44195992623301450, -315.5913626894246136 ) ) ;
#29206 = CIRCLE ( 'NONE', #30646, 19.99999999999990763 ) ;
#29207 = CARTESIAN_POINT ( 'NONE',  ( 789.9999999999992042, 205.0000000000000568, -350.0000000000000000 ) ) ;
#29208 = FACE_OUTER_BOUND ( 'NONE', #38072, .T. ) ;
#29210 = CARTESIAN_POINT ( 'NONE',  ( 767.8955696845333705, -360.4527844766010958, 362.1676090361162323 ) ) ;
#29209 = CARTESIAN_POINT ( 'NONE',  ( 786.6156483768007774, -145.4419599262326699, 315.5913626894246136 ) ) ;
#29211 = EDGE_LOOP ( 'NONE', ( #30936, #31834, #43506, #7683 ) ) ;
#29212 = CARTESIAN_POINT ( 'NONE',  ( 756.1348686366196716, -281.2601417444139997, -347.5531968255698416 ) ) ;
#29213 = CARTESIAN_POINT ( 'NONE',  ( 781.7834795799800531, -154.8164208402382371, 315.0636971347436202 ) ) ;
#29214 = UNCERTAINTY_MEASURE_WITH_UNIT (LENGTH_MEASURE( 1.000000000000000082E-05 ), #30081, 'distance_accuracy_value', 'NONE');
#29215 = CARTESIAN_POINT ( 'NONE',  ( 812.6845335610512393, -319.9874144716866340, -353.5525998758768651 ) ) ;
#29216 = CARTESIAN_POINT ( 'NONE',  ( 809.9999999999993179, -512.9681489794448908, -339.9999999999999432 ) ) ;
#29217 = CARTESIAN_POINT ( 'NONE',  ( 788.7631598425961101, -433.4419599262316183, 305.7194118038759143 ) ) ;
#29218 = ADVANCED_FACE ( 'NONE', ( #43172 ), #8524, .F. ) ;
#29219 = EDGE_LOOP ( 'NONE', ( #252, #19722 ) ) ;
#29220 = CARTESIAN_POINT ( 'NONE',  ( 767.8955696845333705, -336.4527844766012095, 362.1676090361162323 ) ) ;
#29221 = VECTOR ( 'NONE', #14440, 1000.000000000000000 ) ;
#29222 = EDGE_CURVE ( 'NONE', #40010, #33295, #33518, .T. ) ;
#29223 = CARTESIAN_POINT ( 'NONE',  ( 756.7813123517142913, -91.98741447168737295, -329.9779781133712504 ) ) ;
#29224 = VERTEX_POINT ( 'NONE', #25380 ) ;
#29225 = CARTESIAN_POINT ( 'NONE',  ( 792.1044303154645831, -444.4527844766009821, 317.8323909638837677 ) ) ;
#29226 = AXIS2_PLACEMENT_3D ( 'NONE', #14465, #28998, #18162 ) ;
#29227 = CARTESIAN_POINT ( 'NONE',  ( 814.2001403089898304, -185.3618753856926844, -347.4397851343538264 ) ) ;
#29228 = ADVANCED_FACE ( 'NONE', ( #32778 ), #4380, .T. ) ;
#29229 = ORIENTED_EDGE ( 'NONE', *, *, #12516, .F. ) ;
#29230 = CARTESIAN_POINT ( 'NONE',  ( 803.6646147819162707, -137.9073299311473875, -348.8264449731211130 ) ) ;
#29231 = VERTEX_POINT ( 'NONE', #4594 ) ;
#29232 = CARTESIAN_POINT ( 'NONE',  ( 802.9823548866075953, -409.0999726633340288, -330.0799878456151077 ) ) ;
#29233 = CARTESIAN_POINT ( 'NONE',  ( 774.6312213355099630, 0.6381246143067236254, 364.6798772138717482 ) ) ;
#29234 = CARTESIAN_POINT ( 'NONE',  ( 763.2154366446407039, -165.6237781080507716, 321.4292242960311228 ) ) ;
#29237 = CARTESIAN_POINT ( 'NONE',  ( 793.4146539503750546, -409.9874144716863498, 307.6481478633938877 ) ) ;
#29236 = CARTESIAN_POINT ( 'NONE',  ( 779.9999999999992042, 126.4563064324884465, -309.9999999999998863 ) ) ;
#29235 = CARTESIAN_POINT ( 'NONE',  ( -190.7583438952259485, 394.6698570112193920, -244.9999999999999716 ) ) ;
#29238 = EDGE_LOOP ( 'NONE', ( #33685, #9186, #28177, #7341 ) ) ;
#29239 = CARTESIAN_POINT ( 'NONE',  ( 799.2566176426618085, -408.0090635724249069, -324.0069404352559559 ) ) ;
#29240 = CARTESIAN_POINT ( 'NONE',  ( -28.63011601220122415, -512.9681489794448908, -352.0000000000000000 ) ) ;
#29241 = CARTESIAN_POINT ( 'NONE',  ( 766.4474001241216001, -187.0999726633346825, -307.3154664389482491 ) ) ;
#29242 = CARTESIAN_POINT ( 'NONE',  ( 764.1737431748507561, -58.37269993606236085, 371.6461892240376415 ) ) ;
#29243 = AXIS2_PLACEMENT_3D ( 'NONE', #31030, #23627, #31259 ) ;
#29245 = DIRECTION ( 'NONE',  ( 1.880165489482579047E-16, 1.000000000000000000, 0.000000000000000000 ) ) ;
#29244 = CARTESIAN_POINT ( 'NONE',  ( 571.1634899080285095, 258.0939999999999372, -193.8809999999981528 ) ) ;
#29246 = EDGE_CURVE ( 'NONE', #33818, #19659, #18470, .T. ) ;
#29247 = CARTESIAN_POINT ( 'NONE',  ( 779.4709603349208464, -336.3510508353228943, -314.7162404726379918 ) ) ;
#29248 = CARTESIAN_POINT ( 'NONE',  ( 799.9999999999993179, -365.3551492539851893, -18.13243251470705886 ) ) ;
#29249 = CARTESIAN_POINT ( 'NONE',  ( 749.5768839229115201, -180.5545181178801499, -358.0661480581553064 ) ) ;
#29250 = DIRECTION ( 'NONE',  ( 0.000000000000000000, 0.000000000000000000, 1.000000000000000000 ) ) ;
#29251 = FACE_BOUND ( 'NONE', #9616, .T. ) ;
#29252 = AXIS2_PLACEMENT_3D ( 'NONE', #822, #7535, #39872 ) ;
#29253 = CARTESIAN_POINT ( 'NONE',  ( 804.6971507214547046, -387.2817908451522726, 344.0799538623459739 ) ) ;
#29254 = EDGE_CURVE ( 'NONE', #30100, #9272, #323, .T. ) ;
#29255 = CARTESIAN_POINT ( 'NONE',  ( 758.8095938919644823, -248.0891481129651766, -311.6929314249762797 ) ) ;
#29256 = CARTESIAN_POINT ( 'NONE',  ( 311.1634899080286232, 260.0000000000000000, -199.9999999999963336 ) ) ;
#29257 = CARTESIAN_POINT ( 'NONE',  ( 762.1405469898971887, -1.543693567511449150, -357.8594530101015607 ) ) ;
#29258 = CARTESIAN_POINT ( 'NONE',  ( 746.4236121716829757, -183.8272453906074020, 328.8385539511384650 ) ) ;
#29259 = CARTESIAN_POINT ( 'NONE',  ( 751.2241431872005251, -136.1692326535053894, -359.9636004259367610 ) ) ;
#29260 = CARTESIAN_POINT ( 'NONE',  ( 812.7932403749906598, -135.1800572038746679, 327.7687537140311633 ) ) ;
#29261 = CARTESIAN_POINT ( 'NONE',  ( 745.0891759886404770, -364.2709662947830793, -342.4968714119734159 ) ) ;
#29262 = EDGE_CURVE ( 'NONE', #40029, #25691, #42712, .T. ) ;
#29263 = DIRECTION ( 'NONE',  ( 1.000000000000000000, 0.000000000000000000, 0.000000000000000000 ) ) ;
#29264 = DIRECTION ( 'NONE',  ( -0.000000000000000000, 1.000000000000000000, -0.000000000000000000 ) ) ;
#29265 = CARTESIAN_POINT ( 'NONE',  ( 804.9363028652555840, -232.2709662947834488, 338.2165204200192079 ) ) ;
#29266 = CARTESIAN_POINT ( 'NONE',  ( 759.0159684113467620, -16.91815448151702839, 325.8855110935213020 ) ) ;
#29267 = CARTESIAN_POINT ( 'NONE',  ( 795.6651683502461765, -418.7146871989590409, -371.3240766477733814 ) ) ;
#29268 = B_SPLINE_CURVE_WITH_KNOTS ( 'NONE', 3,
 ( #6201, #13154, #27234, #5758 ),
 .UNSPECIFIED., .F., .F.,
 ( 4, 4 ),
 ( 0.03659475354221209537, 0.03709560045499031566 ),
 .UNSPECIFIED. ) ;
#29269 = CARTESIAN_POINT ( 'NONE',  ( 777.4774526936600978, -442.2709662947826814, -304.7301800767027657 ) ) ;
#29270 = DIRECTION ( 'NONE',  ( 0.000000000000000000, 0.000000000000000000, 1.000000000000000000 ) ) ;
#29271 = CARTESIAN_POINT ( 'NONE',  ( 783.7566961878529810, -24.89650538077847486, 305.1792804349288417 ) ) ;
#29272 = ORIENTED_EDGE ( 'NONE', *, *, #13131, .T. ) ;
#29273 = CARTESIAN_POINT ( 'NONE',  ( 794.1144889064781864, -202.1692326535051905, -360.9840315886528401 ) ) ;
#29274 = CARTESIAN_POINT ( 'NONE',  ( 768.0187753319979720, -8.634602658420517329, 318.0580252608186242 ) ) ;
#29275 = CARTESIAN_POINT ( 'NONE',  ( 773.7943932421234194, -239.8055962898687028, -305.5313806188329409 ) ) ;
#29276 = CARTESIAN_POINT ( 'NONE',  ( 745.1769319972822814, -353.8055962898683333, 346.2694204179732083 ) ) ;
#29277 = CARTESIAN_POINT ( 'NONE',  ( 774.6312213355098493, -167.3618753856927412, 364.6798772138717482 ) ) ;
#29278 = ORIENTED_EDGE ( 'NONE', *, *, #10363, .F. ) ;
#29279 = CARTESIAN_POINT ( 'NONE',  ( 756.1443688327750579, -429.6237781080499190, 314.3581564841659315 ) ) ;
#29280 = AXIS2_PLACEMENT_3D ( 'NONE', #39671, #11024, #39204 ) ;
#29281 = CARTESIAN_POINT ( 'NONE',  ( 788.8264449731200330, -141.1800572038746395, -363.6646147819171233 ) ) ;
#29282 = CARTESIAN_POINT ( 'NONE',  ( 805.1927285166397041, -352.8164208402374129, 341.8018195045277707 ) ) ;
#29283 = VECTOR ( 'NONE', #21331, 1000.000000000000000 ) ;
#29284 = CARTESIAN_POINT ( 'NONE',  ( 745.7998596910086917, -29.36187538569318178, -332.5602148656461168 ) ) ;
#29285 = AXIS2_PLACEMENT_3D ( 'NONE', #35759, #4138, #32306 ) ;
#29286 = ORIENTED_EDGE ( 'NONE', *, *, #29752, .F. ) ;
#29287 = CARTESIAN_POINT ( 'NONE',  ( 748.6759233522253680, -448.3726999360611103, -324.3348316497537098 ) ) ;
#29288 = CIRCLE ( 'NONE', #27786, 8.025000000000003908 ) ;
#29289 = ORIENTED_EDGE ( 'NONE', *, *, #31416, .T. ) ;
#29290 = CARTESIAN_POINT ( 'NONE',  ( 766.0291762391763086, -322.9181544815161260, -360.7704444035551319 ) ) ;
#29291 = CONTEXT_DEPENDENT_SHAPE_REPRESENTATION ( #39394, #17029 ) ;
#29293 = CARTESIAN_POINT ( 'NONE',  ( 755.8894580844503253, -375.8272453906069472, 332.3691319403863531 ) ) ;
#29292 = CARTESIAN_POINT ( 'NONE',  ( 757.8323909638827445, -50.63460265842036989, 352.1044303154654358 ) ) ;
#29294 = CARTESIAN_POINT ( 'NONE',  ( 762.1405469898971887, -289.5436935675103882, -357.8594530101015607 ) ) ;
#29295 = CIRCLE ( 'NONE', #24856, 9.999999999999980460 ) ;
#29297 = CARTESIAN_POINT ( 'NONE',  ( 768.8385539511368734, -287.2601417444140566, 306.4236121716840557 ) ) ;
#29296 = CARTESIAN_POINT ( 'NONE',  ( 763.0537975583476964, -408.4527844766009821, 371.0346526505628617 ) ) ;
#29298 = CARTESIAN_POINT ( 'NONE',  ( 813.9316612368132837, -103.4419599262327836, 348.6739635108323228 ) ) ;
#29299 = CARTESIAN_POINT ( 'NONE',  ( 796.1575198192839480, -294.0090635724253048, -359.4546378042384163 ) ) ;
#29300 = CARTESIAN_POINT ( 'NONE',  ( 754.8072714833581358, -292.8164208402376971, -338.1981804954720587 ) ) ;
#29301 = DIRECTION ( 'NONE',  ( -1.880165489482579047E-16, -1.000000000000000000, 0.000000000000000000 ) ) ;
#29302 = CARTESIAN_POINT ( 'NONE',  ( 759.9864689768902508, -170.0891481129654608, -354.9819416627836404 ) ) ;
#29303 = DIRECTION ( 'NONE',  ( -1.000000000000000000, -0.000000000000000000, -0.000000000000000000 ) ) ;
#29304 = CARTESIAN_POINT ( 'NONE',  ( 746.8695393053150156, -413.9073299311465348, 327.6429770376306010 ) ) ;
#29306 = CARTESIAN_POINT ( 'NONE',  ( -769.9999999999992042, 205.0000000000000568, -339.9999999999999432 ) ) ;
#29305 = CARTESIAN_POINT ( 'NONE',  ( 769.9999999999992042, 205.0000000000000568, -319.9999999999999432 ) ) ;
#29307 = EDGE_CURVE ( 'NONE', #21916, #35390, #8082, .T. ) ;
#29308 = CARTESIAN_POINT ( 'NONE',  ( 781.2370466360911223, -92.73633629969860692, -304.9990715423533629 ) ) ;
#29309 = CYLINDRICAL_SURFACE ( 'NONE', #19694, 10.00000000000000888 ) ;
#29310 = CARTESIAN_POINT ( 'NONE',  ( 879.9999999999992042, 249.9999999999998295, -199.9999999999999716 ) ) ;
#29311 = CARTESIAN_POINT ( 'NONE',  ( 761.4292242960306112, -305.4636090269706870, 323.2154366446414429 ) ) ;
#29312 = CARTESIAN_POINT ( 'NONE',  ( 755.3201227861273992, -147.7255117493291152, 345.3687786644892981 ) ) ;
#29313 = ORIENTED_EDGE ( 'NONE', *, *, #8380, .T. ) ;
#29314 = CARTESIAN_POINT ( 'NONE',  ( 746.8695393053151292, -149.9073299311473875, -327.6429770376306578 ) ) ;
#29315 = CARTESIAN_POINT ( 'NONE',  ( 770.0799878456142551, -325.9874144716865771, 362.9823548866085616 ) ) ;
#29316 = DIRECTION ( 'NONE',  ( 1.000000000000000000, 0.000000000000000000, 0.000000000000000000 ) ) ;
#29317 = CARTESIAN_POINT ( 'NONE',  ( 749.5768839229115201, -60.55451811788051941, 358.0661480581553064 ) ) ;
#29319 = VECTOR ( 'NONE', #16567, 1000.000000000000000 ) ;
#29318 = CARTESIAN_POINT ( 'NONE',  ( 792.3570229623688874, -285.1800572038740711, -373.1304606946836202 ) ) ;
#29320 = ADVANCED_FACE ( 'NONE', ( #14556 ), #36233, .T. ) ;
#29321 = CARTESIAN_POINT ( 'NONE',  ( 772.5602148656447525, -201.7255117493290015, 305.7998596910095443 ) ) ;
#29322 = CARTESIAN_POINT ( 'NONE',  ( 759.9864689768902508, -122.0891481129656171, 354.9819416627836404 ) ) ;
#29323 = SURFACE_STYLE_USAGE ( .BOTH. , #1121 ) ;
#29324 = CARTESIAN_POINT ( 'NONE',  ( 778.7502325331095108, -312.3510508353230080, -304.6391490659818828 ) ) ;
#29325 = CARTESIAN_POINT ( 'NONE',  ( 802.5472867521000353, -4.372699936062523385, 350.8726784830461156 ) ) ;
#29326 = CARTESIAN_POINT ( 'NONE',  ( 745.7998596910086917, -365.3618753856920875, -332.5602148656461168 ) ) ;
#29327 = CARTESIAN_POINT ( 'NONE',  ( 999.9999999999992042, 478.9999999999999432, 359.0000000000000000 ) ) ;
#29328 = CARTESIAN_POINT ( 'NONE',  ( 758.6633372737375112, -380.5328690171409676, 326.9102291470432533 ) ) ;
#29329 = ORIENTED_EDGE ( 'NONE', *, *, #28285, .T. ) ;
#29330 = CARTESIAN_POINT ( 'NONE',  ( 771.2633955100217236, -407.9073299311465348, -363.4237431249939618 ) ) ;
#29331 = AXIS2_PLACEMENT_3D ( 'NONE', #22285, #25763, #36381 ) ;
#29332 = CARTESIAN_POINT ( 'NONE',  ( 757.8323909638827445, -218.6346026584197944, -352.1044303154654358 ) ) ;
#29333 = CARTESIAN_POINT ( 'NONE',  ( 800.1688906516307043, -82.16923265350558836, -369.0717654672308186 ) ) ;
#29334 = DIRECTION ( 'NONE',  ( 0.000000000000000000, 0.000000000000000000, 1.000000000000000000 ) ) ;
#29335 = CARTESIAN_POINT ( 'NONE',  ( 815.0009284576459549, -246.3510508353232638, 338.7629533639073429 ) ) ;
#29336 = CARTESIAN_POINT ( 'NONE',  ( 785.3687786644885591, -59.36187538569307520, 315.3201227861280813 ) ) ;
#29337 = CARTESIAN_POINT ( 'NONE',  ( 794.1144889064781864, -226.1692326535051052, -360.9840315886528401 ) ) ;
#29338 = CARTESIAN_POINT ( 'NONE',  ( 762.1405469898971887, -217.5436935675107293, 357.8594530101015607 ) ) ;
#29339 = CARTESIAN_POINT ( 'NONE',  ( 752.4576283171824116, -69.07832356259653750, -317.7880784355627952 ) ) ;
#29340 = CARTESIAN_POINT ( 'NONE',  ( 806.2451613922657998, -452.9681489794450613, -344.7413990863497020 ) ) ;
#29341 = EDGE_LOOP ( 'NONE', ( #32895, #7570, #16650, #34982 ) ) ;
#29342 = VERTEX_POINT ( 'NONE', #15238 ) ;
#29343 = CARTESIAN_POINT ( 'NONE',  ( 768.9521613784389729, -345.8272453906069472, -373.2346286133773106 ) ) ;
#29344 = CARTESIAN_POINT ( 'NONE',  ( 777.4774526936600978, -298.2709662947831930, 304.7301800767028226 ) ) ;
#29345 = CARTESIAN_POINT ( 'NONE',  ( 800.1688906516307043, -34.16923265350572336, 369.0717654672308186 ) ) ;
#29346 = CARTESIAN_POINT ( 'NONE',  ( 769.9779781133707957, -187.0999726633346825, -316.7813123517150871 ) ) ;
#29347 = CARTESIAN_POINT ( 'NONE',  ( 774.6312213355099630, -167.3618753856927412, -364.6798772138717482 ) ) ;
#29348 = CARTESIAN_POINT ( 'NONE',  ( 792.1044303154646968, -372.4527844766012095, -317.8323909638837677 ) ) ;
#29349 = ORIENTED_EDGE ( 'NONE', *, *, #7658, .T. ) ;
#29350 = CARTESIAN_POINT ( 'NONE',  ( 775.9200461376533440, 24.19440371013046231, -315.3028492785443291 ) ) ;
#29351 = EDGE_LOOP ( 'NONE', ( #39002, #35405, #12879, #30845, #37954, #34340 ) ) ;
#29352 = CARTESIAN_POINT ( 'NONE',  ( 763.2262854647970016, -320.6346026584195670, 309.2812353651462445 ) ) ;
#29353 = CARTESIAN_POINT ( 'NONE',  ( -728.8365100919714905, 260.0000000000001705, -199.9999999999890861 ) ) ;
#29354 = CARTESIAN_POINT ( 'NONE',  ( 799.4546378042377910, -369.0783235625956422, 356.1575198192848006 ) ) ;
#29355 = DIRECTION ( 'NONE',  ( 0.000000000000000000, 0.000000000000000000, -1.000000000000000000 ) ) ;
#29356 = CARTESIAN_POINT ( 'NONE',  ( 799.2566176426618085, -192.0090635724255606, 324.0069404352559559 ) ) ;
#29357 = CARTESIAN_POINT ( 'NONE',  ( 774.6858677611749044, -57.72551174932945628, 315.5713283507209894 ) ) ;
#29358 = EDGE_LOOP ( 'NONE', ( #38847, #23172, #26740, #20935 ) ) ;
#29359 = CARTESIAN_POINT ( 'NONE',  ( 745.1792804349281596, -422.1908817542430370, -343.7566961878542884 ) ) ;
#29360 = EDGE_CURVE ( 'NONE', #10119, #40963, #4823, .T. ) ;
#29361 = EDGE_CURVE ( 'NONE', #42107, #42944, #1358, .T. ) ;
#29362 = CARTESIAN_POINT ( 'NONE',  ( 801.1904061080338124, -20.08914811296593328, -368.3070685750236066 ) ) ;
#29363 = CARTESIAN_POINT ( 'NONE',  ( 789.9200121543843807, -217.9874144716870035, 317.0176451133914384 ) ) ;
#29364 = CARTESIAN_POINT ( 'NONE',  ( 771.2633955100217236, -407.9073299311465348, -363.4237431249939618 ) ) ;
#29365 = CARTESIAN_POINT ( 'NONE',  ( 794.9819416627830151, -12.99823902205686821, -319.9864689768909898 ) ) ;
#29366 = CARTESIAN_POINT ( 'NONE',  ( 759.7806653035534055, -6.998239022056885972, 324.8639956371180801 ) ) ;
#29367 = SURFACE_SIDE_STYLE ('',( #39545 ) ) ;
#29368 = CARTESIAN_POINT ( 'NONE',  ( 801.5560724626406000, -240.5545181178798941, -326.7756240680316182 ) ) ;
#29369 = CARTESIAN_POINT ( 'NONE',  ( 748.9653473494363425, -50.63460265842036989, 356.9462024416521331 ) ) ;
#29370 = CARTESIAN_POINT ( 'NONE',  ( 787.4397851343537695, -93.72551174932934259, 374.2001403089903988 ) ) ;
#29371 = DIRECTION ( 'NONE',  ( -1.000000000000000000, -0.000000000000000000, 0.000000000000000000 ) ) ;
#29372 = CARTESIAN_POINT ( 'NONE',  ( 767.9999999999992042, 240.0000000000000853, 360.0000000000000000 ) ) ;
#29373 = CARTESIAN_POINT ( 'NONE',  ( 783.7953271457878373, -392.1908817542432075, 375.1787889125761239 ) ) ;
#29374 = DIRECTION ( 'NONE',  ( 0.000000000000000000, 0.000000000000000000, 1.000000000000000000 ) ) ;
#29375 = CARTESIAN_POINT ( 'NONE',  ( 763.2262854647970016, -368.6346026584193964, 309.2812353651462445 ) ) ;
#29376 = CARTESIAN_POINT ( 'NONE',  ( 765.0180583372156207, -312.9982390220559409, -360.0135310231089534 ) ) ;
#29377 = CARTESIAN_POINT ( 'NONE',  ( 754.8983024940795303, 5.103494619221427442, 336.9254006560228163 ) ) ;
#29378 = CARTESIAN_POINT ( 'NONE',  ( 796.1575198192839480, -174.0090635724256742, 359.4546378042384163 ) ) ;
#29379 = CARTESIAN_POINT ( 'NONE',  ( 768.9521613784389729, -81.82724539060772884, -373.2346286133773106 ) ) ;
#29380 = CARTESIAN_POINT ( 'NONE',  ( 756.7813123517142913, -115.9874144716872877, -329.9779781133712504 ) ) ;
#29381 = CARTESIAN_POINT ( 'NONE',  ( 758.0141637701419768, -135.0783235625962959, 367.2620300519063790 ) ) ;
#29382 = CARTESIAN_POINT ( 'NONE',  ( 803.4237431249931660, -423.1800572038737300, 331.2633955100225194 ) ) ;
#29383 = AXIS2_PLACEMENT_3D ( 'NONE', #27885, #6413, #45204 ) ;
#29384 = CARTESIAN_POINT ( 'NONE',  ( 768.0187753319979720, -32.63460265842044095, -318.0580252608186242 ) ) ;
#29385 = CARTESIAN_POINT ( 'NONE',  ( 796.7845633553578182, -129.6237781080508853, -358.5707757039688204 ) ) ;
#29386 = CARTESIAN_POINT ( 'NONE',  ( 788.4001350590139054, -443.1233509495419298, -363.5803521658918385 ) ) ;
#29388 = CARTESIAN_POINT ( 'NONE',  ( 762.1405469898973024, -265.5436935675106156, 357.8594530101016176 ) ) ;
#29387 = CARTESIAN_POINT ( 'NONE',  ( 762.3223304703356007, -247.5436935675106724, 322.3223304703362828 ) ) ;
#29389 = DIRECTION ( 'NONE',  ( 0.000000000000000000, 0.000000000000000000, 1.000000000000000000 ) ) ;
#29390 = ORIENTED_EDGE ( 'NONE', *, *, #14505, .F. ) ;
#29391 = CARTESIAN_POINT ( 'NONE',  ( 793.2243759319678702, 21.46713098285774279, 318.4439275373583200 ) ) ;
#29392 = EDGE_LOOP ( 'NONE', ( #36406, #39224, #1102, #2489 ) ) ;
#29393 = SHAPE_REPRESENTATION_RELATIONSHIP ( 'NONE' , 'NONE' ,  #28884, #37568 ) ;
#29394 = CARTESIAN_POINT ( 'NONE',  ( 767.6429770376291799, -177.1800572038744974, 306.8695393053162093 ) ) ;
#29395 = CARTESIAN_POINT ( 'NONE',  ( 755.1538015810308480, -278.1908817542434917, 343.0433043558613804 ) ) ;
#29396 = ORIENTED_EDGE ( 'NONE', *, *, #20446, .F. ) ;
#29397 = CARTESIAN_POINT ( 'NONE',  ( 790.9844846989617508, -94.37269993606224716, -317.2208543904092721 ) ) ;
#29398 = CARTESIAN_POINT ( 'NONE',  ( 773.7943932421234194, -215.8055962898687881, 305.5313806188329409 ) ) ;
#29399 = CARTESIAN_POINT ( 'NONE',  ( 757.8323909638828582, -266.6346026584197375, -352.1044303154654358 ) ) ;
#29400 = EDGE_LOOP ( 'NONE', ( #31760, #4367 ) ) ;
#29401 = CARTESIAN_POINT ( 'NONE',  ( 781.8018195045266339, -406.2709662947829088, -365.1927285166406705 ) ) ;
#29402 = CARTESIAN_POINT ( 'NONE',  ( 805.1927285166397041, -40.81642084023859951, -341.8018195045277707 ) ) ;
#29403 = CARTESIAN_POINT ( 'NONE',  ( 802.7791456095903868, -268.7146871989595525, 329.0155153010375102 ) ) ;
#29404 = FACE_BOUND ( 'NONE', #28536, .T. ) ;
#29405 = CARTESIAN_POINT ( 'NONE',  ( 759.9999999999992042, 205.0000000000000568, 339.9999999999999432 ) ) ;
#29406 = CARTESIAN_POINT ( 'NONE',  ( 811.3240766477731540, -28.37269993606244967, -355.6651683502462902 ) ) ;
#29407 = CYLINDRICAL_SURFACE ( 'NONE', #26856, 20.00000000000001776 ) ;
#29408 = EDGE_LOOP ( 'NONE', ( #4807, #42314, #632, #40464 ) ) ;
#29409 = CARTESIAN_POINT ( 'NONE',  ( 783.7953271457878373, -296.1908817542434917, -375.1787889125761239 ) ) ;
#29410 = ADVANCED_FACE ( 'NONE', ( #43614, #2482, #19816 ), #29981, .T. ) ;
#29411 = CARTESIAN_POINT ( 'NONE',  ( 802.2119215644370342, -174.0090635724256742, 367.5423716828165084 ) ) ;
#29412 = VECTOR ( 'NONE', #30777, 1000.000000000000000 ) ;
#29414 = CARTESIAN_POINT ( 'NONE',  ( 758.0580252608178853, -294.4527844766013800, -328.0187753319985404 ) ) ;
#29413 = CARTESIAN_POINT ( 'NONE',  ( -858.8365100919713768, 260.0000000000002274, -208.0249999999880970 ) ) ;
#29415 = CARTESIAN_POINT ( 'NONE',  ( 759.9999999999992042, -512.9681489794448908, 309.9999999999998863 ) ) ;
#29416 = CARTESIAN_POINT ( 'NONE',  ( 804.1105419155481968, -147.8272453906075157, -347.6308680596136469 ) ) ;
#29417 = CARTESIAN_POINT ( 'NONE',  ( -879.9999999999992042, 430.0000000000002842, -320.0000000000000568 ) ) ;
#29418 = CARTESIAN_POINT ( 'NONE',  ( 782.5225473063383106, -358.2709662947830225, -375.2698199232970637 ) ) ;
#29419 = DIRECTION ( 'NONE',  ( -0.000000000000000000, 1.000000000000000000, -0.000000000000000000 ) ) ;
#29420 = CARTESIAN_POINT ( 'NONE',  ( 759.9864689768902508, -50.08914811296584446, 354.9819416627836404 ) ) ;
#29421 = CARTESIAN_POINT ( 'NONE',  ( 760.0363995740630116, -298.9181544815161828, 368.7758568127991907 ) ) ;
#29422 = CARTESIAN_POINT ( 'NONE',  ( 748.3538107759620743, -232.7146871989596377, -355.8262568251490165 ) ) ;
#29423 = CARTESIAN_POINT ( 'NONE',  ( 815.2698199232961542, -256.8164208402379245, 342.5225473063383106 ) ) ;
#29424 = CARTESIAN_POINT ( 'NONE',  ( 786.4999999999993179, 26.27639943461401018, 900.0000000000001137 ) ) ;
#29425 = ORIENTED_EDGE ( 'NONE', *, *, #18559, .F. ) ;
#29426 = CARTESIAN_POINT ( 'NONE',  ( 765.0180583372156207, -336.9982390220558273, 360.0135310231089534 ) ) ;
#29427 = CARTESIAN_POINT ( 'NONE',  ( 754.7162404726377645, -86.73633629969862113, 339.4709603349214717 ) ) ;
#29428 = CARTESIAN_POINT ( 'NONE',  ( 755.8398074228967971, -19.44195992623303937, -333.4516893846970333 ) ) ;
#29429 = CARTESIAN_POINT ( 'NONE',  ( 799.9999999999993179, -512.9681489794448908, -329.9999999999999432 ) ) ;
#29430 = PLANE ( 'NONE',  #23287 ) ;
#29432 = CARTESIAN_POINT ( 'NONE',  ( 788.8264449731200330, -381.1800572038737869, 363.6646147819171233 ) ) ;
#29431 = CARTESIAN_POINT ( 'NONE',  ( 789.9200121543843807, -169.9874144716871172, 317.0176451133914384 ) ) ;
#29433 = ORIENTED_EDGE ( 'NONE', *, *, #35997, .F. ) ;
#29434 = CARTESIAN_POINT ( 'NONE',  ( 775.9200461376533440, -335.8055962898683902, -315.3028492785443291 ) ) ;
#29435 = CARTESIAN_POINT ( 'NONE',  ( 800.2193346964447755, -162.9982390220563673, 355.1360043628815788 ) ) ;
#29436 = CARTESIAN_POINT ( 'NONE',  ( 751.2241431872005251, -328.1692326535048210, -359.9636004259367610 ) ) ;
#29437 = DIRECTION ( 'NONE',  ( 0.000000000000000000, 0.000000000000000000, 1.000000000000000000 ) ) ;
#29438 = CARTESIAN_POINT ( 'NONE',  ( 812.7932403749906598, 8.819942796124882634, 327.7687537140311633 ) ) ;
#29439 = ORIENTED_EDGE ( 'NONE', *, *, #38242, .F. ) ;
#29440 = CARTESIAN_POINT ( 'NONE',  ( 801.9419747391806368, -354.4527844766012095, 351.9812246680014027 ) ) ;
#29441 = AXIS2_PLACEMENT_3D ( 'NONE', #37877, #12701, #26781 ) ;
#29442 = CARTESIAN_POINT ( 'NONE',  ( 775.9200461376533440, -71.80559628986922860, -315.3028492785443291 ) ) ;
#29443 = ORIENTED_EDGE ( 'NONE', *, *, #34861, .F. ) ;
#29444 = CARTESIAN_POINT ( 'NONE',  ( 755.0636971347428243, -436.2709662947827951, 341.7834795799807353 ) ) ;
#29445 = EDGE_CURVE ( 'NONE', #27321, #18957, #40936, .T. ) ;
#29446 = CARTESIAN_POINT ( 'NONE',  ( 813.1304606946830518, -185.9073299311472454, -352.3570229623690580 ) ) ;
#29447 = VERTEX_POINT ( 'NONE', #16348 ) ;
#29448 = CARTESIAN_POINT ( 'NONE',  ( 804.9363028652555840, -184.2709662947835909, -338.2165204200192079 ) ) ;
#29449 = ORIENTED_EDGE ( 'NONE', *, *, #28382, .F. ) ;
#29450 = CARTESIAN_POINT ( 'NONE',  ( 800.9840315886518738, -436.9181544815157281, -354.1144889064786412 ) ) ;
#29451 = CARTESIAN_POINT ( 'NONE',  ( 792.1044303154645831, 11.54721552339760038, 317.8323909638837677 ) ) ;
#29452 = CARTESIAN_POINT ( 'NONE',  ( 780.5290396650775619, -156.3510508353235480, 365.2837595273619513 ) ) ;
#29454 = DIRECTION ( 'NONE',  ( 0.000000000000000000, 0.000000000000000000, -1.000000000000000000 ) ) ;
#29453 = LINE ( 'NONE', #19727, #20331 ) ;
#29455 = ADVANCED_FACE ( 'NONE', ( #37593 ), #33899, .F. ) ;
#29456 = ORIENTED_EDGE ( 'NONE', *, *, #19291, .F. ) ;
#29457 = CARTESIAN_POINT ( 'NONE',  ( 796.1575198192839480, -438.0090635724247932, -359.4546378042384163 ) ) ;
#29458 = FACE_OUTER_BOUND ( 'NONE', #40073, .T. ) ;
#29459 = CARTESIAN_POINT ( 'NONE',  ( 795.8262568251477660, -214.3726999360618493, -308.3538107759623585 ) ) ;
#29460 = CARTESIAN_POINT ( 'NONE',  ( 814.4686193811664907, -75.28179084515321051, 346.2056067578752732 ) ) ;
#29462 = CARTESIAN_POINT ( 'NONE',  ( 311.1634899080286232, 256.5000000000000000, -197.2499999999963904 ) ) ;
#29461 = DIRECTION ( 'NONE',  ( -1.880165489482579047E-16, -1.000000000000000000, 0.000000000000000000 ) ) ;
#29463 = CARTESIAN_POINT ( 'NONE',  ( 769.1273215169530886, -334.7146871989593251, -317.4527132478988847 ) ) ;
#29464 = LINE ( 'NONE', #4526, #33555 ) ;
#29465 = CARTESIAN_POINT ( 'NONE',  ( 755.8990559732751535, -203.4636090269709996, -365.9055244015606831 ) ) ;
#29466 = CARTESIAN_POINT ( 'NONE',  ( -78.83651009197140525, 230.0000000000000568, -199.9999999999936051 ) ) ;
#29467 = DIRECTION ( 'NONE',  ( 0.000000000000000000, -1.000000000000000000, 0.000000000000000000 ) ) ;
#29468 = CARTESIAN_POINT ( 'NONE',  ( 805.2837595273609850, -386.7363362996977116, 340.5290396650784714 ) ) ;
#29469 = CARTESIAN_POINT ( 'NONE',  ( 763.0537975583476964, -240.4527844766015789, -371.0346526505628617 ) ) ;
#29470 = EDGE_CURVE ( 'NONE', #33885, #577, #23268, .T. ) ;
#29471 = DIRECTION ( 'NONE',  ( -1.880165489482579047E-16, -1.000000000000000000, -0.000000000000000000 ) ) ;
#29472 = CARTESIAN_POINT ( 'NONE',  ( 757.8323909638827445, -2.634602658420536869, -352.1044303154654358 ) ) ;
#29473 = CIRCLE ( 'NONE', #26521, 20.00000000000004619 ) ;
#29474 = CARTESIAN_POINT ( 'NONE',  ( 754.3581564841646241, -185.4636090269710280, 316.1443688327762516 ) ) ;
#29475 = EDGE_CURVE ( 'NONE', #23953, #17397, #12883, .T. ) ;
#29476 = CARTESIAN_POINT ( 'NONE',  ( 807.5423716828161105, -129.0783235625963243, -362.2119215644372048 ) ) ;
#29477 = CARTESIAN_POINT ( 'NONE',  ( 763.2262854647970016, -152.6346026584200786, 309.2812353651462445 ) ) ;
#29478 = CARTESIAN_POINT ( 'NONE',  ( 751.9810565676468741, -362.0891481129648923, -360.9747183278973921 ) ) ;
#29479 = DIRECTION ( 'NONE',  ( 0.000000000000000000, -0.000000000000000000, -1.000000000000000000 ) ) ;
#29480 = DIRECTION ( 'NONE',  ( -1.000000000000000000, -0.000000000000000000, -0.000000000000000000 ) ) ;
#29481 = EDGE_CURVE ( 'NONE', #755, #8326, #37233, .T. ) ;
#29482 = CARTESIAN_POINT ( 'NONE',  ( 805.1927285166397041, -232.8164208402379245, 341.8018195045277707 ) ) ;
#29483 = CARTESIAN_POINT ( 'NONE',  ( 790.9844846989617508, -22.37269993606246743, 317.2208543904092721 ) ) ;
#29484 = CARTESIAN_POINT ( 'NONE',  ( 774.6312213355099630, -407.3618753856920307, -364.6798772138717482 ) ) ;
#29485 = CARTESIAN_POINT ( 'NONE',  ( 808.3070685750230950, -450.9982390220554294, -361.1904061080339261 ) ) ;
#29486 = DIRECTION ( 'NONE',  ( 8.659560562354869996E-17, 0.7071067811865526798, -0.7071067811865423547 ) ) ;
#29487 = CARTESIAN_POINT ( 'NONE',  ( 754.0944755984390895, -39.62377810805116951, 364.1009440267246760 ) ) ;
#29488 = VERTEX_POINT ( 'NONE', #8964 ) ;
#29489 = CARTESIAN_POINT ( 'NONE',  ( 783.0433043558608688, -216.8965053807778816, -315.1538015810313027 ) ) ;
#29490 = CARTESIAN_POINT ( 'NONE',  ( 765.0180583372156207, -24.99823902205683268, 360.0135310231089534 ) ) ;
#29491 = CARTESIAN_POINT ( 'NONE',  ( 746.7653713866222915, -233.2601417444141987, -351.0478386215610271 ) ) ;
#29492 = FACE_OUTER_BOUND ( 'NONE', #24074, .T. ) ;
#29493 = CARTESIAN_POINT ( 'NONE',  ( 800.1688906516307043, -346.1692326535047641, 369.0717654672308186 ) ) ;
#29494 = VERTEX_POINT ( 'NONE', #15668 ) ;
#29495 = CARTESIAN_POINT ( 'NONE',  ( 764.3348316497523456, -430.7146871989590409, 308.6759233522265617 ) ) ;
#29496 = EDGE_CURVE ( 'NONE', #34870, #811, #2555, .T. ) ;
#29497 = CARTESIAN_POINT ( 'NONE',  ( 802.1676090361156639, -350.6346026584192828, 327.8955696845344505 ) ) ;
#29498 = ADVANCED_FACE ( 'NONE', ( #23033 ), #37128, .F. ) ;
#29499 = CARTESIAN_POINT ( 'NONE',  ( 754.9967657858570647, -73.54369356751118403, -365.0032342141425374 ) ) ;
#29500 = CARTESIAN_POINT ( 'NONE',  ( 800.2193346964446619, -66.99823902205670834, -355.1360043628816925 ) ) ;
#29501 = ORIENTED_EDGE ( 'NONE', *, *, #21886, .T. ) ;
#29502 = CARTESIAN_POINT ( 'NONE',  ( 805.2837595273609850, -26.73633629969882008, -340.5290396650784714 ) ) ;
#29503 = ORIENTED_EDGE ( 'NONE', *, *, #18785, .T. ) ;
#29504 = CARTESIAN_POINT ( 'NONE',  ( 801.5560724626406000, -312.5545181178797520, -326.7756240680316182 ) ) ;
#29506 = CARTESIAN_POINT ( 'NONE',  ( 800.9840315886518738, -364.9181544815158986, 354.1144889064786412 ) ) ;
#29505 = CARTESIAN_POINT ( 'NONE',  ( 792.1044303154645831, -60.45278447660215448, 317.8323909638837677 ) ) ;
#29507 = CARTESIAN_POINT ( 'NONE',  ( 767.8955696845333705, -336.4527844766012095, -362.1676090361162323 ) ) ;
#29509 = CARTESIAN_POINT ( 'NONE',  ( 812.6845335610512393, -319.9874144716866340, 353.5525998758768651 ) ) ;
#29508 = CARTESIAN_POINT ( 'NONE',  ( 814.5518280994195948, -423.7255117493282341, 332.4837098697145166 ) ) ;
#29510 = EDGE_CURVE ( 'NONE', #3360, #25515, #12165, .T. ) ;
#29511 = CARTESIAN_POINT ( 'NONE',  ( 759.8311093483677041, -94.16923265350555994, 310.9282345327691814 ) ) ;
#29512 = CARTESIAN_POINT ( 'NONE',  ( 769.0155153010367712, -322.3726999360615082, -362.7791456095907279 ) ) ;
#29513 = CARTESIAN_POINT ( 'NONE',  ( 803.4237431249931660, -303.1800572038740711, -331.2633955100225194 ) ) ;
#29514 = CARTESIAN_POINT ( 'NONE',  ( -786.4999999999993179, -496.5085659523897448, -356.8883017825714319 ) ) ;
#29515 = CARTESIAN_POINT ( 'NONE',  ( 785.3141322388236176, -141.7255117493291721, -364.4286716492789537 ) ) ;
#29516 = DIRECTION ( 'NONE',  ( 0.000000000000000000, 0.000000000000000000, -1.000000000000000000 ) ) ;
#29517 = CARTESIAN_POINT ( 'NONE',  ( 792.2312462859673587, -419.9073299311465348, 307.2067596250082602 ) ) ;
#29519 = CARTESIAN_POINT ( 'NONE',  ( 746.4999999999993179, -365.3551492539851893, -8.132432514707076621 ) ) ;
#29518 = DIRECTION ( 'NONE',  ( -0.000000000000000000, -0.000000000000000000, -1.000000000000000000 ) ) ;
#29520 = CARTESIAN_POINT ( 'NONE',  ( 747.6481478633932056, -85.09997266333499510, -353.4146539503763620 ) ) ;
#29521 = DIRECTION ( 'NONE',  ( 0.000000000000000000, 0.000000000000000000, -1.000000000000000000 ) ) ;
#29522 = CARTESIAN_POINT ( 'NONE',  ( 914.9999999999992042, 99.99999999999984368, 350.0000000000000000 ) ) ;
#29523 = CARTESIAN_POINT ( 'NONE',  ( 769.9779781133707957, -307.0999726633343130, 316.7813123517150871 ) ) ;
#29524 = CARTESIAN_POINT ( 'NONE',  ( 788.7366044899766848, -155.9073299311473306, 316.5762568750059813 ) ) ;
#29525 = ORIENTED_EDGE ( 'NONE', *, *, #955, .F. ) ;
#29526 = CARTESIAN_POINT ( 'NONE',  ( 814.9108240113580450, -136.2709662947837330, -337.5031285880265273 ) ) ;
#29527 = CARTESIAN_POINT ( 'NONE',  ( 784.0799538623451781, -323.8055962898684470, 364.6971507214555572 ) ) ;
#29528 = LINE ( 'NONE', #43603, #4962 ) ;
#29529 = CARTESIAN_POINT ( 'NONE',  ( 783.7953271457878373, -80.19088175424411702, 375.1787889125761239 ) ) ;
#29530 = EDGE_CURVE ( 'NONE', #44323, #34939, #26289, .T. ) ;
#29531 = CARTESIAN_POINT ( 'NONE',  ( 810.7187646348534145, -282.4527844766014937, -356.7737145352016341 ) ) ;
#29532 = CARTESIAN_POINT ( 'NONE',  ( 759.0252816721024374, -192.9982390220562820, 368.0189434323527280 ) ) ;
#29533 = CARTESIAN_POINT ( 'NONE',  ( 757.8323909638827445, -122.6346026584201354, 352.1044303154654358 ) ) ;
#29534 = VERTEX_POINT ( 'NONE', #5264 ) ;
#29535 = CARTESIAN_POINT ( 'NONE',  ( 746.0683387631852383, -355.4419599262319593, -331.3260364891676204 ) ) ;
#29536 = CARTESIAN_POINT ( 'NONE',  ( 754.9967657858570647, -97.54369356751112718, -365.0032342141425374 ) ) ;
#29537 = CARTESIAN_POINT ( 'NONE',  ( 761.4292242960306112, -17.46360902697157513, 323.2154366446414429 ) ) ;
#29538 = CARTESIAN_POINT ( 'NONE',  ( 814.2001403089898304, -353.3618753856922012, -347.4397851343538264 ) ) ;
#29539 = DIRECTION ( 'NONE',  ( 0.000000000000000000, 1.000000000000000000, -0.000000000000000000 ) ) ;
#29540 = CARTESIAN_POINT ( 'NONE',  ( 756.7813123517142913, -379.9874144716865203, 329.9779781133712504 ) ) ;
#29541 = ORIENTED_EDGE ( 'NONE', *, *, #771, .F. ) ;
#29542 = CARTESIAN_POINT ( 'NONE',  ( 796.7845633553578182, -81.62377810805104161, 358.5707757039688204 ) ) ;
#29543 = CARTESIAN_POINT ( 'NONE',  ( 804.4286716492782716, -425.3618753856919170, -345.3141322388244703 ) ) ;
#29544 = CARTESIAN_POINT ( 'NONE',  ( 804.4286716492782716, -209.3618753856926276, -345.3141322388244703 ) ) ;
#29545 = CARTESIAN_POINT ( 'NONE',  ( 771.2368401574024119, -109.4419599262327836, -374.2805881961240857 ) ) ;
#29546 = DIRECTION ( 'NONE',  ( 1.000000000000000000, -8.326672684688676025E-16, 0.000000000000000000 ) ) ;
#29547 = CARTESIAN_POINT ( 'NONE',  ( 814.8230680027162407, -245.8055962898686460, 333.7305795820267917 ) ) ;
#29548 = CARTESIAN_POINT ( 'NONE',  ( 788.8264449731201466, -45.18005720387493795, 363.6646147819170665 ) ) ;
#29549 = ADVANCED_FACE ( 'NONE', ( #44528 ), #18798, .F. ) ;
#29550 = CARTESIAN_POINT ( 'NONE',  ( 800.7704444035546203, -244.1692326535050768, -326.0291762391768771 ) ) ;
#29551 = CARTESIAN_POINT ( 'NONE',  ( 754.8072714833581358, -220.8164208402379529, 338.1981804954720587 ) ) ;
#29552 = EDGE_CURVE ( 'NONE', #24407, #7346, #23493, .T. ) ;
#29553 = CARTESIAN_POINT ( 'NONE',  ( 767.6429770376289525, 14.81994279612486309, -306.8695393053162093 ) ) ;
#29554 = CARTESIAN_POINT ( 'NONE',  ( 801.9858362298568863, -51.07832356259657303, -312.7379699480935642 ) ) ;
#29555 = CARTESIAN_POINT ( 'NONE',  ( 799.9999999999993179, 205.0000000000000568, 339.9999999999999432 ) ) ;
#29556 = ORIENTED_EDGE ( 'NONE', *, *, #569, .T. ) ;
#29557 = EDGE_LOOP ( 'NONE', ( #15136, #33966 ) ) ;
#29558 = CARTESIAN_POINT ( 'NONE',  ( 762.1177392798416577, -378.5545181178795247, -309.8865473780659272 ) ) ;
#29559 = EDGE_CURVE ( 'NONE', #38375, #44144, #9949, .T. ) ;
#29560 = CARTESIAN_POINT ( 'NONE',  ( 748.9653473494365699, -290.6346026584196238, 356.9462024416520762 ) ) ;
#29561 = CARTESIAN_POINT ( 'NONE',  ( 813.2346286133761168, -29.26014174441482751, 328.9521613784389160 ) ) ;
#29562 = CARTESIAN_POINT ( 'NONE',  ( 779.4763451958990572, -200.7363362996982801, -365.0264073115438919 ) ) ;
#29563 = CARTESIAN_POINT ( 'NONE',  ( 778.2165204200184689, -166.8164208402382087, -364.9363028652563230 ) ) ;
#29564 = CARTESIAN_POINT ( 'NONE',  ( 800.0135310231082713, -398.0891481129647218, -325.0180583372163028 ) ) ;
#29565 = EDGE_LOOP ( 'NONE', ( #40424, #4935, #27567, #41996 ) ) ;
#29566 = ORIENTED_EDGE ( 'NONE', *, *, #665, .T. ) ;
#29567 = CARTESIAN_POINT ( 'NONE',  ( 777.4774526936600978, -322.2709662947830225, 304.7301800767027657 ) ) ;
#29568 = PLANE ( 'NONE',  #17452 ) ;
#29569 = CARTESIAN_POINT ( 'NONE',  ( 758.6633372737375112, -356.5328690171410813, 326.9102291470432533 ) ) ;
#29570 = LINE ( 'NONE', #42808, #24067 ) ;
#29571 = DIRECTION ( 'NONE',  ( 0.000000000000000000, 1.000000000000000000, 0.000000000000000000 ) ) ;
#29572 = CARTESIAN_POINT ( 'NONE',  ( 772.4468031744293057, -177.8272453906074304, 363.8651313633793620 ) ) ;
#29573 = CARTESIAN_POINT ( 'NONE',  ( 804.6798772138708955, -63.72551174932939233, 334.6312213355107019 ) ) ;
#29574 = ORIENTED_EDGE ( 'NONE', *, *, #3258, .F. ) ;
#29575 = CARTESIAN_POINT ( 'NONE',  ( 791.0478386215596629, -429.8272453906067199, -306.7653713866226326 ) ) ;
#29576 = CARTESIAN_POINT ( 'NONE',  ( 767.6429770376291799, -33.18005720387498769, -306.8695393053162093 ) ) ;
#29577 = CARTESIAN_POINT ( 'NONE',  ( 761.2382568024794409, -231.6237781080504874, 356.9571628226838129 ) ) ;
#29578 = CARTESIAN_POINT ( 'NONE',  ( 755.3201227861273992, -387.7255117493283478, -345.3687786644892981 ) ) ;
#29579 = CARTESIAN_POINT ( 'NONE',  ( 785.3687786644885591, -11.36187538569323863, -315.3201227861280813 ) ) ;
#29580 = CARTESIAN_POINT ( 'NONE',  ( 758.8095938919642549, -416.0891481129645513, 311.6929314249763365 ) ) ;
#29581 = CARTESIAN_POINT ( 'NONE',  ( 51.16348990802859475, 260.0000000000000568, -199.9999999999945146 ) ) ;
#29582 = CARTESIAN_POINT ( 'NONE',  ( 757.4527132478984868, -256.3726999360617924, -329.1273215169538844 ) ) ;
#29583 = CARTESIAN_POINT ( 'NONE',  ( 814.9108240113580450, -160.2709662947836762, -337.5031285880265273 ) ) ;
#29584 = CARTESIAN_POINT ( 'NONE',  ( 745.7998596910086917, -53.36187538569310362, 332.5602148656461168 ) ) ;
#29585 = CARTESIAN_POINT ( 'NONE',  ( 759.0252816721024374, -96.99823902205660886, 368.0189434323527280 ) ) ;
#29586 = CARTESIAN_POINT ( 'NONE',  ( 779.2785047387700388, 16.45630643248848912, -314.0977342670951202 ) ) ;
#29587 = DIRECTION ( 'NONE',  ( -0.000000000000000000, 1.000000000000000000, -0.000000000000000000 ) ) ;
#29588 = CARTESIAN_POINT ( 'NONE',  ( 757.7880784355613741, -378.0090635724250774, 312.4576283171834916 ) ) ;
#29589 = PLANE ( 'NONE',  #4391 ) ;
#29590 = CARTESIAN_POINT ( 'NONE',  ( 751.9810565676468741, -362.0891481129648923, 360.9747183278973921 ) ) ;
#29591 = CARTESIAN_POINT ( 'NONE',  ( 759.9864689768902508, -314.0891481129650629, -354.9819416627836404 ) ) ;
#29592 = CARTESIAN_POINT ( 'NONE',  ( 787.6308680596127942, 12.73985825558503926, 364.1105419155492768 ) ) ;
#29593 = CARTESIAN_POINT ( 'NONE',  ( 745.7194118038753459, -85.64542720878952764, -348.7631598425976449 ) ) ;
#29594 = CARTESIAN_POINT ( 'NONE',  ( 805.1016975059191054, -126.8965053807781516, -343.0745993439771837 ) ) ;
#29595 = CARTESIAN_POINT ( 'NONE',  ( 805.9055244015594326, -123.6237781080508569, 315.8990559732753240 ) ) ;
#29596 = CYLINDRICAL_SURFACE ( 'NONE', #35051, 2.749999999999863665 ) ;
#29597 = CARTESIAN_POINT ( 'NONE',  ( 792.1044303154645831, -12.45278447660232146, -317.8323909638837677 ) ) ;
#29598 = CARTESIAN_POINT ( 'NONE',  ( 754.8983024940795303, -114.8965053807782226, -336.9254006560228163 ) ) ;
#29599 = CARTESIAN_POINT ( 'NONE',  ( 774.6312213355099630, -119.3618753856928691, -364.6798772138717482 ) ) ;
#29600 = CARTESIAN_POINT ( 'NONE',  ( 802.1676090361156639, -134.6346026584201070, 327.8955696845344505 ) ) ;
#29601 = CARTESIAN_POINT ( 'NONE',  ( 798.7617431975189675, -435.6237781080499190, -323.0428371773161871 ) ) ;
#29603 = CARTESIAN_POINT ( 'NONE',  ( 802.1676090361155502, -254.6346026584197091, 327.8955696845344505 ) ) ;
#29602 = CARTESIAN_POINT ( 'NONE',  ( 794.9819416627830151, -252.9982390220560831, 319.9864689768909898 ) ) ;
#29604 = DIRECTION ( 'NONE',  ( 0.000000000000000000, 1.000000000000000000, 0.000000000000000000 ) ) ;
#29605 = ORIENTED_EDGE ( 'NONE', *, *, #5829, .T. ) ;
#29606 = CARTESIAN_POINT ( 'NONE',  ( 800.7704444035546203, 19.83076734649410966, 326.0291762391768771 ) ) ;
#29607 = VERTEX_POINT ( 'NONE', #12433 ) ;
#29608 = DIRECTION ( 'NONE',  ( 0.000000000000000000, 0.000000000000000000, 1.000000000000000000 ) ) ;
#29609 = CARTESIAN_POINT ( 'NONE',  ( 792.2312462859673587, -179.9073299311472454, 307.2067596250082602 ) ) ;
#29610 = CARTESIAN_POINT ( 'NONE',  ( 761.4292242960306112, -305.4636090269706870, 323.2154366446414429 ) ) ;
#29611 = CARTESIAN_POINT ( 'NONE',  ( 776.9566956441375396, -396.8965053807772847, 364.8461984189686405 ) ) ;
#29612 = VERTEX_POINT ( 'NONE', #40402 ) ;
#29613 = CARTESIAN_POINT ( 'NONE',  ( 757.4527132478984868, -64.37269993606231822, -329.1273215169538844 ) ) ;
#29614 = CARTESIAN_POINT ( 'NONE',  ( 755.0636971347428243, -292.2709662947831930, -341.7834795799807353 ) ) ;
#29615 = VERTEX_POINT ( 'NONE', #30207 ) ;
#29616 = CARTESIAN_POINT ( 'NONE',  ( 764.8639956371174549, -392.0891481129648355, -319.7806653035542013 ) ) ;
#29617 = CARTESIAN_POINT ( 'NONE',  ( 788.8264449731200330, -45.18005720387493085, -363.6646147819171233 ) ) ;
#29618 = CARTESIAN_POINT ( 'NONE',  ( 800.7704444035546203, -268.1692326535049347, 326.0291762391768771 ) ) ;
#29619 = DIRECTION ( 'NONE',  ( 1.000000000000000000, 0.000000000000000000, 0.000000000000000000 ) ) ;
#29620 = FACE_BOUND ( 'NONE', #14652, .T. ) ;
#29621 = DIRECTION ( 'NONE',  ( -1.000000000000000000, -0.000000000000000000, -0.000000000000000000 ) ) ;
#29622 = ORIENTED_EDGE ( 'NONE', *, *, #1300, .F. ) ;
#29623 = CARTESIAN_POINT ( 'NONE',  ( 788.6739635108323228, -295.6454272087888739, -373.9316612368139090 ) ) ;
#29625 = CARTESIAN_POINT ( 'NONE',  ( 803.6646147819161570, -281.9073299311468759, -348.8264449731210561 ) ) ;
#29624 = CARTESIAN_POINT ( 'NONE',  ( 998.9999999999992042, -600.0000000000001137, -360.0000000000000000 ) ) ;
#29626 = DIRECTION ( 'NONE',  ( 0.000000000000000000, 1.000000000000000000, 0.000000000000000000 ) ) ;
#29627 = CARTESIAN_POINT ( 'NONE',  ( 766.9102291470427417, -162.5545181178802352, -318.6633372737382501 ) ) ;
#29628 = CARTESIAN_POINT ( 'NONE',  ( 813.1304606946830518, -17.90732993114776406, 352.3570229623690580 ) ) ;
#29629 = LINE ( 'NONE', #9745, #27672 ) ;
#29630 = CARTESIAN_POINT ( 'NONE',  ( 758.0141637701419768, -15.07832356259669560, -367.2620300519063790 ) ) ;
#29631 = CARTESIAN_POINT ( 'NONE',  ( 777.5031285880264704, -358.8164208402375834, -374.9108240113588408 ) ) ;
#29632 = DIRECTION ( 'NONE',  ( -1.000000000000000000, -0.000000000000000000, -0.000000000000000000 ) ) ;
#29633 = CARTESIAN_POINT ( 'NONE',  ( 778.1981804954714335, -58.27096629478398171, 314.8072714833589885 ) ) ;
#29634 = CARTESIAN_POINT ( 'NONE',  ( 814.4686193811664907, -291.2817908451525000, 346.2056067578752732 ) ) ;
#29635 = CARTESIAN_POINT ( 'NONE',  ( 782.4968714119720516, -250.8164208402379245, 305.0891759886411023 ) ) ;
#29636 = CARTESIAN_POINT ( 'NONE',  ( 803.8556311672234642, -441.6237781080499190, -365.6418435158340117 ) ) ;
#29637 = FACE_OUTER_BOUND ( 'NONE', #33864, .T. ) ;
#29638 = ORIENTED_EDGE ( 'NONE', *, *, #28934, .T. ) ;
#29639 = CARTESIAN_POINT ( 'NONE',  ( 759.7806653035534055, -366.9982390220556567, 324.8639956371180801 ) ) ;
#29640 = CARTESIAN_POINT ( 'NONE',  ( 755.8894580844503253, -135.8272453906076009, 332.3691319403863531 ) ) ;
#29641 = CARTESIAN_POINT ( 'NONE',  ( 786.6156483768007774, -1.441959926233096656, -315.5913626894246136 ) ) ;
#29642 = DIRECTION ( 'NONE',  ( 0.000000000000000000, 0.000000000000000000, 1.000000000000000000 ) ) ;
#29643 = FACE_OUTER_BOUND ( 'NONE', #9659, .T. ) ;
#29644 = CARTESIAN_POINT ( 'NONE',  ( 812.6845335610512393, -127.9874144716872308, 353.5525998758768651 ) ) ;
#29645 = CARTESIAN_POINT ( 'NONE',  ( 759.7806653035534055, -390.9982390220557136, 324.8639956371180801 ) ) ;
#29646 = VERTEX_POINT ( 'NONE', #36693 ) ;
#29647 = CARTESIAN_POINT ( 'NONE',  ( 804.9511171171677688, -317.8055962898684470, -335.8780910478229202 ) ) ;
#29648 = CARTESIAN_POINT ( 'NONE',  ( 759.9864689768902508, -170.0891481129654608, 354.9819416627836404 ) ) ;
#29649 = UNCERTAINTY_MEASURE_WITH_UNIT (LENGTH_MEASURE( 1.000000000000000082E-05 ), #16477, 'distance_accuracy_value', 'NONE');
#29650 = EDGE_CURVE ( 'NONE', #9272, #8247, #44297, .T. ) ;
#29651 = CARTESIAN_POINT ( 'NONE',  ( 807.5423716828161105, -345.0783235625956991, -362.2119215644372048 ) ) ;
#29652 = LINE ( 'NONE', #30553, #30055 ) ;
#29653 = ORIENTED_EDGE ( 'NONE', *, *, #3849, .T. ) ;
#29654 = CARTESIAN_POINT ( 'NONE',  ( 805.1927285166397041, -352.8164208402374129, 341.8018195045277707 ) ) ;
#29655 = ORIENTED_EDGE ( 'NONE', *, *, #37131, .F. ) ;
#29656 = CARTESIAN_POINT ( 'NONE',  ( 804.4286716492782716, -449.3618753856918602, 345.3141322388244703 ) ) ;
#29657 = CARTESIAN_POINT ( 'NONE',  ( 814.9108240113580450, -184.2709662947835909, -337.5031285880265273 ) ) ;
#29658 = CARTESIAN_POINT ( 'NONE',  ( 751.9810565676468741, -98.08914811296568814, 360.9747183278973921 ) ) ;
#29659 = ORIENTED_EDGE ( 'NONE', *, *, #28628, .F. ) ;
#29660 = AXIS2_PLACEMENT_3D ( 'NONE', #30354, #34046, #44446 ) ;
#29661 = CARTESIAN_POINT ( 'NONE',  ( 801.9419747391806368, -162.4527844766018632, -351.9812246680014027 ) ) ;
#29662 = ORIENTED_EDGE ( 'NONE', *, *, #44509, .F. ) ;
#29663 = CARTESIAN_POINT ( 'NONE',  ( 761.4292242960306112, -425.4636090269703459, -323.2154366446414429 ) ) ;
#29664 = CARTESIAN_POINT ( 'NONE',  ( 755.0636971347428243, -4.270966294784170003, 341.7834795799807353 ) ) ;
#29665 = CARTESIAN_POINT ( 'NONE',  ( 772.3691319403857278, -167.2601417444143976, 315.8894580844506663 ) ) ;
#29667 = DIRECTION ( 'NONE',  ( 0.000000000000000000, 0.000000000000000000, 1.000000000000000000 ) ) ;
#29666 = CARTESIAN_POINT ( 'NONE',  ( 927.9999999999992042, 154.9999999999998863, 350.0000000000000000 ) ) ;
#29668 = ORIENTED_EDGE ( 'NONE', *, *, #37727, .T. ) ;
#29669 = ADVANCED_FACE ( 'NONE', ( #1570, #29748 ), #8752, .F. ) ;
#29670 = CARTESIAN_POINT ( 'NONE',  ( 773.4516893846965786, -427.6454272087885897, -315.8398074228977066 ) ) ;
#29671 = CARTESIAN_POINT ( 'NONE',  ( 745.1792804349281596, -206.1908817542437191, -343.7566961878542884 ) ) ;
#29672 = CARTESIAN_POINT ( 'NONE',  ( 802.2119215644370342, -78.00906357242591582, 367.5423716828165084 ) ) ;
#29674 = CARTESIAN_POINT ( 'NONE',  ( 755.3201227861273992, -171.7255117493291152, -345.3687786644892981 ) ) ;
#29673 = DIRECTION ( 'NONE',  ( -0.000000000000000000, 1.000000000000000000, -0.000000000000000000 ) ) ;
#29675 = CARTESIAN_POINT ( 'NONE',  ( 755.8398074228967971, -331.4419599262320162, -333.4516893846970333 ) ) ;
#29676 = DIRECTION ( 'NONE',  ( 0.000000000000000000, -0.9238795325112892920, 0.3826834323650836756 ) ) ;
#29677 = CARTESIAN_POINT ( 'NONE',  ( 797.8822607201568644, -222.5545181178800362, -370.1134526219340160 ) ) ;
#29678 = CARTESIAN_POINT ( 'NONE',  ( -786.4999999999993179, -436.2161768796786987, 399.7184814855371542 ) ) ;
#29679 = LINE ( 'NONE', #15597, #3172 ) ;
#29680 = CARTESIAN_POINT ( 'NONE',  ( 793.0897708529556667, -30.55451811788062244, -361.3366627262616362 ) ) ;
#29681 = CARTESIAN_POINT ( 'NONE',  ( 793.0897708529556667, -414.5545181178795247, 361.3366627262616362 ) ) ;
#29682 = VECTOR ( 'NONE', #40386, 1000.000000000000000 ) ;
#29683 = CARTESIAN_POINT ( 'NONE',  ( 751.6929314249750860, -246.9982390220560831, -318.8095938919659034 ) ) ;
#29684 = CARTESIAN_POINT ( 'NONE',  ( 755.8894580844503253, -231.8272453906072315, 332.3691319403863531 ) ) ;
#29685 = DIRECTION ( 'NONE',  ( -0.000000000000000000, -0.000000000000000000, 1.000000000000000000 ) ) ;
#29686 = CARTESIAN_POINT ( 'NONE',  ( 754.8072714833581358, -28.81642084023863148, -338.1981804954720587 ) ) ;
#29687 = CARTESIAN_POINT ( 'NONE',  ( 812.3518521366052028, -193.0999726633346256, 326.5853460496235243 ) ) ;
#29688 = CARTESIAN_POINT ( 'NONE',  ( 747.3154664389472828, -115.9874144716872877, -326.4474001241230781 ) ) ;
#29689 = CARTESIAN_POINT ( 'NONE',  ( 812.7932403749906598, -159.1800572038746111, 327.7687537140311633 ) ) ;
#29690 = CARTESIAN_POINT ( 'NONE',  ( 748.9653473494363425, -386.6346026584191691, -356.9462024416521331 ) ) ;
#29691 = CARTESIAN_POINT ( 'NONE',  ( 0.000000000000000000, 0.000000000000000000, -244.9999999999999716 ) ) ;
#29692 = CARTESIAN_POINT ( 'NONE',  ( -959.5497976682736407, 120.6654763175833693, -2132.806278688367456 ) ) ;
#29693 = CARTESIAN_POINT ( 'NONE',  ( 791.9812246680005501, -260.6346026584197375, 361.9419747391813189 ) ) ;
#29694 = CARTESIAN_POINT ( 'NONE',  ( 784.1219089521767955, -21.28179084515337749, 315.0488828828318333 ) ) ;
#29695 = EDGE_CURVE ( 'NONE', #23353, #15565, #17507, .T. ) ;
#29696 = CARTESIAN_POINT ( 'NONE',  ( 778.1981804954714335, -394.2709662947827951, -314.8072714833589885 ) ) ;
#29697 = DIRECTION ( 'NONE',  ( 1.000000000000000000, 0.000000000000000000, 0.000000000000000000 ) ) ;
#29698 = CARTESIAN_POINT ( 'NONE',  ( 805.0032342141412300, -445.5436935675098766, -314.9967657858571783 ) ) ;
#29699 = FACE_OUTER_BOUND ( 'NONE', #8663, .T. ) ;
#29700 = CARTESIAN_POINT ( 'NONE',  ( 764.0069404352550464, -39.07832356259662276, 359.2566176426627180 ) ) ;
#29701 = EDGE_LOOP ( 'NONE', ( #7882, #43608, #36363, #36250, #30970, #42624 ) ) ;
#29702 = EDGE_CURVE ( 'NONE', #3542, #36764, #8477, .T. ) ;
#29703 = CARTESIAN_POINT ( 'NONE',  ( 764.0069404352550464, -231.0783235625960401, -359.2566176426627180 ) ) ;
#29704 = CARTESIAN_POINT ( 'NONE',  ( 803.6646147819161570, -17.90732993114776406, 348.8264449731210561 ) ) ;
#29705 = CARTESIAN_POINT ( 'NONE',  ( 813.9316612368132837, -223.4419599262323857, -348.6739635108323228 ) ) ;
#29706 = DIRECTION ( 'NONE',  ( 1.000000000000000000, 0.000000000000000000, 0.000000000000000000 ) ) ;
#29707 = CARTESIAN_POINT ( 'NONE',  ( 759.8311093483677041, -334.1692326535047073, 310.9282345327691814 ) ) ;
#29708 = VERTEX_POINT ( 'NONE', #2950 ) ;
#29709 = CARTESIAN_POINT ( 'NONE',  ( 755.5713283507202505, -341.3618753856922012, 334.6858677611754729 ) ) ;
#29710 = CARTESIAN_POINT ( 'NONE',  ( 782.4968714119720516, -82.81642084023846451, -305.0891759886411023 ) ) ;
#29711 = VECTOR ( 'NONE', #44447, 999.9999999999998863 ) ;
#29712 = CARTESIAN_POINT ( 'NONE',  ( 805.1927285166399315, -64.81642084023852135, -341.8018195045277707 ) ) ;
#29713 = ORIENTED_EDGE ( 'NONE', *, *, #18266, .T. ) ;
#29714 = CARTESIAN_POINT ( 'NONE',  ( 804.1105419155481968, -3.827245390607979303, -347.6308680596136469 ) ) ;
#29715 = ORIENTED_EDGE ( 'NONE', *, *, #8274, .F. ) ;
#29716 = CARTESIAN_POINT ( 'NONE',  ( 776.9254006560222479, -308.1908817542434349, -314.8983024940802125 ) ) ;
#29718 = CARTESIAN_POINT ( 'NONE',  ( 784.1219089521767955, -357.2817908451523294, 315.0488828828318333 ) ) ;
#29717 = CARTESIAN_POINT ( 'NONE',  ( 795.1360043628807261, -68.08914811296575920, 360.2193346964456282 ) ) ;
#29721 = CARTESIAN_POINT ( 'NONE',  ( 746.0683387631852383, -307.4419599262320730, 331.3260364891676204 ) ) ;
#29720 = FACE_OUTER_BOUND ( 'NONE', #14640, .T. ) ;
#29719 = CARTESIAN_POINT ( 'NONE',  ( 751.6929314249750860, -414.9982390220555430, 318.8095938919659034 ) ) ;
#29722 = CARTESIAN_POINT ( 'NONE',  ( 793.4146539503750546, -97.98741447168734453, 307.6481478633938877 ) ) ;
#29723 = CARTESIAN_POINT ( 'NONE',  ( 761.4292242960306112, -329.4636090269706870, -323.2154366446414429 ) ) ;
#29724 = CARTESIAN_POINT ( 'NONE',  ( 762.3223304703356007, -319.5436935675104451, -322.3223304703362828 ) ) ;
#29725 = CARTESIAN_POINT ( 'NONE',  ( 804.9363028652555840, -160.2709662947836762, -338.2165204200192079 ) ) ;
#29726 = CARTESIAN_POINT ( 'NONE',  ( 814.9108240113580450, -424.2709662947829088, 337.5031285880265273 ) ) ;
#29728 = DIRECTION ( 'NONE',  ( 0.000000000000000000, 0.7372773368101331881, -0.6755902076156503622 ) ) ;
#29727 = CARTESIAN_POINT ( 'NONE',  ( 831.1634899080286232, 229.9999999999998863, -199.9999999999999432 ) ) ;
#29729 = CARTESIAN_POINT ( 'NONE',  ( 746.4236121716829757, -111.8272453906076151, -328.8385539511384650 ) ) ;
#29730 = CARTESIAN_POINT ( 'NONE',  ( 8.137430123673030402E-14, 430.0000000000000568, 0.000000000000000000 ) ) ;
#29731 = CARTESIAN_POINT ( 'NONE',  ( 775.4999999999993179, -501.1515549466498669, -368.0974687824633520 ) ) ;
#29732 = CARTESIAN_POINT ( 'NONE',  ( 793.9708237608222134, -286.9181544815161828, 319.2295555964448681 ) ) ;
#29733 = ORIENTED_EDGE ( 'NONE', *, *, #44419, .T. ) ;
#29734 = CARTESIAN_POINT ( 'NONE',  ( 801.1904061080338124, -140.0891481129655176, -368.3070685750236066 ) ) ;
#29735 = DIRECTION ( 'NONE',  ( 0.000000000000000000, -1.000000000000000000, -0.000000000000000000 ) ) ;
#29736 = CARTESIAN_POINT ( 'NONE',  ( 750.9282345327678740, -88.91815448151682233, 319.8311093483690115 ) ) ;
#29737 = CARTESIAN_POINT ( 'NONE',  ( 804.7487373415286811, -283.5436935675105019, -364.7487373415288516 ) ) ;
#29738 = ADVANCED_FACE ( 'NONE', ( #3413 ), #20714, .F. ) ;
#29739 = CARTESIAN_POINT ( 'NONE',  ( 751.6929314249750860, -438.9982390220554294, -318.8095938919659034 ) ) ;
#29740 = CARTESIAN_POINT ( 'NONE',  ( 771.1735550268778070, -105.1800572038747248, 316.3353852180827630 ) ) ;
#29741 = AXIS2_PLACEMENT_3D ( 'NONE', #724, #35824, #24103 ) ;
#29742 = EDGE_LOOP ( 'NONE', ( #18084, #38429, #39218, #20846 ) ) ;
#29743 = CARTESIAN_POINT ( 'NONE',  ( 812.6845335610512393, -343.9874144716865771, -353.5525998758768651 ) ) ;
#29744 = VECTOR ( 'NONE', #35070, 1000.000000000000114 ) ;
#29745 = CARTESIAN_POINT ( 'NONE',  ( 767.6429770376289525, -81.18005720387481006, -306.8695393053162093 ) ) ;
#29746 = CARTESIAN_POINT ( 'NONE',  ( 798.5707757039680246, -29.46360902697153250, 356.7845633553585003 ) ) ;
#29747 = CARTESIAN_POINT ( 'NONE',  ( 751.9810565676468741, -362.0891481129648923, -360.9747183278973921 ) ) ;
#29748 = FACE_OUTER_BOUND ( 'NONE', #31318, .T. ) ;
#29749 = CARTESIAN_POINT ( 'NONE',  ( 780.5290396650775619, -396.3510508353228374, 365.2837595273619513 ) ) ;
#29750 = ORIENTED_EDGE ( 'NONE', *, *, #19370, .F. ) ;
#29751 = EDGE_CURVE ( 'NONE', #16603, #27605, #42389, .T. ) ;
#29752 = EDGE_CURVE ( 'NONE', #45702, #31705, #17260, .T. ) ;
#29753 = CARTESIAN_POINT ( 'NONE',  ( 755.0636971347428243, -220.2709662947834772, -341.7834795799807353 ) ) ;
#29754 = CARTESIAN_POINT ( 'NONE',  ( 746.7653713866222915, -113.2601417444145682, -351.0478386215610271 ) ) ;
#29755 = CARTESIAN_POINT ( 'NONE',  ( -338.8365100919713200, 260.0000000000001137, -199.9999999999917861 ) ) ;
#29756 = CARTESIAN_POINT ( 'NONE',  ( 754.0944755984390895, -255.6237781080504874, 364.1009440267246760 ) ) ;
#29757 = CARTESIAN_POINT ( 'NONE',  ( 778.1981804954715471, -58.27096629478398881, 314.8072714833591021 ) ) ;
#29758 = VECTOR ( 'NONE', #24580, 1000.000000000000000 ) ;
#29759 = VERTEX_POINT ( 'NONE', #24405 ) ;
#29760 = CARTESIAN_POINT ( 'NONE',  ( 799.4546378042377910, -225.0783235625959833, -356.1575198192848006 ) ) ;
#29761 = CARTESIAN_POINT ( 'NONE',  ( 800.0135310231082713, -230.0891481129652618, 325.0180583372163028 ) ) ;
#29762 = CARTESIAN_POINT ( 'NONE',  ( 764.3348316497523456, -430.7146871989590409, -308.6759233522265617 ) ) ;
#29763 = CARTESIAN_POINT ( 'NONE',  ( 808.7758568127978833, -76.16923265350557415, -320.0363995740631822 ) ) ;
#29764 = DIRECTION ( 'NONE',  ( 1.000000000000000000, 0.000000000000000000, -0.000000000000000000 ) ) ;
#29765 = EDGE_CURVE ( 'NONE', #21723, #40483, #4058, .T. ) ;
#29766 = VERTEX_POINT ( 'NONE', #23945 ) ;
#29767 = ORIENTED_EDGE ( 'NONE', *, *, #21597, .F. ) ;
#29768 = CARTESIAN_POINT ( 'NONE',  ( 755.8990559732751535, -371.4636090269705164, -365.9055244015606831 ) ) ;
#29769 = ADVANCED_FACE ( 'NONE', ( #24631, #9650, #10331, #6177, #41522 ), #38065, .F. ) ;
#29770 = CARTESIAN_POINT ( 'NONE',  ( 803.4237431249931660, -231.1800572038743553, -331.2633955100225194 ) ) ;
#29771 = CARTESIAN_POINT ( 'NONE',  ( 787.5162901302840055, -323.3618753856922581, 305.4481719005793252 ) ) ;
#29772 = CARTESIAN_POINT ( 'NONE',  ( 746.0683387631852383, -19.44195992623303937, 331.3260364891676204 ) ) ;
#29773 = EDGE_CURVE ( 'NONE', #44478, #30797, #14377, .T. ) ;
#29774 = CARTESIAN_POINT ( 'NONE',  ( 757.4527132478984868, -232.3726999360617924, -329.1273215169538844 ) ) ;
#29775 = CARTESIAN_POINT ( 'NONE',  ( 764.8639956371174549, -176.0891481129653755, -319.7806653035542013 ) ) ;
#29776 = VECTOR ( 'NONE', #15823, 1000.000000000000000 ) ;
#29777 = CARTESIAN_POINT ( 'NONE',  ( 781.8018195045267476, -382.2709662947829088, -365.1927285166407273 ) ) ;
#29778 = CIRCLE ( 'NONE', #9868, 2.749999999999919176 ) ;
#29779 = VERTEX_POINT ( 'NONE', #41989 ) ;
#29780 = CARTESIAN_POINT ( 'NONE',  ( 759.7806653035534055, -222.9982390220561399, 324.8639956371180801 ) ) ;
#29781 = CARTESIAN_POINT ( 'NONE',  ( 757.8323909638827445, -98.63460265842024910, -352.1044303154654358 ) ) ;
#29782 = VERTEX_POINT ( 'NONE', #41761 ) ;
#29783 = CARTESIAN_POINT ( 'NONE',  ( 748.9653473494363425, -338.6346026584195101, 356.9462024416521331 ) ) ;
#29784 = DIRECTION ( 'NONE',  ( 0.000000000000000000, 0.000000000000000000, 1.000000000000000000 ) ) ;
#29785 = DIRECTION ( 'NONE',  ( 1.000000000000000000, 0.000000000000000000, 0.000000000000000000 ) ) ;
#29786 = DIRECTION ( 'NONE',  ( 1.000000000000000000, -1.880165489482579047E-16, 0.000000000000000000 ) ) ;
#29787 = CARTESIAN_POINT ( 'NONE',  ( 779.4763451958990572, -176.7363362996983369, 365.0264073115438919 ) ) ;
#29788 = CARTESIAN_POINT ( 'NONE',  ( 795.1360043628807261, -92.08914811296568814, 360.2193346964456282 ) ) ;
#29789 = EDGE_LOOP ( 'NONE', ( #23495, #16815, #20716, #33591 ) ) ;
#29790 = CARTESIAN_POINT ( 'NONE',  ( 749.5768839229115201, -444.5545181178792973, -358.0661480581553064 ) ) ;
#29791 = CARTESIAN_POINT ( 'NONE',  ( 804.7487373415286811, -43.54369356751131903, -364.7487373415288516 ) ) ;
#29792 = CARTESIAN_POINT ( 'NONE',  ( 789.9200121543843807, -265.9874144716867477, 317.0176451133914384 ) ) ;
#29793 = CARTESIAN_POINT ( 'NONE',  ( 755.5713283507202505, -389.3618753856919739, -334.6858677611754729 ) ) ;
#29794 = CARTESIAN_POINT ( 'NONE',  ( 788.8264449731201466, 2.819942796124898621, -363.6646147819170665 ) ) ;
#29795 = VECTOR ( 'NONE', #32648, 1000.000000000000000 ) ;
#29796 = ADVANCED_FACE ( 'NONE', ( #13575 ), #10111, .T. ) ;
#29797 = CARTESIAN_POINT ( 'NONE',  ( 814.9108240113580450, -424.2709662947829088, 337.5031285880265273 ) ) ;
#29798 = CARTESIAN_POINT ( 'NONE',  ( 879.9999999999992042, 529.9999999999997726, -320.0000000000000000 ) ) ;
#29799 = CARTESIAN_POINT ( 'NONE',  ( 802.5472867521000353, -268.3726999360616787, -350.8726784830461156 ) ) ;
#29800 = CARTESIAN_POINT ( 'NONE',  ( 810.7187646348534145, -162.4527844766018632, -356.7737145352016341 ) ) ;
#29801 = ADVANCED_FACE ( 'NONE', ( #31347 ), #13814, .T. ) ;
#29802 = CARTESIAN_POINT ( 'NONE',  ( 805.0032342141412300, -37.54369356751132614, 314.9967657858571783 ) ) ;
#29803 = CARTESIAN_POINT ( 'NONE',  ( 792.3570229623688874, -141.1800572038746395, 373.1304606946836202 ) ) ;
#29804 = CARTESIAN_POINT ( 'NONE',  ( 787.3558975768202117, 16.45630643248848557, -313.9911135047267408 ) ) ;
#29805 = CARTESIAN_POINT ( 'NONE',  ( 51.16348990802859475, 256.5000000000000568, -199.9999999999945146 ) ) ;
#29806 = FACE_OUTER_BOUND ( 'NONE', #13200, .T. ) ;
#29807 = CARTESIAN_POINT ( 'NONE',  ( 796.9462024416508257, -372.4527844766010958, 308.9653473494370246 ) ) ;
#29808 = CARTESIAN_POINT ( 'NONE',  ( 762.1405469898971887, -313.5436935675102745, -357.8594530101015607 ) ) ;
#29809 = EDGE_CURVE ( 'NONE', #41260, #42341, #6859, .T. ) ;
#29810 = CARTESIAN_POINT ( 'NONE',  ( 769.1273215169530886, 25.28531280103955226, 317.4527132478988847 ) ) ;
#29811 = AXIS2_PLACEMENT_3D ( 'NONE', #943, #42542, #11811 ) ;
#29812 = CARTESIAN_POINT ( 'NONE',  ( 766.4474001241216001, -115.0999726633348956, -307.3154664389482491 ) ) ;
#29813 = CARTESIAN_POINT ( 'NONE',  ( 796.7845633553578182, -129.6237781080508853, -358.5707757039688204 ) ) ;
#29814 = CARTESIAN_POINT ( 'NONE',  ( 746.7653713866222915, -137.2601417444144829, 351.0478386215610271 ) ) ;
#29815 = CARTESIAN_POINT ( 'NONE',  ( -338.8365100919713200, 260.0000000000001137, -199.9999999999917861 ) ) ;
#29816 = CARTESIAN_POINT ( 'NONE',  ( 748.3538107759620743, -160.7146871989598651, 355.8262568251490165 ) ) ;
#29817 = CARTESIAN_POINT ( 'NONE',  ( 756.3353852180819104, -29.90732993114771787, -331.1735550268788302 ) ) ;
#29818 = CARTESIAN_POINT ( 'NONE',  ( 775.9200461376533440, -143.8055962898690154, -315.3028492785443291 ) ) ;
#29819 = CARTESIAN_POINT ( 'NONE',  ( 785.3141322388236176, -117.7255117493292715, -364.4286716492789537 ) ) ;
#29820 = CARTESIAN_POINT ( 'NONE',  ( 781.8018195045266339, -118.2709662947837899, 365.1927285166406705 ) ) ;
#29821 = CARTESIAN_POINT ( 'NONE',  ( 765.8855110935204493, -430.1692326535043094, -319.0159684113471599 ) ) ;
#29823 = CARTESIAN_POINT ( 'NONE',  ( 759.9864689768902508, -266.0891481129651197, 354.9819416627836404 ) ) ;
#29822 = CARTESIAN_POINT ( 'NONE',  ( 768.0187753319979720, -272.6346026584196807, 318.0580252608186242 ) ) ;
#29824 = PLANE ( 'NONE',  #6491 ) ;
#29825 = VERTEX_POINT ( 'NONE', #2726 ) ;
#29826 = CARTESIAN_POINT ( 'NONE',  ( 754.8983024940795303, 5.103494619221427442, 336.9254006560228163 ) ) ;
#29827 = CARTESIAN_POINT ( 'NONE',  ( 766.4474001241216001, -259.0999726633343698, -307.3154664389482491 ) ) ;
#29828 = ORIENTED_EDGE ( 'NONE', *, *, #34562, .T. ) ;
#29829 = CARTESIAN_POINT ( 'NONE',  ( 0.000000000000000000, 0.000000000000000000, 0.000000000000000000 ) ) ;
#29830 = VECTOR ( 'NONE', #36178, 1000.000000000000000 ) ;
#29831 = CARTESIAN_POINT ( 'NONE',  ( 746.8695393053151292, -221.9073299311471033, 327.6429770376306578 ) ) ;
#29832 = CARTESIAN_POINT ( 'NONE',  ( 759.0159684113467620, -304.9181544815161828, 325.8855110935213020 ) ) ;
#29833 = CARTESIAN_POINT ( 'NONE',  ( 796.7845633553578182, -393.6237781080500326, 358.5707757039688204 ) ) ;
#29834 = ORIENTED_EDGE ( 'NONE', *, *, #17111, .T. ) ;
#29835 = CARTESIAN_POINT ( 'NONE',  ( 800.9840315886518738, -124.9181544815167086, -354.1144889064786412 ) ) ;
#29836 = CARTESIAN_POINT ( 'NONE',  ( 804.9363028652555840, -280.2709662947833067, -338.2165204200192079 ) ) ;
#29837 = ORIENTED_EDGE ( 'NONE', *, *, #7143, .F. ) ;
#29838 = CARTESIAN_POINT ( 'NONE',  ( 762.1405469898971887, -409.5436935675101040, -357.8594530101015607 ) ) ;
#29839 = CARTESIAN_POINT ( 'NONE',  ( 756.5762568750052424, -99.18005720387478164, -348.7366044899774238 ) ) ;
#29840 = CARTESIAN_POINT ( 'NONE',  ( 756.7813123517142913, -259.9874144716869182, 329.9779781133712504 ) ) ;
#29841 = FACE_OUTER_BOUND ( 'NONE', #44283, .T. ) ;
#29842 = CARTESIAN_POINT ( 'NONE',  ( 914.9999999999992042, 99.99999999999984368, -350.0000000000000000 ) ) ;
#29843 = CLOSED_SHELL ( 'NONE', ( #21418, #35139, #7712, #29410, #22910, #29320, #21031, #26918, #23326, #34902, #24691 ) ) ;
#29844 = CARTESIAN_POINT ( 'NONE',  ( 811.3240766477731540, -4.372699936062523385, -355.6651683502462902 ) ) ;
#29845 = LINE ( 'NONE', #26149, #6965 ) ;
#29846 = ORIENTED_EDGE ( 'NONE', *, *, #34562, .F. ) ;
#29847 = CARTESIAN_POINT ( 'NONE',  ( 802.2119215644370342, -294.0090635724253048, -367.5423716828165084 ) ) ;
#29848 = CARTESIAN_POINT ( 'NONE',  ( 776.2046728542105711, -212.1908817542436623, 304.8212110874238761 ) ) ;
#29849 = VECTOR ( 'NONE', #28252, 1000.000000000000000 ) ;
#29851 = CARTESIAN_POINT ( 'NONE',  ( 804.9363028652555840, -280.2709662947833067, -338.2165204200192079 ) ) ;
#29850 = CARTESIAN_POINT ( 'NONE',  ( -37.63011601220122770, -513.1383975375929367, -349.9999999999999432 ) ) ;
#29852 = DIRECTION ( 'NONE',  ( 1.000000000000000000, 0.000000000000000000, 0.000000000000000000 ) ) ;
#29853 = CARTESIAN_POINT ( 'NONE',  ( 801.5560724626406000, -168.5545181178802352, -326.7756240680316182 ) ) ;
#29854 = LINE ( 'NONE', #19020, #11432 ) ;
#29856 = VECTOR ( 'NONE', #19859, 1000.000000000000114 ) ;
#29855 = CARTESIAN_POINT ( 'NONE',  ( 787.4397851343537695, -333.7255117493286320, -374.2001403089903988 ) ) ;
#29857 = CARTESIAN_POINT ( 'NONE',  ( 756.3353852180819104, -53.90732993114765037, 331.1735550268788302 ) ) ;
#29858 = AXIS2_PLACEMENT_3D ( 'NONE', #19356, #22818, #33442 ) ;
#29859 = CARTESIAN_POINT ( 'NONE',  ( 809.0717654672305343, -292.9181544815162397, 360.1688906516309885 ) ) ;
#29860 = CARTESIAN_POINT ( 'NONE',  ( 747.2067596250078623, -267.1800572038742985, 352.2312462859687230 ) ) ;
#29861 = CARTESIAN_POINT ( 'NONE',  ( 755.2512626584698410, 16.45630643248849267, -315.2512626584710915 ) ) ;
#29862 = EDGE_CURVE ( 'NONE', #36920, #12779, #3648, .T. ) ;
#29863 = FACE_OUTER_BOUND ( 'NONE', #41667, .T. ) ;
#29864 = VECTOR ( 'NONE', #790, 1000.000000000000000 ) ;
#29865 = CARTESIAN_POINT ( 'NONE',  ( 1820.038553321469863, -407.8586036264140375, 201.9999999999998863 ) ) ;
#29866 = CARTESIAN_POINT ( 'NONE',  ( 759.7806653035534055, -342.9982390220557136, 324.8639956371180801 ) ) ;
#29867 = CARTESIAN_POINT ( 'NONE',  ( 766.9102291470427417, -114.5545181178803631, 318.6633372737382501 ) ) ;
#29868 = CARTESIAN_POINT ( 'NONE',  ( 757.2208543904082489, -16.71468719896031985, -350.9844846989624330 ) ) ;
#29869 = CARTESIAN_POINT ( 'NONE',  ( 998.9999999999992042, 249.9999999999998863, -360.0000000000000000 ) ) ;
#29870 = PLANE ( 'NONE',  #41011 ) ;
#29871 = CARTESIAN_POINT ( 'NONE',  ( 803.6646147819161570, -401.9073299311463643, 348.8264449731210561 ) ) ;
#29872 = EDGE_LOOP ( 'NONE', ( #34257, #19720 ) ) ;
#29873 = VECTOR ( 'NONE', #44175, 1000.000000000000000 ) ;
#29874 = CARTESIAN_POINT ( 'NONE',  ( 776.9566956441375396, -324.8965053807775121, -364.8461984189686405 ) ) ;
#29875 = CARTESIAN_POINT ( 'NONE',  ( 758.0580252608178853, -150.4527844766018916, 328.0187753319985404 ) ) ;
#29876 = CIRCLE ( 'NONE', #18855, 19.99999999999990763 ) ;
#29877 = CARTESIAN_POINT ( 'NONE',  ( 805.9055244015594326, -315.6237781080503169, -315.8990559732753240 ) ) ;
#29878 = DIRECTION ( 'NONE',  ( -0.000000000000000000, -0.000000000000000000, 1.000000000000000000 ) ) ;
#29879 = ORIENTED_EDGE ( 'NONE', *, *, #44934, .T. ) ;
#29880 = CARTESIAN_POINT ( 'NONE',  ( 771.1735550268778070, -369.1800572038739574, 316.3353852180827630 ) ) ;
#29881 = VECTOR ( 'NONE', #10424, 1000.000000000000000 ) ;
#29882 = EDGE_LOOP ( 'NONE', ( #44647, #26690, #4245, #4943 ) ) ;
#29883 = CARTESIAN_POINT ( 'NONE',  ( 808.3070685750230950, -186.9982390220563104, -361.1904061080339261 ) ) ;
#29884 = CARTESIAN_POINT ( 'NONE',  ( 808.3070685750232087, -90.99823902205662307, 361.1904061080339829 ) ) ;
#29885 = ORIENTED_EDGE ( 'NONE', *, *, #31423, .F. ) ;
#29886 = CARTESIAN_POINT ( 'NONE',  ( 758.0580252608178853, -174.4527844766018063, -328.0187753319985404 ) ) ;
#29887 = VERTEX_POINT ( 'NONE', #20941 ) ;
#29888 = CARTESIAN_POINT ( 'NONE',  ( 755.3028492785439312, -423.2817908451521589, -335.9200461376539693 ) ) ;
#29889 = CIRCLE ( 'NONE', #35803, 8.024999999999948841 ) ;
#29890 = CARTESIAN_POINT ( 'NONE',  ( 804.7487373415286811, -259.5436935675106156, 364.7487373415288516 ) ) ;
#29891 = CARTESIAN_POINT ( 'NONE',  ( 793.2243759319678702, -170.5328690171416781, 318.4439275373583200 ) ) ;
#29893 = DIRECTION ( 'NONE',  ( 1.000000000000000000, 0.000000000000000000, -0.000000000000000000 ) ) ;
#29892 = CYLINDRICAL_SURFACE ( 'NONE', #45445, 2.749999999999863665 ) ;
#29894 = CIRCLE ( 'NONE', #18840, 8.024999999999948841 ) ;
#29895 = ORIENTED_EDGE ( 'NONE', *, *, #8337, .F. ) ;
#29896 = CARTESIAN_POINT ( 'NONE',  ( 772.4468031744293057, -417.8272453906067199, -363.8651313633793620 ) ) ;
#29897 = DIRECTION ( 'NONE',  ( 0.000000000000000000, 0.000000000000000000, 1.000000000000000000 ) ) ;
#29898 = ORIENTED_EDGE ( 'NONE', *, *, #2930, .F. ) ;
#29899 = CARTESIAN_POINT ( 'NONE',  ( 814.2805881961230625, -193.6454272087891582, -331.2368401574024119 ) ) ;
#29900 = CARTESIAN_POINT ( 'NONE',  ( 754.3581564841646241, -113.4636090269712554, 316.1443688327762516 ) ) ;
#29902 = CARTESIAN_POINT ( 'NONE',  ( 800.0135310231082713, -182.0891481129654323, -325.0180583372163028 ) ) ;
#29901 = DIRECTION ( 'NONE',  ( -0.000000000000000000, 1.000000000000000000, -0.000000000000000000 ) ) ;
#29903 = CARTESIAN_POINT ( 'NONE',  ( 794.1144889064781864, -346.1692326535047641, -360.9840315886528401 ) ) ;
#29904 = DIRECTION ( 'NONE',  ( -0.000000000000000000, 1.000000000000000000, -0.000000000000000000 ) ) ;
#29905 = CARTESIAN_POINT ( 'NONE',  ( 757.7880784355613741, -234.0090635724255037, -312.4576283171834916 ) ) ;
#29906 = DIRECTION ( 'NONE',  ( 1.000000000000000000, 0.000000000000000000, 0.000000000000000000 ) ) ;
#29907 = FACE_BOUND ( 'NONE', #12521, .T. ) ;
#29908 = CARTESIAN_POINT ( 'NONE',  ( 758.4439275373578084, -60.55451811788051941, -353.2243759319684386 ) ) ;
#29909 = CARTESIAN_POINT ( 'NONE',  ( 769.9779781133707957, -403.0999726633339719, 316.7813123517150871 ) ) ;
#29910 = EDGE_CURVE ( 'NONE', #14643, #10014, #10675, .T. ) ;
#29911 = VECTOR ( 'NONE', #18466, 1000.000000000000000 ) ;
#29912 = CARTESIAN_POINT ( 'NONE',  ( 808.3070685750232087, -258.9982390220561115, -361.1904061080339829 ) ) ;
#29913 = CARTESIAN_POINT ( 'NONE',  ( 766.9102291470427417, -234.5545181178799794, 318.6633372737382501 ) ) ;
#29914 = DIRECTION ( 'NONE',  ( 0.000000000000000000, -0.3826834323650838976, -0.9238795325112892920 ) ) ;
#29915 = DIRECTION ( 'NONE',  ( 0.000000000000000000, -0.000000000000000000, 1.000000000000000000 ) ) ;
#29916 = CARTESIAN_POINT ( 'NONE',  ( 758.0580252608178853, -54.45278447660219001, -328.0187753319985404 ) ) ;
#29917 = CARTESIAN_POINT ( 'NONE',  ( 781.2370466360911223, -188.7363362996983085, 304.9990715423533629 ) ) ;
#29918 = CARTESIAN_POINT ( 'NONE',  ( 776.2433038121456548, -132.8965053807781374, -374.8207195650711014 ) ) ;
#29919 = CARTESIAN_POINT ( 'NONE',  ( 808.3070685750230950, -138.9982390220563957, 361.1904061080339261 ) ) ;
#29920 = CARTESIAN_POINT ( 'NONE',  ( 763.2262854647970016, -368.6346026584193964, -309.2812353651462445 ) ) ;
#29921 = AXIS2_PLACEMENT_3D ( 'NONE', #14235, #28304, #34784 ) ;
#29922 = CARTESIAN_POINT ( 'NONE',  ( 441.1634899080286232, 259.9999999999999432, -193.8809999999972433 ) ) ;
#29923 = CARTESIAN_POINT ( 'NONE',  ( 755.0636971347428243, -244.2709662947834204, 341.7834795799807353 ) ) ;
#29924 = CARTESIAN_POINT ( 'NONE',  ( 755.1538015810308480, -38.19088175424422360, 343.0433043558613804 ) ) ;
#29925 = CARTESIAN_POINT ( 'NONE',  ( 764.8639956371174549, -392.0891481129648355, -319.7806653035542013 ) ) ;
#29926 = AXIS2_PLACEMENT_3D ( 'NONE', #25506, #17680, #35903 ) ;
#29927 = LINE ( 'NONE', #2201, #38716 ) ;
#29928 = CARTESIAN_POINT ( 'NONE',  ( 788.6739635108323228, -7.645427208789786100, -373.9316612368139090 ) ) ;
#29929 = LINE ( 'NONE', #30155, #21020 ) ;
#29930 = CARTESIAN_POINT ( 'NONE',  ( 793.2243759319678702, -74.53286901714196233, 318.4439275373583200 ) ) ;
#29931 = EDGE_LOOP ( 'NONE', ( #24939, #4615 ) ) ;
#29932 =( REPRESENTATION_RELATIONSHIP ('NONE','NONE', #39835, #28315 ) REPRESENTATION_RELATIONSHIP_WITH_TRANSFORMATION ( #45703 )SHAPE_REPRESENTATION_RELATIONSHIP( ) );
#29933 = CARTESIAN_POINT ( 'NONE',  ( 759.2295555964440155, -232.1692326535051620, -353.9708237608231229 ) ) ;
#29934 = CARTESIAN_POINT ( 'NONE',  ( 800.2193346964447755, -66.99823902205672255, 355.1360043628815788 ) ) ;
#29935 = CARTESIAN_POINT ( 'NONE',  ( 810.1134526219336749, -224.5328690171415076, -357.8822607201570349 ) ) ;
#29936 = CARTESIAN_POINT ( 'NONE',  ( 181.1634899080285948, 256.5000000000000000, -193.8809999999953959 ) ) ;
#29937 = CARTESIAN_POINT ( 'NONE',  ( 791.1614460488616487, -347.2601417444138860, 373.5763878283158874 ) ) ;
#29938 = EDGE_LOOP ( 'NONE', ( #30963, #23413, #43792, #25335 ) ) ;
#29939 = CARTESIAN_POINT ( 'NONE',  ( 785.3141322388236176, -141.7255117493291721, -364.4286716492789537 ) ) ;
#29940 = CARTESIAN_POINT ( 'NONE',  ( 754.8072714833581358, -364.8164208402374697, 338.1981804954720587 ) ) ;
#29941 = CARTESIAN_POINT ( 'NONE',  ( 763.2262854647970016, -80.63460265842029173, -309.2812353651462445 ) ) ;
#29942 = CARTESIAN_POINT ( 'NONE',  ( 774.6858677611749044, -81.72551174932937101, -315.5713283507209894 ) ) ;
#29943 = ORIENTED_EDGE ( 'NONE', *, *, #42215, .T. ) ;
#29944 = CARTESIAN_POINT ( 'NONE',  ( 790.0220218866281812, -7.099972663335241130, -363.2186876482849129 ) ) ;
#29945 = AXIS2_PLACEMENT_3D ( 'NONE', #10240, #27120, #38423 ) ;
#29946 = EDGE_LOOP ( 'NONE', ( #31349, #16480, #43812, #27509 ) ) ;
#29947 = CARTESIAN_POINT ( 'NONE',  ( 796.1575198192839480, -318.0090635724251911, -359.4546378042384163 ) ) ;
#29949 = CARTESIAN_POINT ( 'NONE',  ( 802.9823548866075953, -409.0999726633340288, 330.0799878456151077 ) ) ;
#29948 = CARTESIAN_POINT ( 'NONE',  ( 802.1676090361156639, -110.6346026584201638, 327.8955696845344505 ) ) ;
#29950 = VECTOR ( 'NONE', #3339, 1000.000000000000000 ) ;
#29951 = AXIS2_PLACEMENT_3D ( 'NONE', #3837, #18167, #18612 ) ;
#29954 = CARTESIAN_POINT ( 'NONE',  ( 744.8212110874229666, -330.8965053807774552, 336.2046728542121627 ) ) ;
#29953 = CARTESIAN_POINT ( 'NONE',  ( -521.6730038022808458, 200.0000000000001421, -122.7905160835438068 ) ) ;
#29952 = CARTESIAN_POINT ( 'NONE',  ( 767.7687537140311633, -431.9073299311464211, 372.7932403749916830 ) ) ;
#29955 = CARTESIAN_POINT ( 'NONE',  ( 758.4439275373578084, -324.5545181178796952, -353.2243759319684386 ) ) ;
#29956 = CARTESIAN_POINT ( 'NONE',  ( 757.8323909638827445, -338.6346026584195101, -352.1044303154654358 ) ) ;
#29957 = CARTESIAN_POINT ( 'NONE',  ( 764.8639956371174549, -152.0891481129655460, -319.7806653035542013 ) ) ;
#29958 = CARTESIAN_POINT ( 'NONE',  ( 751.9810565676468741, -434.0891481129646081, 360.9747183278973921 ) ) ;
#29959 = AXIS2_PLACEMENT_3D ( 'NONE', #16826, #37133, #5734 ) ;
#29961 = DIRECTION ( 'NONE',  ( 0.000000000000000000, 0.6755902076156502511, 0.7372773368101330771 ) ) ;
#29960 = DIRECTION ( 'NONE',  ( 0.000000000000000000, 0.000000000000000000, 1.000000000000000000 ) ) ;
#29962 = CARTESIAN_POINT ( 'NONE',  ( 799.4546378042377910, -273.0783235625958696, -356.1575198192848006 ) ) ;
#29963 = CARTESIAN_POINT ( 'NONE',  ( 776.2046728542105711, -116.1908817542440033, -304.8212110874238761 ) ) ;
#29964 = CARTESIAN_POINT ( 'NONE',  ( -746.4999999999993179, -365.3551492539851893, -28.13243251470704109 ) ) ;
#29965 = CARTESIAN_POINT ( 'NONE',  ( -728.8365100919714905, 240.0000000000001990, -202.7499999999889440 ) ) ;
#29966 = VECTOR ( 'NONE', #1601, 1000.000000000000000 ) ;
#29967 = CARTESIAN_POINT ( 'NONE',  ( 799.2566176426618085, -312.0090635724251911, 324.0069404352559559 ) ) ;
#29968 = ORIENTED_EDGE ( 'NONE', *, *, #38186, .F. ) ;
#29969 = CARTESIAN_POINT ( 'NONE',  ( 755.8990559732751535, -275.4636090269708575, 365.9055244015606831 ) ) ;
#29970 = CARTESIAN_POINT ( 'NONE',  ( 808.3070685750232087, -138.9982390220564241, -361.1904061080339829 ) ) ;
#29971 = DIRECTION ( 'NONE',  ( 1.000000000000000000, 0.000000000000000000, 0.000000000000000000 ) ) ;
#29972 = CARTESIAN_POINT ( 'NONE',  ( 752.7379699480933368, -84.00906357242590161, 361.9858362298580232 ) ) ;
#29973 = CARTESIAN_POINT ( 'NONE',  ( 777.4774526936600978, -274.2709662947833067, -304.7301800767027657 ) ) ;
#29974 = CARTESIAN_POINT ( 'NONE',  ( 763.2262854647970016, -440.6346026584191122, -309.2812353651462445 ) ) ;
#29975 = CARTESIAN_POINT ( 'NONE',  ( 802.1676090361156639, -158.6346026584199933, 327.8955696845344505 ) ) ;
#29976 = ORIENTED_EDGE ( 'NONE', *, *, #151, .F. ) ;
#29977 = CARTESIAN_POINT ( 'NONE',  ( 807.5423716828161105, -345.0783235625956991, -362.2119215644372048 ) ) ;
#29978 = CARTESIAN_POINT ( 'NONE',  ( 751.9810565676468741, -74.08914811296577341, -360.9747183278973921 ) ) ;
#29979 = CARTESIAN_POINT ( 'NONE',  ( 758.4439275373578084, -12.55451811788067751, 353.2243759319684386 ) ) ;
#29980 = CARTESIAN_POINT ( 'NONE',  ( 748.9653473494363425, -338.6346026584195101, -356.9462024416521331 ) ) ;
#29981 = PLANE ( 'NONE',  #6986 ) ;
#29982 = CARTESIAN_POINT ( 'NONE',  ( 803.8651313633788504, -389.2601417444136018, 332.4468031744301015 ) ) ;
#29983 = ORIENTED_EDGE ( 'NONE', *, *, #12485, .F. ) ;
#29984 = AXIS2_PLACEMENT_3D ( 'NONE', #44436, #1940, #23171 ) ;
#29985 = CARTESIAN_POINT ( 'NONE',  ( 781.2497674668890113, -132.3510508353235764, -375.3608509340180603 ) ) ;
#29986 = LINE ( 'NONE', #19821, #19636 ) ;
#29987 = CARTESIAN_POINT ( 'NONE',  ( 807.5423716828161105, -249.0783235625959549, 362.2119215644372048 ) ) ;
#29988 = CARTESIAN_POINT ( 'NONE',  ( 755.0636971347428243, -100.2709662947838609, 341.7834795799807353 ) ) ;
#29989 = ORIENTED_EDGE ( 'NONE', *, *, #12563, .T. ) ;
#29990 = CARTESIAN_POINT ( 'NONE',  ( 805.0264073115434940, -6.351050835323991173, -339.4763451958999099 ) ) ;
#29991 = CARTESIAN_POINT ( 'NONE',  ( 759.7806653035534055, -246.9982390220560546, 324.8639956371180801 ) ) ;
#29992 = VECTOR ( 'NONE', #40137, 1000.000000000000000 ) ;
#29993 = CARTESIAN_POINT ( 'NONE',  ( 773.7943932421234194, -431.8055962898681059, -305.5313806188329409 ) ) ;
#29994 = DIRECTION ( 'NONE',  ( 1.000000000000000000, 0.000000000000000000, 0.000000000000000000 ) ) ;
#29995 = ORIENTED_EDGE ( 'NONE', *, *, #17132, .F. ) ;
#29996 = VERTEX_POINT ( 'NONE', #14259 ) ;
#29997 = CARTESIAN_POINT ( 'NONE',  ( 814.4686193811664907, -363.2817908451523294, -346.2056067578752732 ) ) ;
#29998 = CARTESIAN_POINT ( 'NONE',  ( 767.8955696845333705, -240.4527844766015221, -362.1676090361162323 ) ) ;
#29999 = CARTESIAN_POINT ( 'NONE',  ( 746.8695393053151292, -341.9073299311466485, 327.6429770376306578 ) ) ;
#30000 = EDGE_CURVE ( 'NONE', #36920, #2495, #28327, .T. ) ;
#30001 = CARTESIAN_POINT ( 'NONE',  ( 773.7943932421234194, -47.80559628986931386, 305.5313806188329409 ) ) ;
#30002 = CARTESIAN_POINT ( 'NONE',  ( 790.9844846989617508, -214.3726999360618493, -317.2208543904092721 ) ) ;
#30003 = CARTESIAN_POINT ( 'NONE',  ( 804.9363028652555840, -232.2709662947834488, -338.2165204200192079 ) ) ;
#30004 = CARTESIAN_POINT ( 'NONE',  ( 788.7366044899766848, -395.9073299311465348, -316.5762568750059813 ) ) ;
#30005 = ORIENTED_EDGE ( 'NONE', *, *, #19848, .T. ) ;
#30006 = CARTESIAN_POINT ( 'NONE',  ( 804.4286716492782716, -209.3618753856926276, 345.3141322388244703 ) ) ;
#30007 = CARTESIAN_POINT ( 'NONE',  ( 801.9419747391806368, -90.45278447660209054, -351.9812246680014027 ) ) ;
#30008 = ORIENTED_EDGE ( 'NONE', *, *, #4128, .T. ) ;
#30009 = CARTESIAN_POINT ( 'NONE',  ( 751.9810565676468741, -338.0891481129649492, 360.9747183278973921 ) ) ;
#30010 = CARTESIAN_POINT ( 'NONE',  ( -858.8365100919713768, 260.0000000000002274, -193.8809999999881768 ) ) ;
#30011 = DIRECTION ( 'NONE',  ( 1.000000000000000000, 0.000000000000000000, 0.000000000000000000 ) ) ;
#30012 = VECTOR ( 'NONE', #10361, 1000.000000000000000 ) ;
#30013 = DIRECTION ( 'NONE',  ( 0.000000000000000000, 0.000000000000000000, 1.000000000000000000 ) ) ;
#30014 = EDGE_CURVE ( 'NONE', #6928, #42899, #30900, .T. ) ;
#30015 = CARTESIAN_POINT ( 'NONE',  ( 800.9840315886518738, -196.9181544815164386, 354.1144889064786412 ) ) ;
#30016 = CARTESIAN_POINT ( 'NONE',  ( 756.5762568750052424, -99.18005720387478164, 348.7366044899774238 ) ) ;
#30017 = ORIENTED_EDGE ( 'NONE', *, *, #1266, .T. ) ;
#30018 = CARTESIAN_POINT ( 'NONE',  ( 814.2805881961230625, -457.6454272087884760, -331.2368401574024119 ) ) ;
#30019 = CARTESIAN_POINT ( 'NONE',  ( 812.7932403749906598, -39.18005720387496638, -327.7687537140311633 ) ) ;
#30020 = CARTESIAN_POINT ( 'NONE',  ( 794.1144889064781864, -250.1692326535050199, 360.9840315886528401 ) ) ;
#30021 = AXIS2_PLACEMENT_3D ( 'NONE', #34447, #38372, #3723 ) ;
#30022 = CARTESIAN_POINT ( 'NONE',  ( 785.3687786644884454, -395.3618753856918602, -315.3201227861279676 ) ) ;
#30023 = CARTESIAN_POINT ( 'NONE',  ( 757.8323909638828582, -2.634602658420536425, -352.1044303154654358 ) ) ;
#30024 = CARTESIAN_POINT ( 'NONE',  ( 777.5031285880264704, -430.8164208402374129, 374.9108240113588408 ) ) ;
#30025 = CARTESIAN_POINT ( 'NONE',  ( 795.2725662613897839, 16.45630643248849267, 314.1785221222716586 ) ) ;
#30026 = CARTESIAN_POINT ( 'NONE',  ( 755.1538015810308480, -302.1908817542433781, -343.0433043558613804 ) ) ;
#30027 = CARTESIAN_POINT ( 'NONE',  ( 751.6929314249748586, -150.9982390220563957, -318.8095938919659034 ) ) ;
#30028 = CIRCLE ( 'NONE', #25626, 10.00000000000000888 ) ;
#30029 = CARTESIAN_POINT ( 'NONE',  ( 777.5031285880264704, -46.81642084023858530, 374.9108240113588408 ) ) ;
#30030 = CARTESIAN_POINT ( 'NONE',  ( 763.2262854647970016, -152.6346026584200786, 309.2812353651462445 ) ) ;
#30031 = CARTESIAN_POINT ( 'NONE',  ( 794.6702036691820012, 16.45630643248850689, -314.5864782580647443 ) ) ;
#30032 = DIRECTION ( 'NONE',  ( 1.000000000000000000, 0.000000000000000000, 0.000000000000000000 ) ) ;
#30033 = EDGE_CURVE ( 'NONE', #38354, #8383, #32497, .T. ) ;
#30034 = EDGE_CURVE ( 'NONE', #12718, #44771, #29147, .T. ) ;
#30035 = CARTESIAN_POINT ( 'NONE',  ( -200.7583438952258916, 294.6698570112193920, -224.9999999999999716 ) ) ;
#30036 = CARTESIAN_POINT ( 'NONE',  ( 814.9108240113580450, -376.2709662947829656, 337.5031285880265273 ) ) ;
#30037 = CARTESIAN_POINT ( 'NONE',  ( 778.2165204200184689, -358.8164208402375834, -364.9363028652563230 ) ) ;
#30038 = CARTESIAN_POINT ( 'NONE',  ( 795.9930595647434757, 20.92167643740319605, 320.7433823573372820 ) ) ;
#30039 = EDGE_CURVE ( 'NONE', #23168, #9031, #847, .T. ) ;
#30040 = CARTESIAN_POINT ( 'NONE',  ( 807.2620300519052989, -96.00906357242585898, -318.0141637701419768 ) ) ;
#30041 = CARTESIAN_POINT ( 'NONE',  ( 784.0799538623451781, -131.8055962898690439, -364.6971507214555572 ) ) ;
#30042 = CARTESIAN_POINT ( 'NONE',  ( 813.2346286133761168, -149.2601417444144261, 328.9521613784389160 ) ) ;
#30043 = CARTESIAN_POINT ( 'NONE',  ( 804.6798772138710092, 8.274488250670337663, 334.6312213355106451 ) ) ;
#30044 = CARTESIAN_POINT ( 'NONE',  ( 793.4146539503750546, -169.9874144716871172, 307.6481478633938877 ) ) ;
#30045 = CARTESIAN_POINT ( 'NONE',  ( 804.6798772138708955, -39.72551174932951312, -334.6312213355107019 ) ) ;
#30046 = CARTESIAN_POINT ( 'NONE',  ( 755.8398074228967971, -115.4419599262327409, -333.4516893846970333 ) ) ;
#30047 = CARTESIAN_POINT ( 'NONE',  ( 788.8264449731200330, -117.1800572038746964, 363.6646147819171233 ) ) ;
#30048 = CARTESIAN_POINT ( 'NONE',  ( 805.9055244015594326, 20.37622189194865285, -315.8990559732753240 ) ) ;
#30050 = CARTESIAN_POINT ( 'NONE',  ( 771.1735550268780344, -273.1800572038742985, 316.3353852180828198 ) ) ;
#30049 = CARTESIAN_POINT ( 'NONE',  ( 774.6858677611749044, -297.7255117493286889, 315.5713283507209894 ) ) ;
#30051 = PLANE ( 'NONE',  #13851 ) ;
#30052 = VERTEX_POINT ( 'NONE', #28580 ) ;
#30053 = CARTESIAN_POINT ( 'NONE',  ( 765.8855110935204493, 1.830767346494167391, 319.0159684113471599 ) ) ;
#30054 = CARTESIAN_POINT ( 'NONE',  ( 810.4231160770870019, -288.5545181178798657, -321.9338519418446936 ) ) ;
#30055 = VECTOR ( 'NONE', #19941, 1000.000000000000000 ) ;
#30056 = EDGE_CURVE ( 'NONE', #17152, #34249, #35035, .T. ) ;
#30057 = ORIENTED_EDGE ( 'NONE', *, *, #6661, .T. ) ;
#30058 = CARTESIAN_POINT ( 'NONE',  ( 0.000000000000000000, 0.000000000000000000, 0.000000000000000000 ) ) ;
#30059 = CARTESIAN_POINT ( 'NONE',  ( 804.7487373415286811, -235.5436935675107293, 364.7487373415288516 ) ) ;
#30060 = EDGE_CURVE ( 'NONE', #17397, #34100, #11486, .T. ) ;
#30061 = CARTESIAN_POINT ( 'NONE',  ( 780.5236548040995785, -284.7363362996979390, 314.9735926884559944 ) ) ;
#30062 = CARTESIAN_POINT ( 'NONE',  ( 786.6156483768007774, -409.4419599262317320, 315.5913626894246136 ) ) ;
#30063 = EDGE_LOOP ( 'NONE', ( #32664, #13475 ) ) ;
#30064 = CARTESIAN_POINT ( 'NONE',  ( 796.1575198192839480, -126.0090635724257737, -359.4546378042384163 ) ) ;
#30065 = CARTESIAN_POINT ( 'NONE',  ( 771.2633955100217236, -119.9073299311474443, -363.4237431249939618 ) ) ;
#30066 = CARTESIAN_POINT ( 'NONE',  ( 768.0187753319979720, -296.6346026584195670, -318.0580252608186242 ) ) ;
#30067 = VERTEX_POINT ( 'NONE', #18418 ) ;
#30068 = CARTESIAN_POINT ( 'NONE',  ( 756.3353852180819104, -413.9073299311465348, -331.1735550268788302 ) ) ;
#30069 = CARTESIAN_POINT ( 'NONE',  ( 759.9864689768902508, -74.08914811296577341, -354.9819416627836404 ) ) ;
#30070 = CARTESIAN_POINT ( 'NONE',  ( 805.1016975059191054, -294.8965053807775689, 343.0745993439771837 ) ) ;
#30071 = EDGE_CURVE ( 'NONE', #41324, #18090, #39440, .T. ) ;
#30072 = DIRECTION ( 'NONE',  ( 0.000000000000000000, -6.938893903907222461E-16, 1.000000000000000000 ) ) ;
#30073 = DIRECTION ( 'NONE',  ( 0.000000000000000000, 0.000000000000000000, 1.000000000000000000 ) ) ;
#30074 = EDGE_CURVE ( 'NONE', #37455, #24474, #43859, .T. ) ;
#30075 = DIRECTION ( 'NONE',  ( -0.000000000000000000, 1.000000000000000000, -0.000000000000000000 ) ) ;
#30076 = ORIENTED_EDGE ( 'NONE', *, *, #14334, .F. ) ;
#30077 = CARTESIAN_POINT ( 'NONE',  ( 797.8822607201568644, -342.5545181178796952, -370.1134526219340160 ) ) ;
#30078 = CARTESIAN_POINT ( 'NONE',  ( 744.6391490659812007, -206.7363362996982801, 338.7502325331110455 ) ) ;
#30080 = CARTESIAN_POINT ( 'NONE',  ( 795.1360043628807261, -284.0891481129650629, -360.2193346964456282 ) ) ;
#30079 = CARTESIAN_POINT ( 'NONE',  ( 784.4999999999993179, -501.1515549466498669, -368.0974687824633520 ) ) ;
#30081 =( LENGTH_UNIT ( ) NAMED_UNIT ( * ) SI_UNIT ( .MILLI., .METRE. ) );
#30082 = CARTESIAN_POINT ( 'NONE',  ( 804.1105419155481968, -195.8272453906074304, -347.6308680596136469 ) ) ;
#30083 = CARTESIAN_POINT ( 'NONE',  ( 772.5602148656447525, -33.72551174932952733, 305.7998596910095443 ) ) ;
#30084 = DIRECTION ( 'NONE',  ( -0.000000000000000000, -0.6755902076156505842, -0.7372773368101327440 ) ) ;
#30085 = CARTESIAN_POINT ( 'NONE',  ( 812.7932403749906598, -375.1800572038739574, -327.7687537140311633 ) ) ;
#30086 = CARTESIAN_POINT ( 'NONE',  ( 762.3223304703356007, -55.54369356751127640, 322.3223304703362828 ) ) ;
#30087 = AXIS2_PLACEMENT_3D ( 'NONE', #20615, #34710, #3068 ) ;
#30088 = CARTESIAN_POINT ( 'NONE',  ( 762.1177392798416577, -306.5545181178797520, 309.8865473780659272 ) ) ;
#30089 = EDGE_CURVE ( 'NONE', #757, #42387, #25096, .T. ) ;
#30090 = CARTESIAN_POINT ( 'NONE',  ( 777.4774526936600978, -250.2709662947832783, 304.7301800767027657 ) ) ;
#30091 = CARTESIAN_POINT ( 'NONE',  ( 763.0537975583475827, -24.45278447660229304, -371.0346526505627480 ) ) ;
#30092 = DIRECTION ( 'NONE',  ( -1.880165489482579047E-16, -1.000000000000000000, 0.000000000000000000 ) ) ;
#30093 = CARTESIAN_POINT ( 'NONE',  ( 794.9999999999993179, 212.6707680665973612, -236.5295014342203785 ) ) ;
#30094 = CARTESIAN_POINT ( 'NONE',  ( 792.1044303154645831, -372.4527844766010958, 317.8323909638837677 ) ) ;
#30095 = CARTESIAN_POINT ( 'NONE',  ( 775.8780910478218402, -129.2817908451530400, 364.9511171171680530 ) ) ;
#30096 = CARTESIAN_POINT ( 'NONE',  ( 801.3366627262608972, -8.532869017142163059, -353.0897708529566899 ) ) ;
#30097 = CARTESIAN_POINT ( 'NONE',  ( -28.63011601220122415, -110.5936016518799221, 750.6326042729449455 ) ) ;
#30098 = DIRECTION ( 'NONE',  ( 0.000000000000000000, 0.000000000000000000, -1.000000000000000000 ) ) ;
#30099 = CARTESIAN_POINT ( 'NONE',  ( 756.5762568750052424, -411.1800572038738437, 348.7366044899774238 ) ) ;
#30100 = VERTEX_POINT ( 'NONE', #39210 ) ;
#30101 = CARTESIAN_POINT ( 'NONE',  ( 756.1348686366196716, -329.2601417444138860, -347.5531968255698416 ) ) ;
#30103 = CARTESIAN_POINT ( 'NONE',  ( 803.6646147819162707, -161.9073299311472738, 348.8264449731211130 ) ) ;
#30102 = CARTESIAN_POINT ( 'NONE',  ( 754.8072714833581358, -172.8164208402381234, 338.1981804954720587 ) ) ;
#30104 = UNCERTAINTY_MEASURE_WITH_UNIT (LENGTH_MEASURE( 1.000000000000000082E-05 ), #24309, 'distance_accuracy_value', 'NONE');
#30105 = CARTESIAN_POINT ( 'NONE',  ( 815.1787889125755555, -342.8965053807773984, -343.7953271457877804 ) ) ;
#30106 = DIRECTION ( 'NONE',  ( 0.000000000000000000, 1.000000000000000000, 0.000000000000000000 ) ) ;
#30107 = EDGE_LOOP ( 'NONE', ( #25951, #4724, #35178, #13878, #29046, #15253, #40644, #45526 ) ) ;
#30108 = CARTESIAN_POINT ( 'NONE',  ( 774.6858677611749044, -345.7255117493285184, 315.5713283507209894 ) ) ;
#30109 = EDGE_CURVE ( 'NONE', #1931, #15194, #10799, .T. ) ;
#30110 = ORIENTED_EDGE ( 'NONE', *, *, #45522, .F. ) ;
#30111 = CARTESIAN_POINT ( 'NONE',  ( 777.4774526936600978, -178.2709662947835625, -304.7301800767027657 ) ) ;
#30112 = CARTESIAN_POINT ( 'NONE',  ( 772.5602148656447525, -105.7255117493293000, 305.7998596910095443 ) ) ;
#30113 = ADVANCED_FACE ( 'NONE', ( #25784 ), #13647, .F. ) ;
#30114 = ORIENTED_EDGE ( 'NONE', *, *, #30071, .F. ) ;
#30115 = CARTESIAN_POINT ( 'NONE',  ( 788.8264449731201466, -165.1800572038745543, -363.6646147819170665 ) ) ;
#30116 = ORIENTED_EDGE ( 'NONE', *, *, #40773, .F. ) ;
#30117 = CIRCLE ( 'NONE', #20558, 8.024999999999948841 ) ;
#30118 = CARTESIAN_POINT ( 'NONE',  ( 758.4439275373578084, -444.5545181178792973, -353.2243759319684386 ) ) ;
#30119 = CARTESIAN_POINT ( 'NONE',  ( 772.4837098697144029, -263.3618753856924855, 374.5518280994205611 ) ) ;
#30120 = CARTESIAN_POINT ( 'NONE',  ( 755.8398074228967971, -211.4419599262324709, 333.4516893846970333 ) ) ;
#30122 = CARTESIAN_POINT ( 'NONE',  ( 779.9999999999992042, -452.9681489794448339, 309.9999999999998863 ) ) ;
#30121 = PLANE ( 'NONE',  #38054 ) ;
#30123 = ORIENTED_EDGE ( 'NONE', *, *, #24975, .T. ) ;
#30124 = CARTESIAN_POINT ( 'NONE',  ( 758.4439275373578084, -420.5545181178793541, -353.2243759319684386 ) ) ;
#30125 = DIRECTION ( 'NONE',  ( 1.000000000000000000, 0.000000000000000000, -0.000000000000000000 ) ) ;
#30126 = ORIENTED_EDGE ( 'NONE', *, *, #43588, .F. ) ;
#30127 = CARTESIAN_POINT ( 'NONE',  ( 755.8990559732751535, -227.4636090269709143, -365.9055244015606831 ) ) ;
#30128 = CARTESIAN_POINT ( 'NONE',  ( 791.0478386215596629, -117.8272453906076151, 306.7653713866226326 ) ) ;
#30130 = CARTESIAN_POINT ( 'NONE',  ( 778.1981804954714335, -178.2709662947835625, -314.8072714833589885 ) ) ;
#30129 = LINE ( 'NONE', #19275, #27829 ) ;
#30131 = CARTESIAN_POINT ( 'NONE',  ( 796.7845633553578182, -345.6237781080501463, -358.5707757039688204 ) ) ;
#30132 = LINE ( 'NONE', #17591, #6255 ) ;
#30133 = CARTESIAN_POINT ( 'NONE',  ( 781.2370466360911223, -236.7363362996981380, -304.9990715423533629 ) ) ;
#30134 = DIRECTION ( 'NONE',  ( -0.000000000000000000, 1.000000000000000000, -0.000000000000000000 ) ) ;
#30135 = DIRECTION ( 'NONE',  ( -0.000000000000000000, -1.000000000000000000, -0.000000000000000000 ) ) ;
#30136 = CARTESIAN_POINT ( 'NONE',  ( 802.9823548866075953, -49.09997266333511590, -330.0799878456151077 ) ) ;
#30137 = CARTESIAN_POINT ( 'NONE',  ( 755.8894580844503253, -423.8272453906067199, 332.3691319403863531 ) ) ;
#30138 = CARTESIAN_POINT ( 'NONE',  ( 812.3518521366052028, -361.0999726633341425, 326.5853460496235243 ) ) ;
#30139 = CARTESIAN_POINT ( 'NONE',  ( 757.2208543904082489, -424.7146871989589840, -350.9844846989624330 ) ) ;
#30140 = CARTESIAN_POINT ( 'NONE',  ( 800.9747183278959710, -276.9982390220559978, -311.9810565676471583 ) ) ;
#30141 = CYLINDRICAL_SURFACE ( 'NONE', #4730, 1.000000000000000888 ) ;
#30142 = CARTESIAN_POINT ( 'NONE',  ( 779.9999999999992042, -462.9681489794448339, 370.0000000000000568 ) ) ;
#30143 = CARTESIAN_POINT ( 'NONE',  ( 803.4237431249931660, -63.18005720387488822, -331.2633955100225194 ) ) ;
#30144 = CARTESIAN_POINT ( 'NONE',  ( 814.4686193811664907, -171.2817908451529263, 346.2056067578752732 ) ) ;
#30145 = CARTESIAN_POINT ( 'NONE',  ( 752.4576283171824116, -141.0783235625962959, -317.7880784355627952 ) ) ;
#30146 = CARTESIAN_POINT ( 'NONE',  ( 763.0537975583475827, -144.4527844766018632, 371.0346526505627480 ) ) ;
#30147 = CARTESIAN_POINT ( 'NONE',  ( 751.9810565676468741, -386.0891481129647786, -360.9747183278973921 ) ) ;
#30148 = CARTESIAN_POINT ( 'NONE',  ( 759.9999999999992042, -462.9681489794448339, -317.6393202250019954 ) ) ;
#30149 = CARTESIAN_POINT ( 'NONE',  ( 764.8639956371174549, -248.0891481129651481, 319.7806653035542013 ) ) ;
#30150 = CARTESIAN_POINT ( 'NONE',  ( 759.0159684113467620, -40.91815448151695023, 325.8855110935213020 ) ) ;
#30151 = CARTESIAN_POINT ( 'NONE',  ( 756.3353852180819104, -389.9073299311465348, -331.1735550268788302 ) ) ;
#30152 = VECTOR ( 'NONE', #4094, 1000.000000000000000 ) ;
#30153 = CARTESIAN_POINT ( 'NONE',  ( 571.1634899080285095, 239.9999999999999716, -199.9999999999981526 ) ) ;
#30154 = CARTESIAN_POINT ( 'NONE',  ( 745.5313806188320314, -39.28179084515331709, -333.7943932421247268 ) ) ;
#30155 = CARTESIAN_POINT ( 'NONE',  ( 799.9999999999993179, -512.9681489794448908, -350.0000000000000000 ) ) ;
#30156 = CARTESIAN_POINT ( 'NONE',  ( 801.3366627262608972, -80.53286901714194812, 353.0897708529566899 ) ) ;
#30157 = ORIENTED_EDGE ( 'NONE', *, *, #16185, .T. ) ;
#30158 = CARTESIAN_POINT ( 'NONE',  ( 763.2154366446407039, -213.6237781080506011, -321.4292242960311228 ) ) ;
#30159 = CARTESIAN_POINT ( 'NONE',  ( 754.8072714833581358, -52.81642084023856398, 338.1981804954720587 ) ) ;
#30160 = CARTESIAN_POINT ( 'NONE',  ( 749.8865473780648472, -236.5328690171414792, -322.1177392798429082 ) ) ;
#30161 = FACE_BOUND ( 'NONE', #32918, .T. ) ;
#30162 = CARTESIAN_POINT ( 'NONE',  ( 754.0944755984390895, -375.6237781080501463, 364.1009440267246760 ) ) ;
#30163 = VERTEX_POINT ( 'NONE', #32962 ) ;
#30164 = CARTESIAN_POINT ( 'NONE',  ( 756.3353852180819104, -269.9073299311468190, 331.1735550268788302 ) ) ;
#30165 = CARTESIAN_POINT ( 'NONE',  ( 747.2067596250078623, -3.180057203875080063, 352.2312462859687230 ) ) ;
#30166 = CARTESIAN_POINT ( 'NONE',  ( 756.3353852180819104, -173.9073299311472169, -331.1735550268788302 ) ) ;
#30167 = CARTESIAN_POINT ( 'NONE',  ( 757.8323909638827445, -362.6346026584194533, 352.1044303154654358 ) ) ;
#30168 = CARTESIAN_POINT ( 'NONE',  ( 777.5031285880264704, -70.81642084023850714, -374.9108240113588408 ) ) ;
#30169 = CARTESIAN_POINT ( 'NONE',  ( 791.9812246680005501, -68.63460265842033436, -361.9419747391813189 ) ) ;
#30170 = ORIENTED_EDGE ( 'NONE', *, *, #18455, .F. ) ;
#30171 = CARTESIAN_POINT ( 'NONE',  ( 755.1538015810308480, -14.19088175424431242, -343.0433043558613804 ) ) ;
#30172 = EDGE_LOOP ( 'NONE', ( #15226, #21142, #2365, #33577, #31995, #20003 ) ) ;
#30173 = CARTESIAN_POINT ( 'NONE',  ( 779.4763451958990572, -368.7363362996977685, -365.0264073115438919 ) ) ;
#30175 = CARTESIAN_POINT ( 'NONE',  ( 796.1575198192839480, -390.0090635724249069, 359.4546378042384163 ) ) ;
#30174 = CARTESIAN_POINT ( 'NONE',  ( 788.8264449731200330, -93.18005720387481006, 363.6646147819171233 ) ) ;
#30178 = CARTESIAN_POINT ( 'NONE',  ( 793.4146539503750546, -337.9874144716865771, 307.6481478633938877 ) ) ;
#30177 = CARTESIAN_POINT ( 'NONE',  ( 51.16348990802859475, 260.0000000000000568, -199.9999999999945146 ) ) ;
#30176 = CARTESIAN_POINT ( 'NONE',  ( 796.9462024416508257, -420.4527844766009821, 308.9653473494370246 ) ) ;
#30179 = CARTESIAN_POINT ( 'NONE',  ( 752.4576283171824116, -93.07832356259645223, 317.7880784355627952 ) ) ;
#30180 = CARTESIAN_POINT ( 'NONE',  ( 804.4086373105744769, -337.6454272087888171, -333.3843516231986541 ) ) ;
#30181 = CARTESIAN_POINT ( 'NONE',  ( 759.7806653035534055, -318.9982390220557704, -324.8639956371180801 ) ) ;
#30182 = CARTESIAN_POINT ( 'NONE',  ( 781.7834795799800531, -154.8164208402382371, -315.0636971347436202 ) ) ;
#30183 = CIRCLE ( 'NONE', #5826, 10.00000000000000888 ) ;
#30184 = CARTESIAN_POINT ( 'NONE',  ( 793.3938497862117174, -453.0432664090020012, 372.3358127763067955 ) ) ;
#30186 = LINE ( 'NONE', #19336, #28550 ) ;
#30185 = LINE ( 'NONE', #33878, #35907 ) ;
#30187 = CARTESIAN_POINT ( 'NONE',  ( 776.9566956441375396, -276.8965053807776258, -364.8461984189686405 ) ) ;
#30188 = CARTESIAN_POINT ( 'NONE',  ( 746.4236121716829757, -135.8272453906076009, -328.8385539511384650 ) ) ;
#30189 = CARTESIAN_POINT ( 'NONE',  ( 789.7124813865536908, -452.9681489794450613, 363.0370378529873960 ) ) ;
#30190 = LINE ( 'NONE', #13558, #1647 ) ;
#30191 = CARTESIAN_POINT ( 'NONE',  ( 800.9840315886518738, -340.9181544815160123, 354.1144889064786412 ) ) ;
#30192 = CARTESIAN_POINT ( 'NONE',  ( 803.4237431249931660, -183.1800572038744974, 331.2633955100225194 ) ) ;
#30193 = EDGE_LOOP ( 'NONE', ( #6238, #749, #39855, #36647, #3776, #45699 ) ) ;
#30194 = CARTESIAN_POINT ( 'NONE',  ( 776.2046728542105711, -284.1908817542434917, 304.8212110874238761 ) ) ;
#30195 = CARTESIAN_POINT ( 'NONE',  ( 754.9967657858570647, -145.5436935675109851, -365.0032342141425943 ) ) ;
#30196 = CARTESIAN_POINT ( 'NONE',  ( 758.9356612065449781, 18.10977687916123813, -318.6379319222613731 ) ) ;
#30197 = CARTESIAN_POINT ( 'NONE',  ( 814.2805881961230625, -73.64542720878957027, 331.2368401574024119 ) ) ;
#30198 = CARTESIAN_POINT ( 'NONE',  ( 805.0032342141412300, -253.5436935675104735, -314.9967657858571783 ) ) ;
#30199 = DIRECTION ( 'NONE',  ( -0.000000000000000000, 1.000000000000000000, -0.000000000000000000 ) ) ;
#30200 = APPLICATION_CONTEXT ( 'automotive_design' ) ;
#30201 = CARTESIAN_POINT ( 'NONE',  ( 797.8594530101008786, -157.5436935675108998, 322.1405469898980982 ) ) ;
#30202 = ORIENTED_EDGE ( 'NONE', *, *, #24944, .T. ) ;
#30203 = CARTESIAN_POINT ( 'NONE',  ( 776.2433038121456548, -324.8965053807775121, -374.8207195650711014 ) ) ;
#30204 = CARTESIAN_POINT ( 'NONE',  ( 745.7998596910086917, -101.3618753856929544, -332.5602148656461168 ) ) ;
#30205 = CARTESIAN_POINT ( 'NONE',  ( 755.8894580844503253, -15.82724539060794200, 332.3691319403863531 ) ) ;
#30206 = CARTESIAN_POINT ( 'NONE',  ( 763.0537975583475827, -336.4527844766012095, -371.0346526505627480 ) ) ;
#30207 = CARTESIAN_POINT ( 'NONE',  ( 989.9999999999992042, -416.7569064942979935, -212.5753187112032947 ) ) ;
#30208 = CARTESIAN_POINT ( 'NONE',  ( 754.8983024940795303, -426.8965053807771142, 336.9254006560228163 ) ) ;
#30209 = VERTEX_POINT ( 'NONE', #35960 ) ;
#30210 = CARTESIAN_POINT ( 'NONE',  ( 781.2497674668890113, -108.3510508353236759, -375.3608509340180603 ) ) ;
#30211 = LINE ( 'NONE', #23498, #44706 ) ;
#30212 = CARTESIAN_POINT ( 'NONE',  ( 808.7758568127978833, -268.1692326535049347, 320.0363995740631822 ) ) ;
#30213 = CARTESIAN_POINT ( 'NONE',  ( 755.0636971347428243, -76.27096629478394618, 341.7834795799807353 ) ) ;
#30214 = AXIS2_PLACEMENT_3D ( 'NONE', #26869, #6775, #34949 ) ;
#30215 = ORIENTED_EDGE ( 'NONE', *, *, #17684, .T. ) ;
#30216 = VERTEX_POINT ( 'NONE', #17956 ) ;
#30217 = CARTESIAN_POINT ( 'NONE',  ( 772.3691319403857278, 0.7398582555850804487, -315.8894580844506663 ) ) ;
#30218 = CARTESIAN_POINT ( 'NONE',  ( 794.9819416627830151, -276.9982390220559978, 319.9864689768909898 ) ) ;
#30219 = CARTESIAN_POINT ( 'NONE',  ( 771.2368401574024119, -421.4419599262317888, -374.2805881961240857 ) ) ;
#30220 = CARTESIAN_POINT ( 'NONE',  ( 927.9999999999992042, 154.9999999999998863, 360.0000000000000000 ) ) ;
#30221 = EDGE_LOOP ( 'NONE', ( #37587, #24412, #17331, #21600 ) ) ;
#30222 = CARTESIAN_POINT ( 'NONE',  ( 745.5313806188320314, -375.2817908451523294, -333.7943932421247268 ) ) ;
#30224 = CARTESIAN_POINT ( 'NONE',  ( 771.2368401574024119, -229.4419599262323572, 374.2805881961240857 ) ) ;
#30223 = CARTESIAN_POINT ( 'NONE',  ( 787.4397851343537695, -309.7255117493287457, 374.2001403089903988 ) ) ;
#30225 = CARTESIAN_POINT ( 'NONE',  ( 812.6845335610512393, -31.98741447168754348, 353.5525998758768651 ) ) ;
#30226 = CARTESIAN_POINT ( 'NONE',  ( 766.0291762391763086, -202.9181544815164386, -360.7704444035551319 ) ) ;
#30227 = CARTESIAN_POINT ( 'NONE',  ( 764.8639956371174549, -224.0891481129653187, -319.7806653035542013 ) ) ;
#30228 = CARTESIAN_POINT ( 'NONE',  ( 801.9419747391806368, -402.4527844766010389, -351.9812246680014027 ) ) ;
#30229 = VERTEX_POINT ( 'NONE', #21637 ) ;
#30230 = CARTESIAN_POINT ( 'NONE',  ( 774.6312213355099630, -215.3618753856925423, 364.6798772138717482 ) ) ;
#30231 = CARTESIAN_POINT ( 'NONE',  ( 759.9864689768902508, -98.08914811296568814, -354.9819416627836404 ) ) ;
#30232 = ORIENTED_EDGE ( 'NONE', *, *, #34849, .F. ) ;
#30233 = CARTESIAN_POINT ( 'NONE',  ( 779.9999999999990905, 18.49609980828599376, -309.9999999999999432 ) ) ;
#30234 = CARTESIAN_POINT ( 'NONE',  ( 787.3558975768202117, 16.45630643248848557, 313.9911135047267408 ) ) ;
#30235 = DIRECTION ( 'NONE',  ( 0.000000000000000000, 0.000000000000000000, 1.000000000000000000 ) ) ;
#30236 = CARTESIAN_POINT ( 'NONE',  ( 757.4527132478984868, -184.3726999360619629, 329.1273215169538844 ) ) ;
#30237 = CARTESIAN_POINT ( 'NONE',  ( 756.5762568750052424, -75.18005720387485269, 348.7366044899774238 ) ) ;
#30238 = EDGE_LOOP ( 'NONE', ( #43632, #20183 ) ) ;
#30239 = CARTESIAN_POINT ( 'NONE',  ( 796.2681130854250569, -462.7578698805381237, -371.0719813302654870 ) ) ;
#30240 = CARTESIAN_POINT ( 'NONE',  ( 782.5225473063383106, -22.27096629478410605, -375.2698199232970637 ) ) ;
#30241 = CARTESIAN_POINT ( 'NONE',  ( 805.1016975059191054, -270.8965053807777394, 343.0745993439771837 ) ) ;
#30242 = CARTESIAN_POINT ( 'NONE',  ( 795.1360043628807261, -404.0891481129646081, -360.2193346964456282 ) ) ;
#30243 = CARTESIAN_POINT ( 'NONE',  ( 795.1360043628808398, -20.08914811296593328, -360.2193346964456282 ) ) ;
#30244 = CARTESIAN_POINT ( 'NONE',  ( 796.9462024416508257, -444.4527844766009821, 308.9653473494370246 ) ) ;
#30245 = LINE ( 'NONE', #40439, #4096 ) ;
#30246 = CARTESIAN_POINT ( 'NONE',  ( 773.4516893846965786, -283.6454272087889308, -315.8398074228977066 ) ) ;
#30247 = CARTESIAN_POINT ( 'NONE',  ( 782.5225473063381969, -166.2709662947835909, -375.2698199232970637 ) ) ;
#30248 = CARTESIAN_POINT ( 'NONE',  ( 745.7998596910086917, -77.36187538569302546, 332.5602148656461168 ) ) ;
#30249 = CARTESIAN_POINT ( 'NONE',  ( 777.5031285880264704, -142.8164208402382656, 374.9108240113588408 ) ) ;
#30250 = CARTESIAN_POINT ( 'NONE',  ( 959.5497976682736407, 239.9999999999998863, 350.0000000000000000 ) ) ;
#30251 = DIRECTION ( 'NONE',  ( -0.000000000000000000, 1.000000000000000000, -0.000000000000000000 ) ) ;
#30252 = CARTESIAN_POINT ( 'NONE',  ( 747.3154664389472828, -235.9874144716868898, -326.4474001241230781 ) ) ;
#30253 = DIRECTION ( 'NONE',  ( 0.000000000000000000, 1.000000000000000000, 0.000000000000000000 ) ) ;
#30254 = CARTESIAN_POINT ( 'NONE',  ( 777.4774526936600978, -394.2709662947827951, 304.7301800767027657 ) ) ;
#30255 = CARTESIAN_POINT ( 'NONE',  ( 755.2512626584698410, -7.543693567511430942, 315.2512626584710915 ) ) ;
#30256 = CARTESIAN_POINT ( 'NONE',  ( 762.1405469898971887, -337.5436935675102177, -357.8594530101015607 ) ) ;
#30257 = CARTESIAN_POINT ( 'NONE',  ( 772.3691319403857278, 24.73985825558500551, 315.8894580844506663 ) ) ;
#30258 = CARTESIAN_POINT ( 'NONE',  ( 746.4236121716829757, -111.8272453906076151, -328.8385539511384650 ) ) ;
#30259 = CARTESIAN_POINT ( 'NONE',  ( 769.1273215169530886, -142.7146871989599219, -317.4527132478988847 ) ) ;
#30260 = CARTESIAN_POINT ( 'NONE',  ( 811.6461892240364477, -124.7146871989599930, 324.1737431748509835 ) ) ;
#30261 = CARTESIAN_POINT ( 'NONE',  ( 773.4999999999993179, -365.3551492539851893, -18.13243251470705886 ) ) ;
#30262 = CARTESIAN_POINT ( 'NONE',  ( 764.8639956371174549, -56.08914811296580893, -319.7806653035542013 ) ) ;
#30263 = CARTESIAN_POINT ( 'NONE',  ( 803.2186876482843445, -151.9874144716871740, -350.0220218866286928 ) ) ;
#30264 = CARTESIAN_POINT ( 'NONE',  ( 765.0180583372156207, -120.9982390220565378, -360.0135310231089534 ) ) ;
#30265 = CARTESIAN_POINT ( 'NONE',  ( 755.0636971347428243, -172.2709662947836478, 341.7834795799807353 ) ) ;
#30266 = ADVANCED_FACE ( 'NONE', ( #38989 ), #21415, .F. ) ;
#30267 = CARTESIAN_POINT ( 'NONE',  ( 813.9316612368132837, -7.441959926233078448, -348.6739635108323228 ) ) ;
#30268 = CARTESIAN_POINT ( 'NONE',  ( 755.3201227861273992, -291.7255117493286320, 345.3687786644892981 ) ) ;
#30269 = DIRECTION ( 'NONE',  ( 1.892425610156518354E-16, 1.000000000000000000, -0.000000000000000000 ) ) ;
#30270 = ORIENTED_EDGE ( 'NONE', *, *, #39742, .T. ) ;
#30271 = CARTESIAN_POINT ( 'NONE',  ( 794.1144889064781864, -10.16923265350579442, 360.9840315886528401 ) ) ;
#30272 = CARTESIAN_POINT ( 'NONE',  ( 788.6739635108323228, -271.6454272087889876, -373.9316612368139090 ) ) ;
#30273 = ORIENTED_EDGE ( 'NONE', *, *, #1182, .F. ) ;
#30274 = DIRECTION ( 'NONE',  ( 0.000000000000000000, 0.000000000000000000, 1.000000000000000000 ) ) ;
#30275 = CARTESIAN_POINT ( 'NONE',  ( 772.4837098697145166, -215.3618753856925707, 374.5518280994205611 ) ) ;
#30276 = CARTESIAN_POINT ( 'NONE',  ( 755.5913626894240451, -301.6454272087889308, 346.6156483768012890 ) ) ;
#30277 = CARTESIAN_POINT ( 'NONE',  ( 789.9200121543843807, -409.9874144716863498, 317.0176451133914384 ) ) ;
#30278 = VERTEX_POINT ( 'NONE', #29030 ) ;
#30279 = CARTESIAN_POINT ( 'NONE',  ( 793.0897708529556667, -126.5545181178803205, -361.3366627262616362 ) ) ;
#30280 = CARTESIAN_POINT ( 'NONE',  ( 785.3687786644884454, -107.3618753856928976, -315.3201227861279676 ) ) ;
#30281 = CARTESIAN_POINT ( 'NONE',  ( 803.6646147819162707, -305.9073299311468190, -348.8264449731211130 ) ) ;
#30282 = VERTEX_POINT ( 'NONE', #25565 ) ;
#30283 = CARTESIAN_POINT ( 'NONE',  ( 797.6776695296629214, -427.5436935675101040, -357.6776695296636603 ) ) ;
#30284 = CARTESIAN_POINT ( 'NONE',  ( 804.6798772138708955, -87.72551174932937101, -334.6312213355107019 ) ) ;
#30285 = CARTESIAN_POINT ( 'NONE',  ( 805.0264073115434940, -294.3510508353230648, 339.4763451958999099 ) ) ;
#30286 = CARTESIAN_POINT ( 'NONE',  ( 939.9999999999993179, -590.0000000000001137, -350.0000000000000000 ) ) ;
#30287 = LINE ( 'NONE', #22900, #38148 ) ;
#30288 = CARTESIAN_POINT ( 'NONE',  ( -468.8365100919714337, 230.0000000000001421, -197.2499999999910187 ) ) ;
#30289 = EDGE_CURVE ( 'NONE', #9329, #44845, #23972, .T. ) ;
#30290 = EDGE_LOOP ( 'NONE', ( #40686, #17638 ) ) ;
#30291 = CARTESIAN_POINT ( 'NONE',  ( 802.2119215644370342, -342.0090635724251342, -367.5423716828165084 ) ) ;
#30292 = CARTESIAN_POINT ( 'NONE',  ( 804.9363028652555840, -304.2709662947832499, -338.2165204200192079 ) ) ;
#30293 = CARTESIAN_POINT ( 'NONE',  ( 799.9999999999993179, 205.0000000000000568, -350.0000000000000000 ) ) ;
#30294 = CARTESIAN_POINT ( 'NONE',  ( 755.5913626894240451, -181.6454272087892434, -346.6156483768012890 ) ) ;
#30295 = CARTESIAN_POINT ( 'NONE',  ( 777.5031285880264704, -46.81642084023858530, 374.9108240113588408 ) ) ;
#30296 = DIRECTION ( 'NONE',  ( -0.000000000000000000, 1.000000000000000000, -0.000000000000000000 ) ) ;
#30297 = CARTESIAN_POINT ( 'NONE',  ( 746.8695393053151292, -365.9073299311466485, -327.6429770376306578 ) ) ;
#30298 = DIRECTION ( 'NONE',  ( 0.000000000000000000, 0.000000000000000000, 1.000000000000000000 ) ) ;
#30299 = CARTESIAN_POINT ( 'NONE',  ( 794.9819416627830151, -60.99823902205671544, 319.9864689768909898 ) ) ;
#30300 = EDGE_CURVE ( 'NONE', #1931, #12197, #28412, .T. ) ;
#30301 = CARTESIAN_POINT ( 'NONE',  ( 764.1737431748507561, -322.3726999360615082, 371.6461892240376415 ) ) ;
#30302 = CARTESIAN_POINT ( 'NONE',  ( 755.2512626584698410, -271.5436935675106156, 315.2512626584710915 ) ) ;
#30303 = CARTESIAN_POINT ( 'NONE',  ( 767.7687537140311633, -23.90732993114773919, -372.7932403749916830 ) ) ;
#30304 = CARTESIAN_POINT ( 'NONE',  ( 756.5762568750052424, -243.1800572038743269, -348.7366044899774238 ) ) ;
#30305 = ADVANCED_FACE ( 'NONE', ( #39896 ), #630, .F. ) ;
#30306 = CARTESIAN_POINT ( 'NONE',  ( 772.4999999999993179, -462.9681489794447202, -270.0000000000000568 ) ) ;
#30307 = CARTESIAN_POINT ( 'NONE',  ( 755.0636971347428243, -364.2709662947830793, 341.7834795799807353 ) ) ;
#30308 = CARTESIAN_POINT ( 'NONE',  ( 761.4292242960306112, -137.4636090269711985, 323.2154366446414429 ) ) ;
#30309 = CARTESIAN_POINT ( 'NONE',  ( 783.0433043558608688, -48.89650538077840025, -315.1538015810313027 ) ) ;
#30310 = CARTESIAN_POINT ( 'NONE',  ( 752.4576283171824116, -45.07832356259660145, 317.7880784355627952 ) ) ;
#30311 = CARTESIAN_POINT ( 'NONE',  ( 801.9419747391806368, -354.4527844766012095, 351.9812246680014027 ) ) ;
#30312 = DIRECTION ( 'NONE',  ( -0.000000000000000000, -0.000000000000000000, 1.000000000000000000 ) ) ;
#30313 = DIRECTION ( 'NONE',  ( -1.000000000000000000, 0.000000000000000000, 0.000000000000000000 ) ) ;
#30314 = CARTESIAN_POINT ( 'NONE',  ( 801.9419747391806368, -402.4527844766010389, 351.9812246680014027 ) ) ;
#30315 = ORIENTED_EDGE ( 'NONE', *, *, #37138, .F. ) ;
#30316 = CARTESIAN_POINT ( 'NONE',  ( 804.6798772138708955, -39.72551174932951312, -334.6312213355107019 ) ) ;
#30317 = EDGE_CURVE ( 'NONE', #26139, #32281, #22307, .T. ) ;
#30318 = EDGE_CURVE ( 'NONE', #36817, #32851, #22094, .T. ) ;
#30319 = CARTESIAN_POINT ( 'NONE',  ( 757.2208543904082489, -328.7146871989592682, -350.9844846989624330 ) ) ;
#30321 = CARTESIAN_POINT ( 'NONE',  ( 759.7806653035535192, -174.9982390220563673, 324.8639956371181370 ) ) ;
#30320 = CARTESIAN_POINT ( 'NONE',  ( 804.6798772138708955, -183.7255117493290015, 334.6312213355107019 ) ) ;
#30322 = CARTESIAN_POINT ( 'NONE',  ( 746.7653713866222915, -353.2601417444137724, -351.0478386215610271 ) ) ;
#30323 = CARTESIAN_POINT ( 'NONE',  ( -786.4999999999993179, -544.8427095258973623, -369.9999999999999432 ) ) ;
#30324 = ORIENTED_EDGE ( 'NONE', *, *, #14574, .F. ) ;
#30325 = CARTESIAN_POINT ( 'NONE',  ( 759.7806653035534055, -342.9982390220557136, 324.8639956371180801 ) ) ;
#30326 = EDGE_LOOP ( 'NONE', ( #11883, #18043, #36660, #2849 ) ) ;
#30327 = CARTESIAN_POINT ( 'NONE',  ( 787.4397851343537695, -213.7255117493289731, -374.2001403089903988 ) ) ;
#30328 = CARTESIAN_POINT ( 'NONE',  ( 751.9810565676468741, -122.0891481129656171, 360.9747183278973921 ) ) ;
#30329 = ORIENTED_EDGE ( 'NONE', *, *, #6342, .F. ) ;
#30330 = CARTESIAN_POINT ( 'NONE',  ( 804.9363028652555840, -160.2709662947836762, -338.2165204200192079 ) ) ;
#30331 = ORIENTED_EDGE ( 'NONE', *, *, #16185, .F. ) ;
#30332 = EDGE_CURVE ( 'NONE', #29494, #34816, #21872, .T. ) ;
#30333 = CARTESIAN_POINT ( 'NONE',  ( 764.8639956371174549, -320.0891481129648355, -319.7806653035542013 ) ) ;
#30334 = CARTESIAN_POINT ( 'NONE',  ( 764.8639956371174549, 15.91085188703394238, -319.7806653035542013 ) ) ;
#30335 = ADVANCED_FACE ( 'NONE', ( #26464 ), #9134, .F. ) ;
#30336 = CARTESIAN_POINT ( 'NONE',  ( 745.7998596910086917, -245.3618753856925139, 332.5602148656461168 ) ) ;
#30337 = CARTESIAN_POINT ( 'NONE',  ( 756.7813123517142913, -187.9874144716870603, 329.9779781133712504 ) ) ;
#30339 = CARTESIAN_POINT ( 'NONE',  ( 779.9999999999992042, -452.9681489794448339, -339.9999999999999432 ) ) ;
#30338 = DIRECTION ( 'NONE',  ( 0.000000000000000000, 0.000000000000000000, 1.000000000000000000 ) ) ;
#30340 = FACE_OUTER_BOUND ( 'NONE', #8519, .T. ) ;
#30341 = ORIENTED_EDGE ( 'NONE', *, *, #30846, .T. ) ;
#30342 = CARTESIAN_POINT ( 'NONE',  ( 766.0291762391763086, -442.9181544815157849, -360.7704444035551319 ) ) ;
#30343 = CARTESIAN_POINT ( 'NONE',  ( -39.63011601220123481, -513.1383975375929367, -349.9999999999999432 ) ) ;
#30344 = CARTESIAN_POINT ( 'NONE',  ( 701.1634899080286232, 229.9999999999999147, -197.2499999999991758 ) ) ;
#30345 = ORIENTED_EDGE ( 'NONE', *, *, #8376, .T. ) ;
#30346 = CARTESIAN_POINT ( 'NONE',  ( 811.3240766477731540, -244.3726999360617924, -355.6651683502462902 ) ) ;
#30347 = VECTOR ( 'NONE', #33939, 1000.000000000000000 ) ;
#30348 = CARTESIAN_POINT ( 'NONE',  ( 745.7194118038753459, -109.6454272087894566, 348.7631598425976449 ) ) ;
#30350 = CARTESIAN_POINT ( 'NONE',  ( 774.6858677611749044, -177.7255117493290868, -315.5713283507209894 ) ) ;
#30349 = DIRECTION ( 'NONE',  ( 0.000000000000000000, -1.000000000000000000, 0.000000000000000000 ) ) ;
#30351 = CARTESIAN_POINT ( 'NONE',  ( 790.8726784830453198, -370.7146871989592114, -362.5472867521010585 ) ) ;
#30352 = DIRECTION ( 'NONE',  ( 0.000000000000000000, 0.000000000000000000, 1.000000000000000000 ) ) ;
#30353 = CARTESIAN_POINT ( 'NONE',  ( 762.1177392798416577, -234.5545181178799794, -309.8865473780659272 ) ) ;
#30354 = CARTESIAN_POINT ( 'NONE',  ( 779.9999999999992042, 16.45630643248849267, 339.9999999999999432 ) ) ;
#30355 = DIRECTION ( 'NONE',  ( 0.000000000000000000, 0.000000000000000000, 1.000000000000000000 ) ) ;
#30356 = CARTESIAN_POINT ( 'NONE',  ( 766.9102291470427417, -90.55451811788041994, -318.6633372737382501 ) ) ;
#30357 = CARTESIAN_POINT ( 'NONE',  ( 799.2566176426618085, -432.0090635724247932, 324.0069404352559559 ) ) ;
#30358 = PLANE ( 'NONE',  #26350 ) ;
#30359 = CARTESIAN_POINT ( 'NONE',  ( 769.1273215169530886, -430.7146871989590409, -317.4527132478988847 ) ) ;
#30360 = CARTESIAN_POINT ( 'NONE',  ( 804.7487373415286811, -283.5436935675105019, -364.7487373415288516 ) ) ;
#30361 = ADVANCED_FACE ( 'NONE', ( #5214 ), #5428, .F. ) ;
#30362 = CARTESIAN_POINT ( 'NONE',  ( 779.9999999999992042, 16.45630643248849267, -339.9999999999999432 ) ) ;
#30363 = DIRECTION ( 'NONE',  ( -0.000000000000000000, -0.000000000000000000, 1.000000000000000000 ) ) ;
#30364 = CARTESIAN_POINT ( 'NONE',  ( 804.4286716492782716, -65.36187538569306810, -345.3141322388244703 ) ) ;
#30365 = ADVANCED_FACE ( 'NONE', ( #29699 ), #23201, .F. ) ;
#30366 = CARTESIAN_POINT ( 'NONE',  ( 746.4236121716829757, -231.8272453906072315, 328.8385539511384650 ) ) ;
#30367 = CARTESIAN_POINT ( 'NONE',  ( 773.7943932421234194, -167.8055962898689586, -305.5313806188329409 ) ) ;
#30368 = CARTESIAN_POINT ( 'NONE',  ( 763.0537975583475827, -168.4527844766018347, 371.0346526505627480 ) ) ;
#30369 = CARTESIAN_POINT ( 'NONE',  ( 814.5518280994195948, -399.7255117493283478, -332.4837098697145734 ) ) ;
#30370 = DIRECTION ( 'NONE',  ( 0.000000000000000000, 0.000000000000000000, -1.000000000000000000 ) ) ;
#30371 = EDGE_CURVE ( 'NONE', #8196, #38417, #37542, .T. ) ;
#30372 = CARTESIAN_POINT ( 'NONE',  ( 768.0187753319979720, -248.6346026584197659, 318.0580252608186242 ) ) ;
#30373 = CARTESIAN_POINT ( 'NONE',  ( 793.9708237608222134, -46.91815448151694312, 319.2295555964448681 ) ) ;
#30374 = CARTESIAN_POINT ( 'NONE',  ( 791.9812246680005501, -380.6346026584192828, -361.9419747391813189 ) ) ;
#30375 = CARTESIAN_POINT ( 'NONE',  ( -454.7528517110260964, 200.0000000000001137, -122.7905160835438068 ) ) ;
#30376 = CARTESIAN_POINT ( 'NONE',  ( 786.4999999999993179, 35.55895481007120651, 914.5706932916501728 ) ) ;
#30377 = CARTESIAN_POINT ( 'NONE',  ( 793.2243759319678702, -98.53286901714187707, 318.4439275373583200 ) ) ;
#30378 = EDGE_LOOP ( 'NONE', ( #38414, #28729, #42566, #41252, #45592, #22845 ) ) ;
#30379 = EDGE_CURVE ( 'NONE', #18435, #39568, #11923, .T. ) ;
#30380 = PRODUCT_RELATED_PRODUCT_CATEGORY ( 'part', '', ( #31792 ) ) ;
#30381 = CARTESIAN_POINT ( 'NONE',  ( 780.5290396650775619, -228.3510508353232922, -365.2837595273619513 ) ) ;
#30382 = CARTESIAN_POINT ( 'NONE',  ( 768.0187753319979720, -56.63460265842036279, 318.0580252608186242 ) ) ;
#30383 = AXIS2_PLACEMENT_3D ( 'NONE', #25545, #18620, #25306 ) ;
#30384 = CARTESIAN_POINT ( 'NONE',  ( 776.2433038121456548, -276.8965053807776258, -374.8207195650711014 ) ) ;
#30385 = CARTESIAN_POINT ( 'NONE',  ( 815.1787889125755555, -366.8965053807773984, 343.7953271457877804 ) ) ;
#30386 = EDGE_LOOP ( 'NONE', ( #5496, #30315 ) ) ;
#30387 = CARTESIAN_POINT ( 'NONE',  ( 762.3223304703356007, -271.5436935675106156, 322.3223304703362828 ) ) ;
#30388 = CARTESIAN_POINT ( 'NONE',  ( 813.1304606946830518, 6.092670068852159559, 352.3570229623690580 ) ) ;
#30389 = CARTESIAN_POINT ( 'NONE',  ( 794.9819416627830151, -180.9982390220563389, -319.9864689768909898 ) ) ;
#30390 = CARTESIAN_POINT ( 'NONE',  ( 781.8018195045266339, -382.2709662947828519, 365.1927285166406705 ) ) ;
#30391 = CARTESIAN_POINT ( 'NONE',  ( 787.4397851343537695, -93.72551174932934259, -374.2001403089903988 ) ) ;
#30392 = CARTESIAN_POINT ( 'NONE',  ( 792.1044303154646968, -84.45278447660207632, -317.8323909638837677 ) ) ;
#30393 = ORIENTED_EDGE ( 'NONE', *, *, #16443, .F. ) ;
#30394 = CARTESIAN_POINT ( 'NONE',  ( 766.9102291470427417, -18.55451811788065797, -318.6633372737382501 ) ) ;
#30395 = ORIENTED_EDGE ( 'NONE', *, *, #45233, .F. ) ;
#30396 = CARTESIAN_POINT ( 'NONE',  ( 757.4527132478984868, -352.3726999360614514, -329.1273215169538844 ) ) ;
#30398 = CARTESIAN_POINT ( 'NONE',  ( 793.9708237608222134, -406.9181544815157849, 319.2295555964448681 ) ) ;
#30397 = CARTESIAN_POINT ( 'NONE',  ( 755.0636971347428243, -100.2709662947838609, 341.7834795799807353 ) ) ;
#30401 = CARTESIAN_POINT ( 'NONE',  ( 807.5423716828161105, -369.0783235625956422, 362.2119215644372048 ) ) ;
#30400 = LINE ( 'NONE', #29953, #20314 ) ;
#30399 = CARTESIAN_POINT ( 'NONE',  ( 745.4481719005789273, -435.7255117493282341, 347.5162901302853697 ) ) ;
#30402 = CARTESIAN_POINT ( 'NONE',  ( 804.4086373105744769, -313.6454272087888171, -333.3843516231986541 ) ) ;
#30403 = CARTESIAN_POINT ( 'NONE',  ( 802.1676090361156639, -326.6346026584193396, -327.8955696845344505 ) ) ;
#30404 = CIRCLE ( 'NONE', #27467, 10.00000000000000888 ) ;
#30405 = CARTESIAN_POINT ( 'NONE',  ( 745.7194118038753459, -133.6454272087893571, -348.7631598425976449 ) ) ;
#30406 = CARTESIAN_POINT ( 'NONE',  ( 782.4968714119720516, -442.8164208402372992, 305.0891759886411023 ) ) ;
#30408 = LINE ( 'NONE', #5463, #21888 ) ;
#30407 = CARTESIAN_POINT ( 'NONE',  ( -775.4999999999993179, -496.5085659523897448, -356.8883017825714319 ) ) ;
#30409 = CARTESIAN_POINT ( 'NONE',  ( 795.9930595647434757, -267.0783235625958696, -320.7433823573372820 ) ) ;
#30410 = CARTESIAN_POINT ( 'NONE',  ( 773.7305795820266212, -105.2817908451530968, -374.8230680027170365 ) ) ;
#30411 = CARTESIAN_POINT ( 'NONE',  ( 772.4999999999993179, -512.9681489794448908, -329.9999999999999432 ) ) ;
#30412 = CARTESIAN_POINT ( 'NONE',  ( -786.4999999999993179, -112.8054336623104348, 752.6593748957919843 ) ) ;
#30413 = CARTESIAN_POINT ( 'NONE',  ( 790.0220218866281812, -343.0999726633342561, 363.2186876482849129 ) ) ;
#30414 = VERTEX_POINT ( 'NONE', #12825 ) ;
#30415 = CARTESIAN_POINT ( 'NONE',  ( 805.6418435158337843, -293.4636090269707438, 363.8556311672236916 ) ) ;
#30416 = CARTESIAN_POINT ( 'NONE',  ( 800.9747183278959710, -180.9982390220563389, -311.9810565676471583 ) ) ;
#30417 = CARTESIAN_POINT ( 'NONE',  ( 914.9999999999992042, 99.99999999999984368, -360.0000000000000000 ) ) ;
#30418 = CARTESIAN_POINT ( 'NONE',  ( 749.5768839229115201, -108.5545181178803915, 358.0661480581553064 ) ) ;
#30419 = CARTESIAN_POINT ( 'NONE',  ( 767.7687537140311633, -287.9073299311468759, -372.7932403749916830 ) ) ;
#30420 = CARTESIAN_POINT ( 'NONE',  ( 914.9999999999992042, 74.99999999999984368, -350.0000000000000000 ) ) ;
#30421 = CARTESIAN_POINT ( 'NONE',  ( 804.9363028652555840, -136.2709662947837330, 338.2165204200192079 ) ) ;
#30422 = VERTEX_POINT ( 'NONE', #5001 ) ;
#30423 = CARTESIAN_POINT ( 'NONE',  ( 771.3260364891663130, -403.6454272087884760, 306.0683387631859773 ) ) ;
#30424 = CARTESIAN_POINT ( 'NONE',  ( 791.1614460488616487, -347.2601417444138860, -373.5763878283158874 ) ) ;
#30425 = CARTESIAN_POINT ( 'NONE',  ( 749.2812353651451076, -102.4527844766020337, -323.2262854647983090 ) ) ;
#30426 = CARTESIAN_POINT ( 'NONE',  ( 773.4516893846965786, -43.64542720878966975, 315.8398074228977066 ) ) ;
#30427 = CARTESIAN_POINT ( 'NONE',  ( 810.7187646348534145, -378.4527844766011526, -356.7737145352016341 ) ) ;
#30428 = DIRECTION ( 'NONE',  ( -1.000000000000000000, -1.644774851296528363E-16, 0.000000000000000000 ) ) ;
#30429 = CARTESIAN_POINT ( 'NONE',  ( 796.7845633553578182, -441.6237781080499190, 358.5707757039688204 ) ) ;
#30430 = ORIENTED_EDGE ( 'NONE', *, *, #15887, .F. ) ;
#30431 = CARTESIAN_POINT ( 'NONE',  ( 804.1601925771018387, -79.44195992623286884, 346.5483106153029098 ) ) ;
#30432 = VECTOR ( 'NONE', #36216, 1000.000000000000000 ) ;
#30433 = CARTESIAN_POINT ( 'NONE',  ( 754.0944755984390895, -111.6237781080509279, -364.1009440267246760 ) ) ;
#30434 = LINE ( 'NONE', #6181, #462 ) ;
#30435 = CARTESIAN_POINT ( 'NONE',  ( 761.9338519418445230, -278.5328690171412518, 370.4231160770881957 ) ) ;
#30436 = CARTESIAN_POINT ( 'NONE',  ( 757.8323909638828582, -74.63460265842030594, 352.1044303154654358 ) ) ;
#30437 = ORIENTED_EDGE ( 'NONE', *, *, #22046, .T. ) ;
#30438 = CARTESIAN_POINT ( 'NONE',  ( 804.4286716492782716, -257.3618753856924286, 345.3141322388244703 ) ) ;
#30439 = CARTESIAN_POINT ( 'NONE',  ( 776.2433038121456548, -420.8965053807772279, -374.8207195650711014 ) ) ;
#30440 = CARTESIAN_POINT ( 'NONE',  ( -468.8365100919714337, 240.0000000000001705, -199.9999999999908766 ) ) ;
#30441 = VERTEX_POINT ( 'NONE', #5900 ) ;
#30442 = CARTESIAN_POINT ( 'NONE',  ( 778.1981804954714335, -178.2709662947835625, -314.8072714833589885 ) ) ;
#30443 = CARTESIAN_POINT ( 'NONE',  ( 804.1009440267234822, -383.4636090269704596, -314.0944755984392600 ) ) ;
#30445 = CARTESIAN_POINT ( 'NONE',  ( 778.7502325331095108, -216.3510508353233490, 304.6391490659818828 ) ) ;
#30444 = CARTESIAN_POINT ( 'NONE',  ( 754.9967657858570647, -313.5436935675103882, 365.0032342141425943 ) ) ;
#30446 = CARTESIAN_POINT ( 'NONE',  ( 755.1538015810308480, -230.1908817542436338, -343.0433043558613804 ) ) ;
#30447 = CARTESIAN_POINT ( 'NONE',  ( 788.7366044899766848, -203.9073299311471885, -316.5762568750059813 ) ) ;
#30448 = CARTESIAN_POINT ( 'NONE',  ( 755.5713283507202505, -413.3618753856920307, -334.6858677611754729 ) ) ;
#30449 = ORIENTED_EDGE ( 'NONE', *, *, #20695, .T. ) ;
#30450 = CARTESIAN_POINT ( 'NONE',  ( 755.0636971347428243, -220.2709662947834772, 341.7834795799807353 ) ) ;
#30451 = CARTESIAN_POINT ( 'NONE',  ( 756.3353852180819104, -101.9073299311474727, -331.1735550268788302 ) ) ;
#30452 = ORIENTED_EDGE ( 'NONE', *, *, #4052, .T. ) ;
#30453 = CARTESIAN_POINT ( 'NONE',  ( 782.4968714119720516, -346.8164208402376971, 305.0891759886411023 ) ) ;
#30454 = FACE_OUTER_BOUND ( 'NONE', #14635, .T. ) ;
#30455 = CARTESIAN_POINT ( 'NONE',  ( 911.9749999999993406, 219.9999999999998863, 360.0000000000000000 ) ) ;
#30456 = FACE_BOUND ( 'NONE', #1080, .T. ) ;
#30457 = CARTESIAN_POINT ( 'NONE',  ( 769.0155153010367712, -226.3726999360617924, 362.7791456095907279 ) ) ;
#30458 = CARTESIAN_POINT ( 'NONE',  ( 774.6312213355099630, -95.36187538569294020, 364.6798772138717482 ) ) ;
#30459 = VERTEX_POINT ( 'NONE', #16295 ) ;
#30460 = CARTESIAN_POINT ( 'NONE',  ( 752.7379699480933368, -444.0090635724249069, -361.9858362298580232 ) ) ;
#30461 = AXIS2_PLACEMENT_3D ( 'NONE', #30585, #12369, #31043 ) ;
#30462 = CARTESIAN_POINT ( 'NONE',  ( 814.2001403089898304, -65.36187538569306810, -347.4397851343538264 ) ) ;
#30463 = CARTESIAN_POINT ( 'NONE',  ( 757.8323909638827445, -74.63460265842032015, 352.1044303154654358 ) ) ;
#30464 = CARTESIAN_POINT ( 'NONE',  ( 783.0433043558608688, -264.8965053807776826, 315.1538015810313027 ) ) ;
#30465 = CARTESIAN_POINT ( 'NONE',  ( 767.8955696845333705, -432.4527844766008684, -362.1676090361162323 ) ) ;
#30466 = CARTESIAN_POINT ( 'NONE',  ( 758.0580252608178853, -54.45278447660219001, -328.0187753319985404 ) ) ;
#30467 = CARTESIAN_POINT ( 'NONE',  ( 747.6481478633932056, -13.09997266333522248, 353.4146539503763620 ) ) ;
#30468 = DIRECTION ( 'NONE',  ( 0.000000000000000000, 0.000000000000000000, 1.000000000000000000 ) ) ;
#30469 = CARTESIAN_POINT ( 'NONE',  ( 758.4439275373578084, -300.5545181178797520, -353.2243759319684386 ) ) ;
#30470 = CARTESIAN_POINT ( 'NONE',  ( 767.7687537140311633, -191.9073299311471885, -372.7932403749916830 ) ) ;
#30471 = CARTESIAN_POINT ( 'NONE',  ( 746.8695393053150156, -77.90732993114757221, 327.6429770376306010 ) ) ;
#30472 = CARTESIAN_POINT ( 'NONE',  ( 767.7687537140311633, -143.9073299311473590, 372.7932403749916830 ) ) ;
#30473 = CARTESIAN_POINT ( 'NONE',  ( 772.4999999999993179, -462.9681489794448339, -370.0000000000000568 ) ) ;
#30474 = PRESENTATION_STYLE_ASSIGNMENT (( #33946 ) ) ;
#30475 = CARTESIAN_POINT ( 'NONE',  ( 771.2368401574024119, -229.4419599262323572, -374.2805881961240857 ) ) ;
#30476 = CIRCLE ( 'NONE', #6878, 10.00000000000000888 ) ;
#30477 = CARTESIAN_POINT ( 'NONE',  ( 745.5313806188320314, -423.2817908451521589, 333.7943932421247268 ) ) ;
#30478 = CARTESIAN_POINT ( 'NONE',  ( 758.8095938919642549, -296.0891481129650629, -311.6929314249763365 ) ) ;
#30479 = LINE ( 'NONE', #6225, #21322 ) ;
#30480 = CARTESIAN_POINT ( 'NONE',  ( 763.2262854647970016, -392.6346026584193396, 309.2812353651462445 ) ) ;
#30481 = CARTESIAN_POINT ( 'NONE',  ( 751.6929314249750860, -6.998239022056886860, 318.8095938919659034 ) ) ;
#30482 = CARTESIAN_POINT ( 'NONE',  ( 771.2633955100217236, -335.9073299311468190, -363.4237431249939618 ) ) ;
#30483 = CARTESIAN_POINT ( 'NONE',  ( 783.0433043558608688, -24.89650538077847486, 315.1538015810313027 ) ) ;
#30484 = CARTESIAN_POINT ( 'NONE',  ( 755.8990559732751535, -83.46360902697136908, -365.9055244015606831 ) ) ;
#30485 = CARTESIAN_POINT ( 'NONE',  ( 783.0433043558608688, -168.8965053807780237, -315.1538015810313027 ) ) ;
#30486 = CARTESIAN_POINT ( 'NONE',  ( 776.2433038121456548, -156.8965053807780805, 374.8207195650711014 ) ) ;
#30487 = CARTESIAN_POINT ( 'NONE',  ( 785.3687786644885591, 12.63812461430668677, 315.3201227861280813 ) ) ;
#30488 = VERTEX_POINT ( 'NONE', #30376 ) ;
#30489 = CARTESIAN_POINT ( 'NONE',  ( 756.3353852180819104, -53.90732993114765037, -331.1735550268788302 ) ) ;
#30490 = CARTESIAN_POINT ( 'NONE',  ( 805.1016975059191054, -174.8965053807779952, -343.0745993439771837 ) ) ;
#30491 = CARTESIAN_POINT ( 'NONE',  ( 803.4237431249931660, -159.1800572038746111, 331.2633955100225194 ) ) ;
#30492 = CARTESIAN_POINT ( 'NONE',  ( 781.2497674668890113, -12.35105083532396897, -375.3608509340180603 ) ) ;
#30494 = CARTESIAN_POINT ( 'NONE',  ( 771.1735550268780344, -297.1800572038741279, 316.3353852180828198 ) ) ;
#30493 = CARTESIAN_POINT ( 'NONE',  ( 756.5762568750052424, -291.1800572038741848, 348.7366044899774238 ) ) ;
#30495 = CIRCLE ( 'NONE', #16494, 10.00000000000000888 ) ;
#30496 = DIRECTION ( 'NONE',  ( 0.000000000000000000, 0.000000000000000000, 1.000000000000000000 ) ) ;
#30497 = ORIENTED_EDGE ( 'NONE', *, *, #35423, .T. ) ;
#30498 = CARTESIAN_POINT ( 'NONE',  ( 757.2208543904082489, -16.71468719896031985, 350.9844846989624330 ) ) ;
#30499 = AXIS2_PLACEMENT_3D ( 'NONE', #14293, #39020, #14070 ) ;
#30500 = CARTESIAN_POINT ( 'NONE',  ( 791.0478386215596629, -261.8272453906071746, -306.7653713866226326 ) ) ;
#30501 = VERTEX_POINT ( 'NONE', #12156 ) ;
#30502 = DIRECTION ( 'NONE',  ( 0.000000000000000000, 0.000000000000000000, -1.000000000000000000 ) ) ;
#30503 = CARTESIAN_POINT ( 'NONE',  ( 782.5225473063383106, -238.2709662947833920, 375.2698199232970637 ) ) ;
#30504 = CARTESIAN_POINT ( 'NONE',  ( 755.1538015810308480, -302.1908817542433781, 343.0433043558613804 ) ) ;
#30505 = CARTESIAN_POINT ( 'NONE',  ( 789.9200121543843807, -433.9874144716862361, 317.0176451133914384 ) ) ;
#30506 = VERTEX_POINT ( 'NONE', #34066 ) ;
#30507 = CARTESIAN_POINT ( 'NONE',  ( 755.8894580844503253, -111.8272453906076151, -332.3691319403863531 ) ) ;
#30508 = CARTESIAN_POINT ( 'NONE',  ( 755.3201227861273992, -99.72551174932928575, -345.3687786644892981 ) ) ;
#30509 = CARTESIAN_POINT ( 'NONE',  ( 805.1927285166399315, -328.8164208402375834, -341.8018195045277707 ) ) ;
#30510 = ORIENTED_EDGE ( 'NONE', *, *, #12322, .T. ) ;
#30511 = CARTESIAN_POINT ( 'NONE',  ( 764.8639956371174549, -440.0891481129644944, -319.7806653035542013 ) ) ;
#30512 = AXIS2_PLACEMENT_3D ( 'NONE', #4176, #7402, #35798 ) ;
#30513 = CARTESIAN_POINT ( 'NONE',  ( 756.7813123517142913, -307.9874144716866340, 329.9779781133712504 ) ) ;
#30514 = CARTESIAN_POINT ( 'NONE',  ( 831.1634899080286232, 256.4999999999998863, -206.1189999999999429 ) ) ;
#30515 = FACE_OUTER_BOUND ( 'NONE', #40153, .T. ) ;
#30516 = CARTESIAN_POINT ( 'NONE',  ( 763.8424801807145741, -114.0090635724258163, 320.5453621957614700 ) ) ;
#30517 = DIRECTION ( 'NONE',  ( -1.880165489482579047E-16, -1.000000000000000000, -0.000000000000000000 ) ) ;
#30518 = VERTEX_POINT ( 'NONE', #44469 ) ;
#30519 = CARTESIAN_POINT ( 'NONE',  ( 760.0363995740630116, -346.9181544815160123, -368.7758568127991907 ) ) ;
#30520 = EDGE_CURVE ( 'NONE', #27605, #16603, #4812, .T. ) ;
#30521 = CARTESIAN_POINT ( 'NONE',  ( 803.6646147819161570, -329.9073299311467053, -348.8264449731210561 ) ) ;
#30522 = SURFACE_STYLE_USAGE ( .BOTH. , #19447 ) ;
#30523 = CARTESIAN_POINT ( 'NONE',  ( 800.9840315886518738, -172.9181544815165239, -354.1144889064786412 ) ) ;
#30524 = EDGE_CURVE ( 'NONE', #1637, #21532, #19094, .T. ) ;
#30525 =( REPRESENTATION_RELATIONSHIP ('NONE','NONE', #39835, #4721 ) REPRESENTATION_RELATIONSHIP_WITH_TRANSFORMATION ( #21204 )SHAPE_REPRESENTATION_RELATIONSHIP( ) );
#30526 = CARTESIAN_POINT ( 'NONE',  ( 787.5162901302840055, -59.36187538569306810, 305.4481719005792684 ) ) ;
#30527 = VECTOR ( 'NONE', #21120, 1000.000000000000000 ) ;
#30528 = FACE_OUTER_BOUND ( 'NONE', #19493, .T. ) ;
#30529 = CARTESIAN_POINT ( 'NONE',  ( 787.5162901302840055, -371.3618753856920307, -305.4481719005793252 ) ) ;
#30530 = VECTOR ( 'NONE', #23188, 1000.000000000000000 ) ;
#30531 = LINE ( 'NONE', #26393, #1068 ) ;
#30532 = CARTESIAN_POINT ( 'NONE',  ( 802.2119215644370342, -318.0090635724251911, 367.5423716828165084 ) ) ;
#30533 = FACE_OUTER_BOUND ( 'NONE', #25749, .T. ) ;
#30534 = CARTESIAN_POINT ( 'NONE',  ( 782.5225473063381969, -286.2709662947833635, 375.2698199232970637 ) ) ;
#30535 = CARTESIAN_POINT ( 'NONE',  ( 772.4837098697144029, -23.36187538569318889, -374.5518280994205611 ) ) ;
#30536 = CARTESIAN_POINT ( 'NONE',  ( 785.3141322388236176, -237.7255117493289163, -364.4286716492789537 ) ) ;
#30537 = DIRECTION ( 'NONE',  ( 0.000000000000000000, 0.000000000000000000, -1.000000000000000000 ) ) ;
#30538 = CARTESIAN_POINT ( 'NONE',  ( 795.1360043628807261, -356.0891481129647218, 360.2193346964456282 ) ) ;
#30539 = CARTESIAN_POINT ( 'NONE',  ( 772.4468031744293057, -129.8272453906075725, 363.8651313633793620 ) ) ;
#30540 = CARTESIAN_POINT ( 'NONE',  ( 755.0488828828309806, -65.80559628986925702, -344.1219089521771934 ) ) ;
#30541 = CARTESIAN_POINT ( 'NONE',  ( 768.8385539511368734, -71.26014174441469606, 306.4236121716840557 ) ) ;
#30542 = CARTESIAN_POINT ( 'NONE',  ( 774.6858677611749044, -369.7255117493284615, 315.5713283507209894 ) ) ;
#30543 = LINE ( 'NONE', #27995, #1149 ) ;
#30544 = CIRCLE ( 'NONE', #20949, 8.025000000000003908 ) ;
#30545 = DIRECTION ( 'NONE',  ( 0.000000000000000000, 1.000000000000000000, -0.000000000000000000 ) ) ;
#30546 = CARTESIAN_POINT ( 'NONE',  ( 744.8212110874229666, -138.8965053807781374, 336.2046728542121627 ) ) ;
#30547 = CARTESIAN_POINT ( 'NONE',  ( 788.7366044899766848, -443.9073299311464780, 316.5762568750059813 ) ) ;
#30548 = EDGE_LOOP ( 'NONE', ( #43194, #12344, #20777, #12401 ) ) ;
#30549 = CARTESIAN_POINT ( 'NONE',  ( 758.6633372737375112, -356.5328690171410813, -326.9102291470432533 ) ) ;
#30551 = CARTESIAN_POINT ( 'NONE',  ( 765.0180583372156207, -192.9982390220562820, 360.0135310231089534 ) ) ;
#30550 = CARTESIAN_POINT ( 'NONE',  ( 771.1735550268778070, -177.1800572038744690, 316.3353852180827630 ) ) ;
#30552 = CARTESIAN_POINT ( 'NONE',  ( 758.0141637701419768, -351.0783235625955854, -367.2620300519063790 ) ) ;
#30553 = CARTESIAN_POINT ( 'NONE',  ( 199.6009925648704098, 290.0000000000001137, -274.9999999999999432 ) ) ;
#30554 = VERTEX_POINT ( 'NONE', #26239 ) ;
#30555 = CARTESIAN_POINT ( 'NONE',  ( 759.9864689768902508, -410.0891481129647218, 354.9819416627836404 ) ) ;
#30556 = VERTEX_POINT ( 'NONE', #22769 ) ;
#30557 = CARTESIAN_POINT ( 'NONE',  ( 767.6429770376289525, -201.1800572038744690, -306.8695393053162093 ) ) ;
#30558 = CARTESIAN_POINT ( 'NONE',  ( 763.2262854647970016, -104.6346026584202207, 309.2812353651462445 ) ) ;
#30559 = ORIENTED_EDGE ( 'NONE', *, *, #2117, .F. ) ;
#30560 = CARTESIAN_POINT ( 'NONE',  ( 751.2241431872005251, -184.1692326535052757, 359.9636004259367610 ) ) ;
#30561 = CARTESIAN_POINT ( 'NONE',  ( 791.9812246680005501, -212.6346026584198796, -361.9419747391813189 ) ) ;
#30562 = VECTOR ( 'NONE', #25191, 1000.000000000000000 ) ;
#30563 = ORIENTED_EDGE ( 'NONE', *, *, #12587, .T. ) ;
#30564 = CARTESIAN_POINT ( 'NONE',  ( 797.6776695296629214, -331.5436935675104451, -357.6776695296636603 ) ) ;
#30565 = CARTESIAN_POINT ( 'NONE',  ( 788.7366044899766848, 12.09267006885214180, -316.5762568750059813 ) ) ;
#30566 = CARTESIAN_POINT ( 'NONE',  ( 772.4837098697144029, -239.3618753856924570, 374.5518280994205611 ) ) ;
#30567 = CARTESIAN_POINT ( 'NONE',  ( 754.9735926884551418, -186.3510508353234343, 340.5236548041000333 ) ) ;
#30569 = DIRECTION ( 'NONE',  ( 0.000000000000000000, 0.000000000000000000, 1.000000000000000000 ) ) ;
#30568 = CARTESIAN_POINT ( 'NONE',  ( 779.9999999999992042, -462.9681489794448339, -309.9999999999998863 ) ) ;
#30570 = DIRECTION ( 'NONE',  ( 0.000000000000000000, 0.000000000000000000, -1.000000000000000000 ) ) ;
#30571 = EDGE_CURVE ( 'NONE', #14331, #42109, #9373, .T. ) ;
#30572 = ORIENTED_EDGE ( 'NONE', *, *, #37418, .T. ) ;
#30573 = CARTESIAN_POINT ( 'NONE',  ( 781.7834795799800531, 13.18357915976123174, -315.0636971347436202 ) ) ;
#30574 = DIRECTION ( 'NONE',  ( -1.000000000000000000, 0.000000000000000000, 0.000000000000000000 ) ) ;
#30575 = DIRECTION ( 'NONE',  ( -1.000000000000000000, 0.000000000000000000, -0.000000000000000000 ) ) ;
#30576 = EDGE_LOOP ( 'NONE', ( #40064, #40523 ) ) ;
#30577 = CARTESIAN_POINT ( 'NONE',  ( 776.2046728542105711, -236.1908817542436338, -304.8212110874238761 ) ) ;
#30578 = CARTESIAN_POINT ( 'NONE',  ( 773.7305795820266212, -105.2817908451530968, 374.8230680027170365 ) ) ;
#30579 = VECTOR ( 'NONE', #20266, 1000.000000000000114 ) ;
#30581 = CARTESIAN_POINT ( 'NONE',  ( 764.8639956371174549, -176.0891481129653755, -319.7806653035542013 ) ) ;
#30580 = DIRECTION ( 'NONE',  ( 1.892425610156518354E-16, 1.000000000000000000, -0.000000000000000000 ) ) ;
#30582 = CARTESIAN_POINT ( 'NONE',  ( 756.7813123517142913, -355.9874144716865203, -329.9779781133712504 ) ) ;
#30583 = CARTESIAN_POINT ( 'NONE',  ( 788.6739635108323228, -247.6454272087890160, -373.9316612368139090 ) ) ;
#30584 = CARTESIAN_POINT ( 'NONE',  ( 989.9999999999992042, -590.0000000000001137, -350.0000000000000000 ) ) ;
#30585 = CARTESIAN_POINT ( 'NONE',  ( 919.9999999999993179, 219.9999999999998863, 360.0000000000000000 ) ) ;
#30586 = CARTESIAN_POINT ( 'NONE',  ( 766.0291762391763086, -82.91815448151682233, -360.7704444035551319 ) ) ;
#30587 = EDGE_CURVE ( 'NONE', #2036, #1585, #29929, .T. ) ;
#30588 = CARTESIAN_POINT ( 'NONE',  ( 786.5483106153019435, -439.6454272087884760, 364.1601925771022366 ) ) ;
#30589 = AXIS2_PLACEMENT_3D ( 'NONE', #36123, #1006, #44468 ) ;
#30590 = CARTESIAN_POINT ( 'NONE',  ( 795.8262568251477660, -358.3726999360613945, 308.3538107759623585 ) ) ;
#30591 = DIRECTION ( 'NONE',  ( 1.000000000000000000, 0.000000000000000000, -0.000000000000000000 ) ) ;
#30592 = CARTESIAN_POINT ( 'NONE',  ( 779.4709603349208464, -432.3510508353226669, -314.7162404726379918 ) ) ;
#30593 = CARTESIAN_POINT ( 'NONE',  ( 767.6429770376291799, -273.1800572038742985, -306.8695393053162093 ) ) ;
#30594 = FACE_OUTER_BOUND ( 'NONE', #14159, .T. ) ;
#30595 = DIRECTION ( 'NONE',  ( -1.000000000000000000, 1.880165489482579047E-16, 0.000000000000000000 ) ) ;
#30596 = CARTESIAN_POINT ( 'NONE',  ( 795.1360043628807261, -44.08914811296584446, -360.2193346964456282 ) ) ;
#30597 = CARTESIAN_POINT ( 'NONE',  ( 764.1737431748507561, -202.3726999360618777, 371.6461892240376415 ) ) ;
#30598 = CARTESIAN_POINT ( 'NONE',  ( 805.9055244015594326, -171.6237781080507432, -315.8990559732753240 ) ) ;
#30599 = CARTESIAN_POINT ( 'NONE',  ( 814.9108240113580450, -184.2709662947835909, 337.5031285880265273 ) ) ;
#30600 = CARTESIAN_POINT ( 'NONE',  ( 755.2512626584698410, -415.5436935675102177, -315.2512626584710915 ) ) ;
#30601 = DIRECTION ( 'NONE',  ( -1.000000000000000000, -0.000000000000000000, 0.000000000000000000 ) ) ;
#30602 = CLOSED_SHELL ( 'NONE', ( #38519, #40741, #1131, #42476, #45087, #38567, #22374, #13640, #35071, #34021, #43593, #30305, #22405, #19069, #43611, #2030, #3818, #20170, #19043, #18150, #9721, #32219, #36452, #39752 ) ) ;
#30603 = CARTESIAN_POINT ( 'NONE',  ( 759.9864689768902508, -266.0891481129651197, 354.9819416627836404 ) ) ;
#30604 = AXIS2_PLACEMENT_3D ( 'NONE', #5311, #29587, #43663 ) ;
#30605 = CARTESIAN_POINT ( 'NONE',  ( 769.9779781133707957, -67.09997266333506616, 316.7813123517150871 ) ) ;
#30606 = EDGE_CURVE ( 'NONE', #44956, #38954, #36863, .T. ) ;
#30607 = CARTESIAN_POINT ( 'NONE',  ( 805.1927285166397041, -424.8164208402372992, -341.8018195045277707 ) ) ;
#30608 = AXIS2_PLACEMENT_3D ( 'NONE', #13674, #31218, #6512 ) ;
#30609 = PLANE ( 'NONE',  #8480 ) ;
#30611 = EDGE_CURVE ( 'NONE', #45491, #18941, #44245, .T. ) ;
#30610 = FACE_OUTER_BOUND ( 'NONE', #8562, .T. ) ;
#30613 = CARTESIAN_POINT ( 'NONE',  ( 802.1676090361156639, -326.6346026584193396, 327.8955696845344505 ) ) ;
#30612 = CARTESIAN_POINT ( 'NONE',  ( 780.5290396650775619, -84.35105083532374692, 365.2837595273619513 ) ) ;
#30614 = ORIENTED_EDGE ( 'NONE', *, *, #35064, .F. ) ;
#30615 = CARTESIAN_POINT ( 'NONE',  ( 758.6633372737375112, -260.5328690171413086, -326.9102291470432533 ) ) ;
#30616 = EDGE_CURVE ( 'NONE', #20005, #33196, #31378, .T. ) ;
#30617 = CARTESIAN_POINT ( 'NONE',  ( 788.8264449731200330, -69.18005720387488111, 363.6646147819171233 ) ) ;
#30618 = CARTESIAN_POINT ( 'NONE',  ( 778.7502325331095108, -264.3510508353232353, -304.6391490659818828 ) ) ;
#30619 = DIRECTION ( 'NONE',  ( -1.000000000000000000, -0.000000000000000000, -0.000000000000000000 ) ) ;
#30620 = CARTESIAN_POINT ( 'NONE',  ( 758.0141637701419768, -375.0783235625955285, 367.2620300519063790 ) ) ;
#30621 = EDGE_LOOP ( 'NONE', ( #37212, #41657, #8673 ) ) ;
#30622 = CARTESIAN_POINT ( 'NONE',  ( 756.5762568750052424, -291.1800572038741848, 348.7366044899774238 ) ) ;
#30623 = AXIS2_PLACEMENT_3D ( 'NONE', #20445, #31062, #13522 ) ;
#30624 = CARTESIAN_POINT ( 'NONE',  ( 795.6651683502461765, -442.7146871989589840, 371.3240766477733814 ) ) ;
#30625 = CARTESIAN_POINT ( 'NONE',  ( 785.3687786644884454, -179.3618753856927128, -315.3201227861279676 ) ) ;
#30626 = CARTESIAN_POINT ( 'NONE',  ( 758.0580252608178853, -366.4527844766012095, 328.0187753319985404 ) ) ;
#30627 = CIRCLE ( 'NONE', #25486, 2.749999999999808153 ) ;
#30628 = CARTESIAN_POINT ( 'NONE',  ( 758.8095938919642549, -104.0891481129656881, -311.6929314249763365 ) ) ;
#30629 = AXIS2_PLACEMENT_3D ( 'NONE', #1496, #8443, #22288 ) ;
#30630 = CARTESIAN_POINT ( 'NONE',  ( 785.3687786644885591, -107.3618753856928976, -315.3201227861280813 ) ) ;
#30631 = VERTEX_POINT ( 'NONE', #22980 ) ;
#30632 = CARTESIAN_POINT ( 'NONE',  ( 779.4763451958990572, -32.73633629969879877, -365.0264073115438919 ) ) ;
#30633 = CARTESIAN_POINT ( 'NONE',  ( 804.1105419155481968, -363.8272453906068336, -347.6308680596136469 ) ) ;
#30634 = EDGE_CURVE ( 'NONE', #35055, #15183, #7020, .T. ) ;
#30636 = CARTESIAN_POINT ( 'NONE',  ( 757.0176451133909268, -421.0999726633340288, 349.9200121543848354 ) ) ;
#30635 = CARTESIAN_POINT ( 'NONE',  ( 781.7834795799800531, -82.81642084023846451, 315.0636971347436202 ) ) ;
#30637 = CARTESIAN_POINT ( 'NONE',  ( 756.7813123517142913, -91.98741447168737295, 329.9779781133712504 ) ) ;
#30640 = CARTESIAN_POINT ( 'NONE',  ( 754.0944755984390895, -351.6237781080502032, 364.1009440267246760 ) ) ;
#30639 = DIRECTION ( 'NONE',  ( 0.000000000000000000, 0.000000000000000000, 1.000000000000000000 ) ) ;
#30638 = DIRECTION ( 'NONE',  ( -0.000000000000000000, 1.000000000000000000, -0.000000000000000000 ) ) ;
#30641 = EDGE_CURVE ( 'NONE', #24881, #12460, #8466, .T. ) ;
#30642 = CARTESIAN_POINT ( 'NONE',  ( 793.0897708529556667, -366.5545181178795815, -361.3366627262616362 ) ) ;
#30643 = CARTESIAN_POINT ( 'NONE',  ( 801.9419747391806368, -330.4527844766013231, -351.9812246680014027 ) ) ;
#30644 = CARTESIAN_POINT ( 'NONE',  ( 744.6391490659812007, -134.7363362996984790, -338.7502325331110455 ) ) ;
#30645 = AXIS2_PLACEMENT_3D ( 'NONE', #31824, #35516, #3891 ) ;
#30646 = AXIS2_PLACEMENT_3D ( 'NONE', #33645, #1998, #30639 ) ;
#30648 = DIRECTION ( 'NONE',  ( 1.000000000000000000, 0.000000000000000000, 0.000000000000000000 ) ) ;
#30647 = CARTESIAN_POINT ( 'NONE',  ( 772.4999999999993179, -462.9681489794447771, 309.9999999999998863 ) ) ;
#30649 = CARTESIAN_POINT ( 'NONE',  ( 778.7629533639073998, -104.7363362996985785, -375.0009284576466371 ) ) ;
#30650 = DIRECTION ( 'NONE',  ( -1.000000000000000000, 0.000000000000000000, 0.000000000000000000 ) ) ;
#30652 = EDGE_CURVE ( 'NONE', #14643, #20167, #26681, .T. ) ;
#30651 = CARTESIAN_POINT ( 'NONE',  ( -468.8365100919714337, 240.0000000000001705, -197.2499999999910187 ) ) ;
#30653 = EDGE_CURVE ( 'NONE', #5854, #40626, #13981, .T. ) ;
#30654 = CARTESIAN_POINT ( 'NONE',  ( 800.9840315886518738, -316.9181544815160692, 354.1144889064786412 ) ) ;
#30655 = ORIENTED_EDGE ( 'NONE', *, *, #24599, .F. ) ;
#30656 = CARTESIAN_POINT ( 'NONE',  ( 781.2370466360911223, -308.7363362996979390, 304.9990715423533629 ) ) ;
#30657 = DIRECTION ( 'NONE',  ( 1.000000000000000000, 0.000000000000000000, 0.000000000000000000 ) ) ;
#30658 = VECTOR ( 'NONE', #5610, 1000.000000000000000 ) ;
#30659 = CARTESIAN_POINT ( 'NONE',  ( 791.0478386215596629, -117.8272453906076151, 306.7653713866226326 ) ) ;
#30660 = CARTESIAN_POINT ( 'NONE',  ( 745.0891759886404770, -292.2709662947831930, -342.4968714119734159 ) ) ;
#30661 = VECTOR ( 'NONE', #32118, 1000.000000000000000 ) ;
#30662 = DIRECTION ( 'NONE',  ( 0.000000000000000000, -1.000000000000000000, 0.000000000000000000 ) ) ;
#30663 = PRODUCT_DEFINITION_SHAPE ( 'NONE', 'NONE',  #45729 ) ;
#30664 = CARTESIAN_POINT ( 'NONE',  ( -598.8365100919716042, 260.0000000000001705, -199.9999999999899671 ) ) ;
#30665 = CARTESIAN_POINT ( 'NONE',  ( 781.8018195045266339, -142.2709662947837330, 365.1927285166406705 ) ) ;
#30666 = ORIENTED_EDGE ( 'NONE', *, *, #43810, .T. ) ;
#30667 = CARTESIAN_POINT ( 'NONE',  ( 809.0717654672305343, -412.9181544815157281, 360.1688906516309885 ) ) ;
#30668 = CARTESIAN_POINT ( 'NONE',  ( 751.2241431872005251, -376.1692326535046504, -359.9636004259367610 ) ) ;
#30669 = CARTESIAN_POINT ( 'NONE',  ( 787.4397851343537695, -117.7255117493292715, -374.2001403089903988 ) ) ;
#30670 = CARTESIAN_POINT ( 'NONE',  ( 763.0428371773158460, -35.46360902697151829, 358.7617431975195359 ) ) ;
#30671 = CARTESIAN_POINT ( 'NONE',  ( 808.0189434323515343, -374.0891481129647786, -319.0252816721025511 ) ) ;
#30672 = DIRECTION ( 'NONE',  ( 0.000000000000000000, 0.000000000000000000, 1.000000000000000000 ) ) ;
#30673 = CARTESIAN_POINT ( 'NONE',  ( 784.0799538623451781, -419.8055962898681059, 364.6971507214555572 ) ) ;
#30674 = ORIENTED_EDGE ( 'NONE', *, *, #13409, .F. ) ;
#30675 = VECTOR ( 'NONE', #19223, 1000.000000000000000 ) ;
#30676 = CARTESIAN_POINT ( 'NONE',  ( 761.9338519418445230, -158.5328690171417065, -370.4231160770881957 ) ) ;
#30677 = DIRECTION ( 'NONE',  ( -1.000000000000000000, -0.000000000000000000, -0.000000000000000000 ) ) ;
#30678 = CARTESIAN_POINT ( 'NONE',  ( 746.0683387631852383, -259.4419599262322436, 331.3260364891676204 ) ) ;
#30679 = CARTESIAN_POINT ( 'NONE',  ( 785.3141322388236176, -69.72551174932942786, 364.4286716492789537 ) ) ;
#30680 = VERTEX_POINT ( 'NONE', #20884 ) ;
#30681 = AXIS2_PLACEMENT_3D ( 'NONE', #43025, #42584, #38902 ) ;
#30682 = CARTESIAN_POINT ( 'NONE',  ( 804.9511171171677688, -5.805596289869448867, -335.8780910478229202 ) ) ;
#30683 = CARTESIAN_POINT ( 'NONE',  ( 805.1927285166397041, -256.8164208402379245, 341.8018195045277707 ) ) ;
#30684 = CARTESIAN_POINT ( 'NONE',  ( 777.5031285880264704, 1.183579159761269040, -374.9108240113588408 ) ) ;
#30685 = CARTESIAN_POINT ( 'NONE',  ( 999.9999999999992042, -599.0000000000001137, -359.0000000000000000 ) ) ;
#30686 = ORIENTED_EDGE ( 'NONE', *, *, #8131, .T. ) ;
#30687 = CARTESIAN_POINT ( 'NONE',  ( 800.0135310231082713, -182.0891481129654323, -325.0180583372163028 ) ) ;
#30688 = CARTESIAN_POINT ( 'NONE',  ( 757.7880784355613741, -426.0090635724247932, -312.4576283171834916 ) ) ;
#30689 = CONICAL_SURFACE ( 'NONE', #24039, 8.025000000000003908, 0.7853981633974482790 ) ;
#30690 = ADVANCED_FACE ( 'NONE', ( #41931, #6583 ), #2894, .F. ) ;
#30691 = CARTESIAN_POINT ( 'NONE',  ( 774.6858677611749044, -249.7255117493288594, -315.5713283507209894 ) ) ;
#30692 = VECTOR ( 'NONE', #4853, 1000.000000000000000 ) ;
#30694 = CARTESIAN_POINT ( 'NONE',  ( 815.1787889125755555, -246.8965053807777679, 343.7953271457877804 ) ) ;
#30693 = CARTESIAN_POINT ( 'NONE',  ( 745.0891759886404770, -316.2709662947832499, 342.4968714119734159 ) ) ;
#30695 = CARTESIAN_POINT ( 'NONE',  ( 805.9055244015594326, -51.62377810805111267, 315.8990559732753240 ) ) ;
#30696 = CARTESIAN_POINT ( 'NONE',  ( 796.9571628226829034, -215.4636090269709712, -321.2382568024804641 ) ) ;
#30697 = CARTESIAN_POINT ( 'NONE',  ( 755.5713283507202505, -221.3618753856925707, -334.6858677611754729 ) ) ;
#30698 = CARTESIAN_POINT ( 'NONE',  ( 759.9864689768902508, -410.0891481129647218, -354.9819416627836404 ) ) ;
#30699 = CARTESIAN_POINT ( 'NONE',  ( 795.1360043628807261, -260.0891481129650060, 360.2193346964456282 ) ) ;
#30700 = VERTEX_POINT ( 'NONE', #24127 ) ;
#30701 = CARTESIAN_POINT ( 'NONE',  ( 813.1304606946830518, -353.9073299311467053, 352.3570229623690580 ) ) ;
#30702 = CARTESIAN_POINT ( 'NONE',  ( 795.2725662613897839, 16.45630643248849267, -314.1785221222716586 ) ) ;
#30703 = CARTESIAN_POINT ( 'NONE',  ( 805.6418435158337843, -5.463609026971610660, -363.8556311672236916 ) ) ;
#30704 = CARTESIAN_POINT ( 'NONE',  ( 779.2785047387700388, 16.45630643248848912, 314.0977342670951202 ) ) ;
#30705 = LINE ( 'NONE', #10142, #12697 ) ;
#30706 = CARTESIAN_POINT ( 'NONE',  ( 779.4763451958990572, -224.7363362996982232, 365.0264073115438919 ) ) ;
#30707 = CARTESIAN_POINT ( 'NONE',  ( 778.1981804954714335, -82.27096629478388934, 314.8072714833589885 ) ) ;
#30708 = CARTESIAN_POINT ( 'NONE',  ( 805.6418435158337843, -437.4636090269703459, -363.8556311672236916 ) ) ;
#30709 = CARTESIAN_POINT ( 'NONE',  ( 745.7998596910086917, -53.36187538569310362, -332.5602148656461168 ) ) ;
#30710 = CARTESIAN_POINT ( 'NONE',  ( 756.7813123517142913, -259.9874144716869182, 329.9779781133712504 ) ) ;
#30711 = VECTOR ( 'NONE', #25234, 1000.000000000000000 ) ;
#30712 = CARTESIAN_POINT ( 'NONE',  ( 785.3141322388236176, -429.7255117493282910, -364.4286716492789537 ) ) ;
#30713 = CARTESIAN_POINT ( 'NONE',  ( 756.5762568750052424, -27.18005720387500901, -348.7366044899774238 ) ) ;
#30714 = CARTESIAN_POINT ( 'NONE',  ( 791.0478386215596629, -21.82724539060792424, 306.7653713866226326 ) ) ;
#30715 = DIRECTION ( 'NONE',  ( -1.000000000000000000, -0.000000000000000000, 0.000000000000000000 ) ) ;
#30716 = CARTESIAN_POINT ( 'NONE',  ( 790.0220218866281812, -295.0999726633343698, -363.2186876482849129 ) ) ;
#30718 = AXIS2_PLACEMENT_3D ( 'NONE', #19064, #19492, #43982 ) ;
#30717 = CARTESIAN_POINT ( 'NONE',  ( 777.5031285880264704, -214.8164208402380666, -374.9108240113588408 ) ) ;
#30719 = CARTESIAN_POINT ( 'NONE',  ( 811.0346526505616112, -86.63460265842023489, 323.0537975583477532 ) ) ;
#30720 = CARTESIAN_POINT ( 'NONE',  ( 814.9108240113580450, -160.2709662947836762, 337.5031285880265273 ) ) ;
#30721 = DIRECTION ( 'NONE',  ( -0.000000000000000000, 0.3826834323650978309, 0.9238795325112835188 ) ) ;
#30722 = CIRCLE ( 'NONE', #12923, 10.00000000000000888 ) ;
#30723 = CARTESIAN_POINT ( 'NONE',  ( -338.8365100919713200, 258.0940000000001078, -199.9999999999917861 ) ) ;
#30724 = CARTESIAN_POINT ( 'NONE',  ( 815.1787889125755555, -246.8965053807777679, -343.7953271457877804 ) ) ;
#30725 = CARTESIAN_POINT ( 'NONE',  ( 795.8262568251477660, -406.3726999360612808, 308.3538107759623585 ) ) ;
#30726 = CARTESIAN_POINT ( 'NONE',  ( 772.5602148656447525, -273.7255117493288026, -305.7998596910095443 ) ) ;
#30727 = LINE ( 'NONE', #34163, #33136 ) ;
#30728 = CARTESIAN_POINT ( 'NONE',  ( 813.1304606946830518, -401.9073299311463643, 352.3570229623690580 ) ) ;
#30729 = CARTESIAN_POINT ( 'NONE',  ( 782.5225473063383106, -22.27096629478410605, 375.2698199232970637 ) ) ;
#30730 = CARTESIAN_POINT ( 'NONE',  ( 781.8018195045266339, -358.2709662947829088, -365.1927285166406705 ) ) ;
#30731 = CARTESIAN_POINT ( 'NONE',  ( 796.7845633553578182, -9.623778108051251223, 358.5707757039688204 ) ) ;
#30732 = CARTESIAN_POINT ( 'NONE',  ( 752.4576283171824116, -45.07832356259660145, -317.7880784355627952 ) ) ;
#30733 = CARTESIAN_POINT ( 'NONE',  ( 780.5290396650775619, -156.3510508353235480, -365.2837595273619513 ) ) ;
#30734 = CARTESIAN_POINT ( 'NONE',  ( 749.8865473780648472, -164.5328690171416781, 322.1177392798429082 ) ) ;
#30735 = CARTESIAN_POINT ( 'NONE',  ( -26.63011601220122060, -512.9681489794448908, -339.9999999999999432 ) ) ;
#30736 = ORIENTED_EDGE ( 'NONE', *, *, #3230, .T. ) ;
#30737 = CARTESIAN_POINT ( 'NONE',  ( 781.8018195045266339, -46.27096629478404566, -365.1927285166406705 ) ) ;
#30738 = CARTESIAN_POINT ( 'NONE',  ( 804.1601925771018387, -175.4419599262325562, -346.5483106153029098 ) ) ;
#30739 = CARTESIAN_POINT ( 'NONE',  ( 768.0187753319979720, -152.6346026584200786, 318.0580252608186242 ) ) ;
#30740 = CARTESIAN_POINT ( 'NONE',  ( 758.0141637701419768, -15.07832356259669560, -367.2620300519063790 ) ) ;
#30741 = CARTESIAN_POINT ( 'NONE',  ( 778.2165204200184689, -286.8164208402378677, 364.9363028652563230 ) ) ;
#30742 = FACE_OUTER_BOUND ( 'NONE', #16134, .T. ) ;
#30743 = ORIENTED_EDGE ( 'NONE', *, *, #38265, .F. ) ;
#30744 = CARTESIAN_POINT ( 'NONE',  ( 789.9200121543843807, -25.98741447168755769, 317.0176451133914384 ) ) ;
#30745 = CARTESIAN_POINT ( 'NONE',  ( 786.2694204179717872, -261.2817908451526705, -305.1769319972829067 ) ) ;
#30746 = PRODUCT_CONTEXT ( 'NONE', #43487, 'mechanical' ) ;
#30747 = VECTOR ( 'NONE', #29521, 1000.000000000000000 ) ;
#30748 = CARTESIAN_POINT ( 'NONE',  ( 754.9967657858570647, -217.5436935675107293, 365.0032342141425943 ) ) ;
#30749 = CARTESIAN_POINT ( 'NONE',  ( 754.7162404726377645, -350.7363362996978253, 339.4709603349214717 ) ) ;
#30750 = CARTESIAN_POINT ( 'NONE',  ( 779.4709603349208464, -432.3510508353226669, 314.7162404726379918 ) ) ;
#30751 = ORIENTED_EDGE ( 'NONE', *, *, #24955, .F. ) ;
#30753 = VECTOR ( 'NONE', #26815, 1000.000000000000000 ) ;
#30752 = CARTESIAN_POINT ( 'NONE',  ( 763.0428371773158460, -131.4636090269711985, -358.7617431975195359 ) ) ;
#30754 = CARTESIAN_POINT ( 'NONE',  ( 791.9812246680005501, -116.6346026584201780, -361.9419747391813189 ) ) ;
#30755 = CARTESIAN_POINT ( 'NONE',  ( 804.4286716492782716, -329.3618753856922581, -345.3141322388244703 ) ) ;
#30756 = ORIENTED_EDGE ( 'NONE', *, *, #45316, .F. ) ;
#30757 = CARTESIAN_POINT ( 'NONE',  ( 755.5713283507202505, -413.3618753856920307, -334.6858677611754729 ) ) ;
#30758 = VECTOR ( 'NONE', #17120, 1000.000000000000114 ) ;
#30759 = CARTESIAN_POINT ( 'NONE',  ( 756.7813123517142913, -283.9874144716867477, 329.9779781133712504 ) ) ;
#30760 = CARTESIAN_POINT ( 'NONE',  ( 793.4578903520955464, -453.6923923018891855, 372.2744472307925321 ) ) ;
#30761 = LINE ( 'NONE', #2569, #5660 ) ;
#30762 = AXIS2_PLACEMENT_3D ( 'NONE', #14234, #37804, #28303 ) ;
#30763 = CARTESIAN_POINT ( 'NONE',  ( 779.4763451958990572, -128.7363362996984790, 365.0264073115438919 ) ) ;
#30764 = CARTESIAN_POINT ( 'NONE',  ( -879.9999999999992042, 260.0000000000002274, -179.9999999999999716 ) ) ;
#30765 = ORIENTED_EDGE ( 'NONE', *, *, #1009, .T. ) ;
#30766 = CARTESIAN_POINT ( 'NONE',  ( 771.3260364891663130, -331.6454272087888171, -306.0683387631859773 ) ) ;
#30767 = CARTESIAN_POINT ( 'NONE',  ( 791.0478386215596629, -189.8272453906073736, 306.7653713866226326 ) ) ;
#30768 = CARTESIAN_POINT ( 'NONE',  ( 804.6798772138708955, -327.7255117493285184, -334.6312213355107019 ) ) ;
#30769 = CARTESIAN_POINT ( 'NONE',  ( 831.1634899080286232, 259.9999999999998863, -199.9999999999999432 ) ) ;
#30770 = CARTESIAN_POINT ( 'NONE',  ( 766.0291762391763086, -178.9181544815165239, -360.7704444035551319 ) ) ;
#30771 = CARTESIAN_POINT ( 'NONE',  ( 813.1304606946830518, -41.90732993114767169, 352.3570229623690580 ) ) ;
#30772 = CARTESIAN_POINT ( 'NONE',  ( 798.5757817331792694, -452.9681489794448339, 357.1584183591081683 ) ) ;
#30773 = CARTESIAN_POINT ( 'NONE',  ( 796.9462024416508257, -396.4527844766010958, -308.9653473494370246 ) ) ;
#30774 = DIRECTION ( 'NONE',  ( 1.000000000000000000, 0.000000000000000000, 0.000000000000000000 ) ) ;
#30775 = AXIS2_PLACEMENT_3D ( 'NONE', #23186, #40996, #11757 ) ;
#30776 = CARTESIAN_POINT ( 'NONE',  ( 810.4231160770870019, -336.5545181178796952, 321.9338519418446936 ) ) ;
#30777 = DIRECTION ( 'NONE',  ( 0.000000000000000000, 0.000000000000000000, 1.000000000000000000 ) ) ;
#30778 = CARTESIAN_POINT ( 'NONE',  ( 747.2067596250078623, -291.1800572038741848, 352.2312462859687230 ) ) ;
#30779 = CARTESIAN_POINT ( 'NONE',  ( 751.9810565676468741, -26.08914811296592262, -360.9747183278973921 ) ) ;
#30780 = CARTESIAN_POINT ( 'NONE',  ( 765.0180583372156207, -264.9982390220561115, -360.0135310231089534 ) ) ;
#30781 = DIRECTION ( 'NONE',  ( -1.000000000000000000, -0.000000000000000000, -0.000000000000000000 ) ) ;
#30782 = CARTESIAN_POINT ( 'NONE',  ( 778.2165204200184689, -382.8164208402374697, 364.9363028652563230 ) ) ;
#30783 = CARTESIAN_POINT ( 'NONE',  ( 804.6971507214547046, -171.2817908451529263, 344.0799538623459739 ) ) ;
#30784 = CARTESIAN_POINT ( 'NONE',  ( 779.4709603349208464, -48.35105083532386061, -314.7162404726379918 ) ) ;
#30785 = CARTESIAN_POINT ( 'NONE',  ( 788.7631598425961101, -49.44195992623295410, 305.7194118038759143 ) ) ;
#30786 = CARTESIAN_POINT ( 'NONE',  ( 797.6776695296629214, -355.5436935675103882, 357.6776695296636603 ) ) ;
#30787 = AXIS2_PLACEMENT_3D ( 'NONE', #36358, #18821, #18593 ) ;
#30788 = FILL_AREA_STYLE ('',( #42091 ) ) ;
#30789 = CARTESIAN_POINT ( 'NONE',  ( 800.0135310231082713, -446.0891481129646081, 325.0180583372163028 ) ) ;
#30790 = VERTEX_POINT ( 'NONE', #41243 ) ;
#30791 = CARTESIAN_POINT ( 'NONE',  ( 756.3353852180819104, -53.90732993114765037, -331.1735550268788302 ) ) ;
#30792 = CARTESIAN_POINT ( 'NONE',  ( 805.1016975059191054, -366.8965053807773984, -343.0745993439771837 ) ) ;
#30794 = CARTESIAN_POINT ( 'NONE',  ( 804.6798772138710092, -207.7255117493289731, 334.6312213355106451 ) ) ;
#30793 = CARTESIAN_POINT ( 'NONE',  ( 759.7806653035534055, -198.9982390220562252, 324.8639956371180801 ) ) ;
#30795 = CARTESIAN_POINT ( 'NONE',  ( 768.8385539511368734, -359.2601417444137724, -306.4236121716840557 ) ) ;
#30796 = CARTESIAN_POINT ( 'NONE',  ( 769.9999999999992042, 178.9475563372491251, 360.0000000000000000 ) ) ;
#30797 = VERTEX_POINT ( 'NONE', #17203 ) ;
#30798 = CARTESIAN_POINT ( 'NONE',  ( 768.0187753319979720, -392.6346026584193396, 318.0580252608186242 ) ) ;
#30799 = EDGE_LOOP ( 'NONE', ( #36926, #41712, #33795, #25063 ) ) ;
#30800 = CARTESIAN_POINT ( 'NONE',  ( 799.9999999999993179, 205.0000000000000568, -319.9999999999999432 ) ) ;
#30801 = CARTESIAN_POINT ( 'NONE',  ( 745.7998596910086917, -221.3618753856925707, -332.5602148656461168 ) ) ;
#30802 = CARTESIAN_POINT ( 'NONE',  ( 745.0891759886404770, -100.2709662947838609, 342.4968714119734159 ) ) ;
#30803 = VERTEX_POINT ( 'NONE', #7048 ) ;
#30804 = CARTESIAN_POINT ( 'NONE',  ( 754.8072714833583632, -196.8164208402380950, -338.1981804954721156 ) ) ;
#30805 = ORIENTED_EDGE ( 'NONE', *, *, #28125, .T. ) ;
#30806 = CARTESIAN_POINT ( 'NONE',  ( 803.6646147819161570, -329.9073299311467053, -348.8264449731210561 ) ) ;
#30807 = CARTESIAN_POINT ( 'NONE',  ( 798.5707757039680246, -461.4636090269701754, -356.7845633553585003 ) ) ;
#30808 = CARTESIAN_POINT ( 'NONE',  ( 773.3843516231979720, -181.4419599262325278, 364.4086373105754433 ) ) ;
#30810 = DIRECTION ( 'NONE',  ( 1.000000000000000000, -0.000000000000000000, -0.000000000000000000 ) ) ;
#30809 = LINE ( 'NONE', #44903, #30661 ) ;
#30811 = LINE ( 'NONE', #44905, #23540 ) ;
#30812 = ORIENTED_EDGE ( 'NONE', *, *, #42786, .T. ) ;
#30813 = CARTESIAN_POINT ( 'NONE',  ( 778.1981804954714335, 13.72903370521577138, -314.8072714833589885 ) ) ;
#30814 = DIRECTION ( 'NONE',  ( 1.000000000000000000, 0.000000000000000000, -0.000000000000000000 ) ) ;
#30815 = DIRECTION ( 'NONE',  ( -0.000000000000000000, 1.000000000000000000, -0.000000000000000000 ) ) ;
#30816 = CARTESIAN_POINT ( 'NONE',  ( 752.7379699480933368, -252.0090635724254184, -361.9858362298580232 ) ) ;
#30817 = CARTESIAN_POINT ( 'NONE',  ( 813.5763878283155464, -99.82724539060768620, 351.1614460488615350 ) ) ;
#30818 = AXIS2_PLACEMENT_3D ( 'NONE', #13877, #37896, #10175 ) ;
#30820 = CARTESIAN_POINT ( 'NONE',  ( 803.4237431249931660, -207.1800572038744406, -331.2633955100225194 ) ) ;
#30819 = DIRECTION ( 'NONE',  ( 0.000000000000000000, 0.000000000000000000, 1.000000000000000000 ) ) ;
#30821 = CARTESIAN_POINT ( 'NONE',  ( 756.1348686366196716, -377.2601417444137724, -347.5531968255698416 ) ) ;
#30822 = CARTESIAN_POINT ( 'NONE',  ( 812.3518521366052028, -241.0999726633345119, -326.5853460496235243 ) ) ;
#30823 = DIRECTION ( 'NONE',  ( -0.000000000000000000, 1.000000000000000000, -0.000000000000000000 ) ) ;
#30824 = CARTESIAN_POINT ( 'NONE',  ( 998.9999999999992042, 249.9999999999998863, -359.0000000000000000 ) ) ;
#30825 = CARTESIAN_POINT ( 'NONE',  ( 796.1575198192839480, -78.00906357242591582, -359.4546378042384163 ) ) ;
#30826 = CARTESIAN_POINT ( 'NONE',  ( 755.5913626894240451, -421.6454272087885329, 346.6156483768012890 ) ) ;
#30827 = ADVANCED_FACE ( 'NONE', ( #23887 ), #6121, .T. ) ;
#30828 = CARTESIAN_POINT ( 'NONE',  ( 998.9999999999992042, 479.9999999999999432, 360.0000000000000000 ) ) ;
#30829 = CARTESIAN_POINT ( 'NONE',  ( 787.4397851343537695, -261.7255117493288026, -374.2001403089903988 ) ) ;
#30830 = DIRECTION ( 'NONE',  ( 1.644774851296528363E-16, -1.000000000000000000, -0.000000000000000000 ) ) ;
#30831 = CARTESIAN_POINT ( 'NONE',  ( 794.9999999999993179, 205.0000000000000568, -255.0000000000000000 ) ) ;
#30832 = CARTESIAN_POINT ( 'NONE',  ( 794.9819416627830151, -36.99823902205679360, -319.9864689768909898 ) ) ;
#30833 = CARTESIAN_POINT ( 'NONE',  ( 783.7953271457878373, -224.1908817542436623, 375.1787889125761239 ) ) ;
#30834 = CARTESIAN_POINT ( 'NONE',  ( 745.1769319972822814, -161.8055962898689870, -346.2694204179732083 ) ) ;
#30835 = CARTESIAN_POINT ( 'NONE',  ( 751.6929314249748586, -198.9982390220562252, 318.8095938919659034 ) ) ;
#30836 = CARTESIAN_POINT ( 'NONE',  ( 814.9108240113580450, -424.2709662947829088, -337.5031285880265273 ) ) ;
#30837 = CARTESIAN_POINT ( 'NONE',  ( -26.63011601220122060, -544.8427095258973623, -350.0000000000000000 ) ) ;
#30838 = CARTESIAN_POINT ( 'NONE',  ( 785.3687786644884454, -275.3618753856923149, 315.3201227861279676 ) ) ;
#30839 = CARTESIAN_POINT ( 'NONE',  ( 799.2566176426618085, -72.00906357242594424, 324.0069404352559559 ) ) ;
#30840 = CARTESIAN_POINT ( 'NONE',  ( 781.7834795799800531, -418.8164208402374129, -315.0636971347436202 ) ) ;
#30841 = DIRECTION ( 'NONE',  ( 0.000000000000000000, 0.000000000000000000, 1.000000000000000000 ) ) ;
#30842 = LINE ( 'NONE', #35216, #38750 ) ;
#30844 = CARTESIAN_POINT ( 'NONE',  ( 755.3201227861273992, -339.7255117493285184, 345.3687786644892981 ) ) ;
#30843 = CARTESIAN_POINT ( 'NONE',  ( 795.9930595647434757, -75.07832356259649487, 320.7433823573372820 ) ) ;
#30845 = ORIENTED_EDGE ( 'NONE', *, *, #7440, .F. ) ;
#30846 = EDGE_CURVE ( 'NONE', #6307, #37952, #10057, .T. ) ;
#30847 = CARTESIAN_POINT ( 'NONE',  ( 804.1601925771018387, -271.4419599262321867, -346.5483106153029098 ) ) ;
#30848 = CARTESIAN_POINT ( 'NONE',  ( 756.3353852180819104, -125.9073299311474159, -331.1735550268788302 ) ) ;
#30849 = CARTESIAN_POINT ( 'NONE',  ( 794.9819416627830151, -60.99823902205671544, 319.9864689768909898 ) ) ;
#30850 = CARTESIAN_POINT ( 'NONE',  ( 813.2346286133761168, -269.2601417444139997, -328.9521613784389160 ) ) ;
#30851 = FACE_OUTER_BOUND ( 'NONE', #9780, .T. ) ;
#30852 = CARTESIAN_POINT ( 'NONE',  ( 786.2056067578752163, -371.8055962898682765, 374.4686193811670023 ) ) ;
#30853 = EDGE_LOOP ( 'NONE', ( #12685, #32425, #32802, #10687 ) ) ;
#30854 = CARTESIAN_POINT ( 'NONE',  ( 755.3201227861273992, -291.7255117493285752, 345.3687786644892981 ) ) ;
#30855 = VECTOR ( 'NONE', #34661, 1000.000000000000000 ) ;
#30856 = CARTESIAN_POINT ( 'NONE',  ( 798.7617431975189675, -27.62377810805120149, -323.0428371773161871 ) ) ;
#30857 = CARTESIAN_POINT ( 'NONE',  ( 768.0187753319979720, -176.6346026584199933, -318.0580252608186242 ) ) ;
#30858 = CARTESIAN_POINT ( 'NONE',  ( 803.6646147819161570, -377.9073299311466485, 348.8264449731210561 ) ) ;
#30859 = EDGE_CURVE ( 'NONE', #16721, #6763, #16614, .T. ) ;
#30860 = CARTESIAN_POINT ( 'NONE',  ( 810.7187646348534145, -114.4527844766020053, -356.7737145352016341 ) ) ;
#30861 = CARTESIAN_POINT ( 'NONE',  ( 791.9812246680005501, -116.6346026584201780, -361.9419747391813189 ) ) ;
#30862 = EDGE_LOOP ( 'NONE', ( #38791, #25689, #19111, #40582 ) ) ;
#30863 = CARTESIAN_POINT ( 'NONE',  ( 769.0155153010367712, -34.37269993606243901, -362.7791456095907279 ) ) ;
#30864 = CARTESIAN_POINT ( 'NONE',  ( 775.8780910478218402, -369.2817908451523294, -364.9511171171680530 ) ) ;
#30866 = CARTESIAN_POINT ( 'NONE',  ( 800.9840315886518738, -412.9181544815157281, 354.1144889064786412 ) ) ;
#30865 = CARTESIAN_POINT ( 'NONE',  ( 803.6646147819161570, -89.90732993114750116, 348.8264449731210561 ) ) ;
#30869 = CARTESIAN_POINT ( 'NONE',  ( 801.9858362298568863, -363.0783235625955854, 312.7379699480935642 ) ) ;
#30868 = CARTESIAN_POINT ( 'NONE',  ( 919.9999999999993179, 219.9999999999998863, 360.0000000000000000 ) ) ;
#30867 = CARTESIAN_POINT ( 'NONE',  ( 784.4999999999993179, -501.1515549466498669, -368.0974687824633520 ) ) ;
#30870 = CARTESIAN_POINT ( 'NONE',  ( 779.4763451958990572, -344.7363362996978253, -365.0264073115438919 ) ) ;
#30871 = CARTESIAN_POINT ( 'NONE',  ( 755.5713283507202505, -365.3618753856920875, -334.6858677611754729 ) ) ;
#30872 = CARTESIAN_POINT ( 'NONE',  ( 804.1009440267234822, -143.4636090269711701, -314.0944755984392600 ) ) ;
#30873 = CARTESIAN_POINT ( 'NONE',  ( 752.7379699480933368, -12.00906357242613609, 361.9858362298580232 ) ) ;
#30875 = CARTESIAN_POINT ( 'NONE',  ( 939.9999999999992042, 47.45399382421949497, 201.9999999999999432 ) ) ;
#30874 = DIRECTION ( 'NONE',  ( 0.000000000000000000, -1.000000000000000000, 0.000000000000000000 ) ) ;
#30876 = CARTESIAN_POINT ( 'NONE',  ( 759.2295555964440155, -256.1692326535049915, -353.9708237608231229 ) ) ;
#30877 = ADVANCED_FACE ( 'NONE', ( #38454 ), #44708, .F. ) ;
#30878 = CARTESIAN_POINT ( 'NONE',  ( 788.6739635108323228, -151.6454272087892718, -373.9316612368139090 ) ) ;
#30879 = CARTESIAN_POINT ( 'NONE',  ( 928.0249999999991815, 154.9999999999998863, 339.9999999999999432 ) ) ;
#30880 = CYLINDRICAL_SURFACE ( 'NONE', #7573, 2.749999999999863665 ) ;
#30881 = CARTESIAN_POINT ( 'NONE',  ( 802.9823548866075953, -337.0999726633342561, 330.0799878456151077 ) ) ;
#30882 = EDGE_CURVE ( 'NONE', #25691, #28582, #20211, .T. ) ;
#30883 = ORIENTED_EDGE ( 'NONE', *, *, #43119, .T. ) ;
#30884 = CARTESIAN_POINT ( 'NONE',  ( 814.2805881961230625, -313.6454272087888171, 331.2368401574024119 ) ) ;
#30885 = CARTESIAN_POINT ( 'NONE',  ( 814.9108240113580450, -160.2709662947836762, -337.5031285880265273 ) ) ;
#30886 = CARTESIAN_POINT ( 'NONE',  ( 989.9999999999992042, -590.0000000000001137, -201.9999999999998579 ) ) ;
#30887 = CONICAL_SURFACE ( 'NONE', #40518, 8.024999999999948841, 0.7853981633963380560 ) ;
#30888 = CARTESIAN_POINT ( 'NONE',  ( 814.8207195650702488, -98.19088175424404596, 336.2433038121456548 ) ) ;
#30889 = CARTESIAN_POINT ( 'NONE',  ( 747.2067596250078623, -291.1800572038741848, -352.2312462859687230 ) ) ;
#30890 = CARTESIAN_POINT ( 'NONE',  ( 187.1337867209877857, 56.78581973499402835, -212.6378164459127049 ) ) ;
#30891 = FACE_OUTER_BOUND ( 'NONE', #3069, .T. ) ;
#30892 = CARTESIAN_POINT ( 'NONE',  ( 803.6646147819161570, -161.9073299311472454, 348.8264449731210561 ) ) ;
#30893 = EDGE_LOOP ( 'NONE', ( #39331, #30751, #42330, #25216 ) ) ;
#30894 = CARTESIAN_POINT ( 'NONE',  ( 754.3581564841646241, -425.4636090269703459, 316.1443688327762516 ) ) ;
#30895 = CARTESIAN_POINT ( 'NONE',  ( 800.1688906516307043, -394.1692326535045368, -369.0717654672308186 ) ) ;
#30896 = CARTESIAN_POINT ( 'NONE',  ( 759.0252816721024374, -120.9982390220565378, -368.0189434323527280 ) ) ;
#30897 = EDGE_CURVE ( 'NONE', #11754, #34011, #28052, .T. ) ;
#30898 = CARTESIAN_POINT ( 'NONE',  ( 793.0897708529556667, -54.55451811788054783, 361.3366627262616362 ) ) ;
#30899 = CARTESIAN_POINT ( 'NONE',  ( 777.4774526936600978, -394.2709662947827951, -304.7301800767027657 ) ) ;
#30900 = LINE ( 'NONE', #13350, #36487 ) ;
#30901 = CARTESIAN_POINT ( 'NONE',  ( 776.9566956441375396, -420.8965053807772279, 364.8461984189686405 ) ) ;
#30902 = ORIENTED_EDGE ( 'NONE', *, *, #27224, .T. ) ;
#30903 = EDGE_CURVE ( 'NONE', #9887, #11032, #12917, .T. ) ;
#30904 = CARTESIAN_POINT ( 'NONE',  ( 788.7631598425961101, -145.4419599262326699, -305.7194118038759143 ) ) ;
#30905 = SURFACE_SIDE_STYLE ('',( #42434 ) ) ;
#30906 = CARTESIAN_POINT ( 'NONE',  ( 768.8385539511368734, -287.2601417444140566, 306.4236121716840557 ) ) ;
#30907 = CARTESIAN_POINT ( 'NONE',  ( 778.2165204200184689, -94.81642084023843609, 364.9363028652563230 ) ) ;
#30908 = ORIENTED_EDGE ( 'NONE', *, *, #28035, .T. ) ;
#30909 = ADVANCED_FACE ( 'NONE', ( #41466 ), #16762, .T. ) ;
#30910 = CARTESIAN_POINT ( 'NONE',  ( 771.1735550268778070, -273.1800572038742985, 316.3353852180827630 ) ) ;
#30911 = EDGE_CURVE ( 'NONE', #40516, #16782, #30842, .T. ) ;
#30912 = CARTESIAN_POINT ( 'NONE',  ( 808.3070685750230950, -18.99823902205683979, -361.1904061080339261 ) ) ;
#30913 = DIRECTION ( 'NONE',  ( -0.000000000000000000, -1.000000000000000000, -0.000000000000000000 ) ) ;
#30914 = ORIENTED_EDGE ( 'NONE', *, *, #9097, .F. ) ;
#30915 = EDGE_LOOP ( 'NONE', ( #43915, #29048, #25786, #22950 ) ) ;
#30916 = CARTESIAN_POINT ( 'NONE',  ( 781.2370466360911223, -404.7363362996975980, -304.9990715423533629 ) ) ;
#30917 = CIRCLE ( 'NONE', #8092, 10.00000000000000888 ) ;
#30918 = CARTESIAN_POINT ( 'NONE',  ( 797.6776695296629214, -259.5436935675106156, -357.6776695296636603 ) ) ;
#30920 = CARTESIAN_POINT ( 'NONE',  ( 766.5853460496234675, -253.9874144716868329, 372.3518521366060554 ) ) ;
#30919 = CARTESIAN_POINT ( 'NONE',  ( 777.4774526936600978, -346.2709662947830225, 304.7301800767028226 ) ) ;
#30921 = CARTESIAN_POINT ( 'NONE',  ( 801.9858362298568863, -51.07832356259657303, 312.7379699480935642 ) ) ;
#30922 = CARTESIAN_POINT ( 'NONE',  ( 790.9844846989617508, -262.3726999360617924, -317.2208543904092721 ) ) ;
#30923 = CARTESIAN_POINT ( 'NONE',  ( 774.6858677611749044, -225.7255117493289163, -315.5713283507209894 ) ) ;
#30924 = CARTESIAN_POINT ( 'NONE',  ( 765.0180583372156207, -432.9982390220555999, -360.0135310231089534 ) ) ;
#30925 = ADVANCED_FACE ( 'NONE', ( #30610 ), #27154, .F. ) ;
#30926 = CARTESIAN_POINT ( 'NONE',  ( 765.0180583372156207, -240.9982390220561683, 360.0135310231089534 ) ) ;
#30927 = ORIENTED_EDGE ( 'NONE', *, *, #9182, .T. ) ;
#30928 = CARTESIAN_POINT ( 'NONE',  ( 751.6929314249748586, -342.9982390220557136, 318.8095938919659034 ) ) ;
#30929 = DIRECTION ( 'NONE',  ( -0.000000000000000000, 1.000000000000000000, -0.000000000000000000 ) ) ;
#30930 = EDGE_CURVE ( 'NONE', #26699, #41138, #18834, .T. ) ;
#30931 = CARTESIAN_POINT ( 'NONE',  ( 781.2370466360911223, -44.73633629969875614, -304.9990715423533629 ) ) ;
#30932 = CARTESIAN_POINT ( 'NONE',  ( 781.4876528434626834, 16.45630643248849267, 313.8857452882203347 ) ) ;
#30933 = CARTESIAN_POINT ( 'NONE',  ( 311.1634899080286232, 258.0939999999999941, -199.9999999999963336 ) ) ;
#30934 = CARTESIAN_POINT ( 'NONE',  ( 804.6971507214547046, -243.2817908451526705, 344.0799538623459739 ) ) ;
#30935 = CARTESIAN_POINT ( 'NONE',  ( 764.8639956371174549, -104.0891481129656881, 319.7806653035542013 ) ) ;
#30936 = ORIENTED_EDGE ( 'NONE', *, *, #17349, .T. ) ;
#30937 = CARTESIAN_POINT ( 'NONE',  ( 780.5236548040995785, -20.73633629969883430, -314.9735926884559944 ) ) ;
#30938 = CARTESIAN_POINT ( 'NONE',  ( 782.4968714119720516, -82.81642084023846451, -305.0891759886411023 ) ) ;
#30939 = CARTESIAN_POINT ( 'NONE',  ( 773.3843516231979720, -301.4419599262320730, 364.4086373105754433 ) ) ;
#30940 = CARTESIAN_POINT ( 'NONE',  ( 788.8264449731200330, -429.1800572038737869, -363.6646147819171233 ) ) ;
#30941 = CARTESIAN_POINT ( 'NONE',  ( 800.0135310231082713, -38.08914811296587999, -325.0180583372163028 ) ) ;
#30942 = CARTESIAN_POINT ( 'NONE',  ( 814.4686193811664907, -3.281790845153435221, 346.2056067578752732 ) ) ;
#30943 = CARTESIAN_POINT ( 'NONE',  ( -190.7583438952259485, 394.6698570112193920, -224.9999999999999716 ) ) ;
#30944 = CARTESIAN_POINT ( 'NONE',  ( 749.2812353651451076, -198.4527844766017495, -323.2262854647983090 ) ) ;
#30945 = CARTESIAN_POINT ( 'NONE',  ( 796.9462024416508257, -84.45278447660206211, 308.9653473494370246 ) ) ;
#30946 = CARTESIAN_POINT ( 'NONE',  ( 787.4397851343537695, -189.7255117493290300, 374.2001403089903988 ) ) ;
#30947 = LINE ( 'NONE', #41566, #40927 ) ;
#30948 = DIRECTION ( 'NONE',  ( 1.000000000000000000, 0.000000000000000000, 0.000000000000000000 ) ) ;
#30949 = CARTESIAN_POINT ( 'NONE',  ( 756.1443688327750579, -261.6237781080504305, -314.3581564841659315 ) ) ;
#30950 = ADVANCED_FACE ( 'NONE', ( #3113 ), #16985, .F. ) ;
#30951 = CARTESIAN_POINT ( 'NONE',  ( 793.5525998758768083, -415.0999726633340288, 372.6845335610516941 ) ) ;
#30952 = CARTESIAN_POINT ( 'NONE',  ( 815.2698199232961542, -280.8164208402378677, -342.5225473063383106 ) ) ;
#30953 = CARTESIAN_POINT ( 'NONE',  ( 759.9999999999992042, -512.9681489794448908, -309.9999999999998863 ) ) ;
#30954 = CARTESIAN_POINT ( 'NONE',  ( 777.5031285880264704, -406.8164208402375266, 374.9108240113588408 ) ) ;
#30955 = CARTESIAN_POINT ( 'NONE',  ( 804.7487373415286811, -19.54369356751139364, 364.7487373415288516 ) ) ;
#30956 = CARTESIAN_POINT ( 'NONE',  ( 765.0180583372156207, -360.9982390220557704, -360.0135310231089534 ) ) ;
#30957 = ADVANCED_FACE ( 'NONE', ( #45160, #27595 ), #27836, .F. ) ;
#30958 = CARTESIAN_POINT ( 'NONE',  ( 803.2186876482843445, -31.98741447168754348, 350.0220218866286928 ) ) ;
#30959 = CARTESIAN_POINT ( 'NONE',  ( 749.8865473780648472, -44.53286901714205470, -322.1177392798429082 ) ) ;
#30960 = CARTESIAN_POINT ( 'NONE',  ( 798.7617431975189675, -147.6237781080508285, -323.0428371773161871 ) ) ;
#30961 = CARTESIAN_POINT ( 'NONE',  ( 764.3348316497523456, -166.7146871989598367, 308.6759233522265617 ) ) ;
#30962 = CARTESIAN_POINT ( 'NONE',  ( 805.1927285166399315, 7.183579159761249500, 341.8018195045277707 ) ) ;
#30963 = ORIENTED_EDGE ( 'NONE', *, *, #30634, .F. ) ;
#30964 = CARTESIAN_POINT ( 'NONE',  ( 759.9864689768902508, -74.08914811296577341, -354.9819416627836404 ) ) ;
#30965 = CARTESIAN_POINT ( 'NONE',  ( 795.9930595647434757, -171.0783235625962106, -320.7433823573372820 ) ) ;
#30966 = CARTESIAN_POINT ( 'NONE',  ( 800.2193346964447755, -162.9982390220563673, 355.1360043628815788 ) ) ;
#30967 = CARTESIAN_POINT ( 'NONE',  ( 778.7502325331095108, -0.3510508353240099355, -304.6391490659818828 ) ) ;
#30968 = CARTESIAN_POINT ( 'NONE',  ( 788.7366044899766848, -299.9073299311468759, 316.5762568750059813 ) ) ;
#30969 = CARTESIAN_POINT ( 'NONE',  ( -180.7583438952258348, 394.6698570112193920, -244.9999999999999716 ) ) ;
#30970 = ORIENTED_EDGE ( 'NONE', *, *, #30056, .F. ) ;
#30971 = CARTESIAN_POINT ( 'NONE',  ( 775.9200461376533440, 0.1944037101305369775, 315.3028492785443291 ) ) ;
#30972 = CARTESIAN_POINT ( 'NONE',  ( 778.7629533639073998, -296.7363362996979390, -375.0009284576466371 ) ) ;
#30973 = CARTESIAN_POINT ( 'NONE',  ( 782.4968714119720516, -250.8164208402379245, 305.0891759886411023 ) ) ;
#30974 = CARTESIAN_POINT ( 'NONE',  ( 773.4516893846965786, -331.6454272087888171, 315.8398074228977066 ) ) ;
#30975 = CARTESIAN_POINT ( 'NONE',  ( 775.9200461376533440, -431.8055962898681059, 315.3028492785443291 ) ) ;
#30976 = CARTESIAN_POINT ( 'NONE',  ( 780.5236548040995785, -164.7363362996983938, -314.9735926884559944 ) ) ;
#30977 = CARTESIAN_POINT ( 'NONE',  ( 754.8072714833581358, -124.8164208402383508, -338.1981804954720587 ) ) ;
#30978 = CARTESIAN_POINT ( 'NONE',  ( 792.1044303154646968, -324.4527844766013231, -317.8323909638837677 ) ) ;
#30979 = ORIENTED_EDGE ( 'NONE', *, *, #29481, .T. ) ;
#30980 = CARTESIAN_POINT ( 'NONE',  ( 758.0580252608178853, -414.4527844766010389, -328.0187753319985404 ) ) ;
#30981 = CARTESIAN_POINT ( 'NONE',  ( 802.7791456095903868, -316.7146871989593819, 329.0155153010375102 ) ) ;
#30982 = LINE ( 'NONE', #45079, #30753 ) ;
#30983 = CARTESIAN_POINT ( 'NONE',  ( 999.9999999999992042, 248.9999999999998863, -200.9999999999999432 ) ) ;
#30984 = CARTESIAN_POINT ( 'NONE',  ( 755.1538015810308480, -134.1908817542439181, 343.0433043558613804 ) ) ;
#30985 = CARTESIAN_POINT ( 'NONE',  ( 800.2193346964447755, 5.001760977943074948, 355.1360043628815788 ) ) ;
#30986 = ORIENTED_EDGE ( 'NONE', *, *, #9750, .F. ) ;
#30987 = CARTESIAN_POINT ( 'NONE',  ( 768.9521613784389729, -345.8272453906069472, -373.2346286133773106 ) ) ;
#30988 = CARTESIAN_POINT ( 'NONE',  ( 799.9636004259356241, -238.9181544815163534, 311.2241431872006956 ) ) ;
#30989 = CARTESIAN_POINT ( 'NONE',  ( 794.9819416627830151, -324.9982390220559409, -319.9864689768909898 ) ) ;
#30990 = CARTESIAN_POINT ( 'NONE',  ( 799.9999999999993179, -462.9681489794448339, 309.9999999999998863 ) ) ;
#30991 = CARTESIAN_POINT ( 'NONE',  ( 760.7433823573367135, -180.0090635724255890, -355.9930595647440441 ) ) ;
#30992 = CARTESIAN_POINT ( 'NONE',  ( 792.3570229623688874, -45.18005720387493085, 373.1304606946836202 ) ) ;
#30993 = CARTESIAN_POINT ( 'NONE',  ( 806.2451613922657998, -452.9681489794450613, 344.7413990863497020 ) ) ;
#30994 = CARTESIAN_POINT ( 'NONE',  ( 748.9653473494365699, -386.6346026584192828, -356.9462024416520762 ) ) ;
#30995 = CARTESIAN_POINT ( 'NONE',  ( -180.7583438952258348, 394.6698570112193920, -244.9999999999999716 ) ) ;
#30996 = CARTESIAN_POINT ( 'NONE',  ( 804.1009440267234822, -311.4636090269706870, 314.0944755984392600 ) ) ;
#30997 = PRODUCT_RELATED_PRODUCT_CATEGORY ( 'part', '', ( #28487 ) ) ;
#30998 = CARTESIAN_POINT ( 'NONE',  ( 779.9999999999992042, 126.4563064324884465, 339.9999999999999432 ) ) ;
#30999 = CARTESIAN_POINT ( 'NONE',  ( 763.2262854647970016, -296.6346026584195670, 309.2812353651462445 ) ) ;
#31000 = CARTESIAN_POINT ( 'NONE',  ( 811.0346526505616112, -14.63460265842049424, -323.0537975583477532 ) ) ;
#31001 = CARTESIAN_POINT ( 'NONE',  ( 797.8594530101008786, -253.5436935675104735, -322.1405469898980982 ) ) ;
#31002 = FACE_BOUND ( 'NONE', #15580, .T. ) ;
#31003 = CARTESIAN_POINT ( 'NONE',  ( 785.3687786644884454, -395.3618753856918602, 315.3201227861279676 ) ) ;
#31004 = CARTESIAN_POINT ( 'NONE',  ( 755.8894580844503253, -159.8272453906075157, 332.3691319403863531 ) ) ;
#31005 = CARTESIAN_POINT ( 'NONE',  ( 754.3581564841646241, -17.46360902697157513, -316.1443688327762516 ) ) ;
#31006 = CARTESIAN_POINT ( 'NONE',  ( 793.2243759319678702, -50.53286901714203339, -318.4439275373583200 ) ) ;
#31007 = CARTESIAN_POINT ( 'NONE',  ( 815.1787889125755555, -54.89650538077837183, 343.7953271457877804 ) ) ;
#31008 = CARTESIAN_POINT ( 'NONE',  ( 771.2633955100217236, -359.9073299311467053, 363.4237431249939618 ) ) ;
#31009 = CARTESIAN_POINT ( 'NONE',  ( 779.9999999999992042, -462.9681489794448339, 339.9999999999999432 ) ) ;
#31010 = PLANE ( 'NONE',  #18146 ) ;
#31011 = CARTESIAN_POINT ( 'NONE',  ( 754.8072714833581358, -436.8164208402372992, 338.1981804954720587 ) ) ;
#31012 = ORIENTED_EDGE ( 'NONE', *, *, #25157, .T. ) ;
#31013 = CARTESIAN_POINT ( 'NONE',  ( 759.7806653035534055, -78.99823902205662307, -324.8639956371180801 ) ) ;
#31014 = CARTESIAN_POINT ( 'NONE',  ( 754.9735926884551418, -378.3510508353227806, -340.5236548041000333 ) ) ;
#31016 = CARTESIAN_POINT ( 'NONE',  ( 788.7366044899766848, -203.9073299311471885, 316.5762568750059813 ) ) ;
#31015 = CARTESIAN_POINT ( 'NONE',  ( 785.3141322388236176, -189.7255117493290300, 364.4286716492789537 ) ) ;
#31017 = ORIENTED_EDGE ( 'NONE', *, *, #4891, .T. ) ;
#31018 = CARTESIAN_POINT ( 'NONE',  ( 746.0683387631852383, -379.4419599262318457, -331.3260364891676204 ) ) ;
#31019 = DIRECTION ( 'NONE',  ( -1.000000000000000000, -0.000000000000000000, 0.000000000000000000 ) ) ;
#31020 = VERTEX_POINT ( 'NONE', #18368 ) ;
#31021 = CARTESIAN_POINT ( 'NONE',  ( 804.4286716492782716, -401.3618753856920307, 345.3141322388244703 ) ) ;
#31022 = VERTEX_POINT ( 'NONE', #22040 ) ;
#31023 = CARTESIAN_POINT ( 'NONE',  ( 815.2698199232961542, -232.8164208402379245, -342.5225473063383106 ) ) ;
#31024 = CARTESIAN_POINT ( 'NONE',  ( 787.5162901302840055, -131.3618753856928549, 305.4481719005793252 ) ) ;
#31025 = ORIENTED_EDGE ( 'NONE', *, *, #34881, .F. ) ;
#31026 = CARTESIAN_POINT ( 'NONE',  ( 755.0636971347428243, -196.2709662947835909, -341.7834795799807353 ) ) ;
#31027 = ORIENTED_EDGE ( 'NONE', *, *, #37723, .F. ) ;
#31028 = CARTESIAN_POINT ( 'NONE',  ( 804.9363028652555840, 7.729033705215793582, -338.2165204200192079 ) ) ;
#31029 = CARTESIAN_POINT ( 'NONE',  ( 799.4546378042377910, -201.0783235625961254, 356.1575198192848006 ) ) ;
#31030 = CARTESIAN_POINT ( 'NONE',  ( 919.9999999999993179, 219.9999999999998863, -360.0000000000000000 ) ) ;
#31031 = CARTESIAN_POINT ( 'NONE',  ( 779.9999999999992042, -452.9681489794448339, 370.0000000000000568 ) ) ;
#31032 = EDGE_LOOP ( 'NONE', ( #44214, #37835, #43650, #21423, #10168, #39580 ) ) ;
#31033 = CARTESIAN_POINT ( 'NONE',  ( 796.1575198192839480, -462.0090635724247932, -359.4546378042384163 ) ) ;
#31034 = DIRECTION ( 'NONE',  ( 0.000000000000000000, 0.000000000000000000, 1.000000000000000000 ) ) ;
#31035 = FACE_OUTER_BOUND ( 'NONE', #39961, .T. ) ;
#31036 = CARTESIAN_POINT ( 'NONE',  ( 814.2805881961230625, -241.6454272087890729, -331.2368401574024119 ) ) ;
#31037 = CARTESIAN_POINT ( 'NONE',  ( 783.7953271457878373, -128.1908817542439465, 375.1787889125761239 ) ) ;
#31039 = CARTESIAN_POINT ( 'NONE',  ( 802.1676090361156639, -206.6346026584198512, -327.8955696845344505 ) ) ;
#31038 = LINE ( 'NONE', #34511, #34938 ) ;
#31040 = CARTESIAN_POINT ( 'NONE',  ( 804.9511171171677688, -413.8055962898681059, -335.8780910478229202 ) ) ;
#31041 = CARTESIAN_POINT ( 'NONE',  ( 793.5525998758768083, -247.0999726633344835, -372.6845335610516941 ) ) ;
#31042 = CARTESIAN_POINT ( 'NONE',  ( 181.1634899080285948, 260.0000000000000000, -206.1189999999954239 ) ) ;
#31043 = DIRECTION ( 'NONE',  ( 1.000000000000000000, 0.000000000000000000, 0.000000000000000000 ) ) ;
#31044 = CARTESIAN_POINT ( 'NONE',  ( 793.9708237608222134, -70.91815448151683654, -319.2295555964448681 ) ) ;
#31045 = CARTESIAN_POINT ( 'NONE',  ( 755.3028492785439312, -423.2817908451521589, 335.9200461376539693 ) ) ;
#31046 = CARTESIAN_POINT ( 'NONE',  ( 989.9999999999992042, 56.73212367640085318, -362.5753187112032379 ) ) ;
#31047 = CARTESIAN_POINT ( 'NONE',  ( 793.2243759319678702, -434.5328690171407970, -318.4439275373583200 ) ) ;
#31048 = CARTESIAN_POINT ( 'NONE',  ( 745.4481719005789273, -291.7255117493286320, -347.5162901302853697 ) ) ;
#31049 = DIRECTION ( 'NONE',  ( -0.000000000000000000, 1.000000000000000000, -0.000000000000000000 ) ) ;
#31050 = CARTESIAN_POINT ( 'NONE',  ( 792.1044303154645831, 11.54721552339760038, 317.8323909638837677 ) ) ;
#31051 = CARTESIAN_POINT ( 'NONE',  ( 788.8264449731200330, -69.18005720387488111, -363.6646147819171233 ) ) ;
#31052 = CARTESIAN_POINT ( 'NONE',  ( 749.5768839229115201, -228.5545181178799794, 358.0661480581553064 ) ) ;
#31053 = CARTESIAN_POINT ( 'NONE',  ( 801.9858362298568863, -171.0783235625962106, -312.7379699480935642 ) ) ;
#31054 = CARTESIAN_POINT ( 'NONE',  ( 796.9462024416508257, -204.4527844766016926, 308.9653473494370246 ) ) ;
#31055 = CARTESIAN_POINT ( 'NONE',  ( 745.4481719005789273, -411.7255117493282910, -347.5162901302853129 ) ) ;
#31056 = DIRECTION ( 'NONE',  ( 0.000000000000000000, -0.000000000000000000, -1.000000000000000000 ) ) ;
#31057 = CARTESIAN_POINT ( 'NONE',  ( 804.6798772138708955, -303.7255117493287457, 334.6312213355107019 ) ) ;
#31058 = ADVANCED_FACE ( 'NONE', ( #29208 ), #39845, .F. ) ;
#31059 = CARTESIAN_POINT ( 'NONE',  ( 760.7433823573367135, -60.00906357242598688, 355.9930595647440441 ) ) ;
#31060 = CARTESIAN_POINT ( 'NONE',  ( 788.8264449731200330, -429.1800572038737869, -363.6646147819171233 ) ) ;
#31061 = CARTESIAN_POINT ( 'NONE',  ( 829.9999999999992042, 290.0000000000001137, -244.9999999999999716 ) ) ;
#31062 = DIRECTION ( 'NONE',  ( 0.000000000000000000, 0.000000000000000000, 1.000000000000000000 ) ) ;
#31064 = CARTESIAN_POINT ( 'NONE',  ( 758.0580252608178853, -342.4527844766013231, 328.0187753319985404 ) ) ;
#31063 = CARTESIAN_POINT ( 'NONE',  ( 779.4709603349208464, -120.3510508353236048, 314.7162404726379918 ) ) ;
#31065 = ORIENTED_EDGE ( 'NONE', *, *, #43267, .F. ) ;
#31066 = CARTESIAN_POINT ( 'NONE',  ( 802.7791456095903868, -244.7146871989596093, -329.0155153010375102 ) ) ;
#31067 = CARTESIAN_POINT ( 'NONE',  ( 755.5713283507202505, -101.3618753856929544, 334.6858677611754729 ) ) ;
#31068 = CARTESIAN_POINT ( 'NONE',  ( 812.6845335610512393, -271.9874144716868045, -353.5525998758768651 ) ) ;
#31069 = CARTESIAN_POINT ( 'NONE',  ( -338.8365100919713200, 260.0000000000001137, -199.9999999999917861 ) ) ;
#31070 = CARTESIAN_POINT ( 'NONE',  ( 795.6651683502461765, -370.7146871989592114, 371.3240766477733814 ) ) ;
#31071 = VERTEX_POINT ( 'NONE', #10737 ) ;
#31072 = CARTESIAN_POINT ( 'NONE',  ( 759.9864689768902508, -290.0891481129650629, 354.9819416627836404 ) ) ;
#31073 = CARTESIAN_POINT ( 'NONE',  ( 796.7845633553578182, -33.62377810805116951, -358.5707757039688204 ) ) ;
#31074 = CARTESIAN_POINT ( 'NONE',  ( 755.0636971347428243, -172.2709662947836478, -341.7834795799807353 ) ) ;
#31075 = CARTESIAN_POINT ( 'NONE',  ( 785.3687786644884454, -395.3618753856918602, 315.3201227861279676 ) ) ;
#31076 = CARTESIAN_POINT ( 'NONE',  ( 796.7737145352015204, -116.6346026584201780, -370.7187646348536987 ) ) ;
#31077 = EDGE_CURVE ( 'NONE', #20728, #34100, #10711, .T. ) ;
#31078 = CARTESIAN_POINT ( 'NONE',  ( 756.5762568750052424, -99.18005720387478164, -348.7366044899774238 ) ) ;
#31079 = ORIENTED_EDGE ( 'NONE', *, *, #34008, .F. ) ;
#31080 = CARTESIAN_POINT ( 'NONE',  ( 763.0428371773158460, -59.46360902697142592, -358.7617431975195359 ) ) ;
#31081 = CARTESIAN_POINT ( 'NONE',  ( 793.0897708529556667, -342.5545181178796952, -361.3366627262616362 ) ) ;
#31083 = CARTESIAN_POINT ( 'NONE',  ( 787.5531968255692163, -453.8272453906066630, 316.1348686366205811 ) ) ;
#31082 = CARTESIAN_POINT ( 'NONE',  ( 804.9363028652555840, -112.2709662947838325, 338.2165204200192079 ) ) ;
#31084 = CARTESIAN_POINT ( 'NONE',  ( 769.1273215169530886, -94.71468719896007826, 317.4527132478988847 ) ) ;
#31087 = CARTESIAN_POINT ( 'NONE',  ( 791.1614460488616487, -371.2601417444136587, 373.5763878283158874 ) ) ;
#31086 = CARTESIAN_POINT ( 'NONE',  ( 829.9999999999992042, -600.0000000000000000, -320.0000000000000568 ) ) ;
#31085 = CARTESIAN_POINT ( 'NONE',  ( 799.9999999999993179, -512.9681489794448908, 350.0000000000000000 ) ) ;
#31088 = CARTESIAN_POINT ( 'NONE',  ( 786.5483106153019435, -343.6454272087887603, -364.1601925771022366 ) ) ;
#31089 = CARTESIAN_POINT ( 'NONE',  ( 771.2633955100217236, -359.9073299311467053, -363.4237431249939618 ) ) ;
#31090 = CARTESIAN_POINT ( 'NONE',  ( 795.8262568251477660, -142.3726999360620766, -308.3538107759623585 ) ) ;
#31091 = CARTESIAN_POINT ( 'NONE',  ( 812.3518521366052028, -1.099972663335260226, 326.5853460496235243 ) ) ;
#31093 = PLANE ( 'NONE',  #24001 ) ;
#31092 = CARTESIAN_POINT ( 'NONE',  ( 919.9999999999993179, 154.9999999999998863, 360.0000000000000000 ) ) ;
#31094 = CARTESIAN_POINT ( 'NONE',  ( 758.6633372737375112, -284.5328690171412518, -326.9102291470432533 ) ) ;
#31095 = CARTESIAN_POINT ( 'NONE',  ( 766.4474001241216001, -163.0999726633347677, -307.3154664389482491 ) ) ;
#31096 = DIRECTION ( 'NONE',  ( -0.000000000000000000, 1.000000000000000000, -0.000000000000000000 ) ) ;
#31097 = DIRECTION ( 'NONE',  ( -0.7071067811857625340, -8.659560562345319848E-17, -0.7071067811873326114 ) ) ;
#31098 = CARTESIAN_POINT ( 'NONE',  ( 799.2566176426618085, -336.0090635724251911, 324.0069404352559559 ) ) ;
#31099 = CARTESIAN_POINT ( 'NONE',  ( 783.7953271457878373, -296.1908817542434917, 375.1787889125761239 ) ) ;
#31100 = CARTESIAN_POINT ( 'NONE',  ( 801.1904061080338124, -188.0891481129653755, -368.3070685750236066 ) ) ;
#31101 = LINE ( 'NONE', #14245, #13536 ) ;
#31102 = CARTESIAN_POINT ( 'NONE',  ( 754.3581564841646241, -113.4636090269712554, 316.1443688327762516 ) ) ;
#31103 = CARTESIAN_POINT ( 'NONE',  ( 758.8095938919642549, -320.0891481129648355, -311.6929314249763365 ) ) ;
#31104 = EDGE_CURVE ( 'NONE', #8149, #31071, #42426, .T. ) ;
#31105 = DIRECTION ( 'NONE',  ( 1.892425610156518354E-16, 1.000000000000000000, -0.000000000000000000 ) ) ;
#31106 = FACE_OUTER_BOUND ( 'NONE', #14096, .T. ) ;
#31107 = CARTESIAN_POINT ( 'NONE',  ( 754.8072714833581358, -196.8164208402380950, 338.1981804954720587 ) ) ;
#31108 = MECHANICAL_DESIGN_GEOMETRIC_PRESENTATION_REPRESENTATION (  '', ( #19308 ), #32608 ) ;
#31109 = ORIENTED_EDGE ( 'NONE', *, *, #22429, .F. ) ;
#31110 = ADVANCED_FACE ( 'NONE', ( #18586 ), #4494, .F. ) ;
#31111 = CARTESIAN_POINT ( 'NONE',  ( 793.5525998758768083, -439.0999726633339719, 372.6845335610516941 ) ) ;
#31112 = CARTESIAN_POINT ( 'NONE',  ( 773.7943932421234194, -359.8055962898683333, -305.5313806188329409 ) ) ;
#31113 = CARTESIAN_POINT ( 'NONE',  ( 745.4481719005789273, -123.7255117493292147, -347.5162901302853129 ) ) ;
#31114 = CARTESIAN_POINT ( 'NONE',  ( 755.5913626894240451, -61.64542720878961291, 346.6156483768012890 ) ) ;
#31115 = CARTESIAN_POINT ( 'NONE',  ( 810.7187646348534145, -402.4527844766010389, -356.7737145352016341 ) ) ;
#31116 = DIRECTION ( 'NONE',  ( -1.000000000000000000, -0.000000000000000000, -0.000000000000000000 ) ) ;
#31117 = CARTESIAN_POINT ( 'NONE',  ( 802.7791456095903868, -436.7146871989589272, 329.0155153010375102 ) ) ;
#31118 = ORIENTED_EDGE ( 'NONE', *, *, #14855, .F. ) ;
#31119 = CARTESIAN_POINT ( 'NONE',  ( 756.5762568750052424, -267.1800572038742985, 348.7366044899774238 ) ) ;
#31120 = CARTESIAN_POINT ( 'NONE',  ( 747.3154664389472828, -163.9874144716871456, -326.4474001241230781 ) ) ;
#31121 = DIRECTION ( 'NONE',  ( 1.000000000000000000, 0.000000000000000000, -0.000000000000000000 ) ) ;
#31122 = CARTESIAN_POINT ( 'NONE',  ( 793.4146539503750546, -265.9874144716867477, 307.6481478633938877 ) ) ;
#31123 = CARTESIAN_POINT ( 'NONE',  ( 785.3141322388236176, -117.7255117493292715, 364.4286716492789537 ) ) ;
#31124 = ORIENTED_EDGE ( 'NONE', *, *, #9214, .T. ) ;
#31125 = CARTESIAN_POINT ( 'NONE',  ( 759.9864689768902508, -266.0891481129651197, 354.9819416627836404 ) ) ;
#31126 = CARTESIAN_POINT ( 'NONE',  ( 813.1304606946830518, 6.092670068852159559, -352.3570229623690580 ) ) ;
#31127 = CARTESIAN_POINT ( 'NONE',  ( 789.6004645510835189, -449.9487230857661757, 364.2073161732290600 ) ) ;
#31129 = EDGE_LOOP ( 'NONE', ( #20576, #13357, #35493, #45286 ) ) ;
#31128 = CARTESIAN_POINT ( 'NONE',  ( 779.4709603349208464, -96.35105083532370429, -314.7162404726379918 ) ) ;
#31130 = CARTESIAN_POINT ( 'NONE',  ( 804.4286716492782716, -185.3618753856926844, -345.3141322388244703 ) ) ;
#31131 = CARTESIAN_POINT ( 'NONE',  ( 793.5525998758768083, -415.0999726633340288, -372.6845335610516941 ) ) ;
#31132 = CARTESIAN_POINT ( 'NONE',  ( 788.8264449731200330, -21.18005720387502677, 363.6646147819171233 ) ) ;
#31133 = CARTESIAN_POINT ( 'NONE',  ( 788.7366044899766848, -251.9073299311470748, -316.5762568750059813 ) ) ;
#31135 = CARTESIAN_POINT ( 'NONE',  ( 781.2497674668890113, -252.3510508353232353, 375.3608509340180603 ) ) ;
#31134 = CARTESIAN_POINT ( 'NONE',  ( 805.0032342141413437, -373.5436935675102177, 314.9967657858572352 ) ) ;
#31136 = CARTESIAN_POINT ( 'NONE',  ( 796.9571628226829034, -239.4636090269709143, -321.2382568024804641 ) ) ;
#31137 = CARTESIAN_POINT ( 'NONE',  ( 755.3201227861273992, -243.7255117493287742, -345.3687786644892981 ) ) ;
#31138 = VECTOR ( 'NONE', #10777, 1000.000000000000000 ) ;
#31139 = CARTESIAN_POINT ( 'NONE',  ( 755.0636971347428243, -436.2709662947827951, -341.7834795799807353 ) ) ;
#31140 = CARTESIAN_POINT ( 'NONE',  ( 764.8639956371174549, -80.08914811296574499, -319.7806653035542013 ) ) ;
#31141 = CARTESIAN_POINT ( 'NONE',  ( 774.6312213355099630, -239.3618753856924570, 364.6798772138717482 ) ) ;
#31142 = ORIENTED_EDGE ( 'NONE', *, *, #9484, .T. ) ;
#31143 = CARTESIAN_POINT ( 'NONE',  ( 746.8695393053150156, -365.9073299311465917, 327.6429770376306010 ) ) ;
#31144 = DIRECTION ( 'NONE',  ( 1.000000000000000000, -1.880165489482579047E-16, 0.000000000000000000 ) ) ;
#31145 = CARTESIAN_POINT ( 'NONE',  ( 745.5313806188320314, -39.28179084515331709, -333.7943932421247268 ) ) ;
#31146 = DIRECTION ( 'NONE',  ( 0.000000000000000000, 1.000000000000000000, 0.000000000000000000 ) ) ;
#31147 = DIRECTION ( 'NONE',  ( 1.000000000000000000, 0.000000000000000000, 0.000000000000000000 ) ) ;
#31148 = EDGE_CURVE ( 'NONE', #6808, #22371, #38021, .T. ) ;
#31149 = CARTESIAN_POINT ( 'NONE',  ( 754.7162404726377645, -230.7363362996981664, 339.4709603349214717 ) ) ;
#31150 = CARTESIAN_POINT ( 'NONE',  ( 758.0580252608178853, -102.4527844766020337, 328.0187753319985404 ) ) ;
#31151 = ORIENTED_EDGE ( 'NONE', *, *, #24693, .T. ) ;
#31152 = CARTESIAN_POINT ( 'NONE',  ( 761.4292242960306112, -17.46360902697157513, -323.2154366446414429 ) ) ;
#31153 = CARTESIAN_POINT ( 'NONE',  ( 754.9967657858570647, -73.54369356751121245, -365.0032342141425943 ) ) ;
#31154 = CARTESIAN_POINT ( 'NONE',  ( 755.8398074228967971, -283.4419599262321867, 333.4516893846970333 ) ) ;
#31155 = CARTESIAN_POINT ( 'NONE',  ( 800.0135310231082713, -446.0891481129646081, -325.0180583372163028 ) ) ;
#31156 = CARTESIAN_POINT ( 'NONE',  ( 755.0636971347428243, -28.27096629478409540, -341.7834795799807353 ) ) ;
#31157 = CARTESIAN_POINT ( 'NONE',  ( 773.7305795820266212, -9.281790845153418346, 374.8230680027170365 ) ) ;
#31158 = ADVANCED_FACE ( 'NONE', ( #10975 ), #7973, .F. ) ;
#31159 = CARTESIAN_POINT ( 'NONE',  ( 808.3070685750230950, -186.9982390220563104, -361.1904061080339261 ) ) ;
#31160 = EDGE_CURVE ( 'NONE', #8154, #41883, #24815, .T. ) ;
#31161 = CARTESIAN_POINT ( 'NONE',  ( 745.7998596910086917, -173.3618753856927128, 332.5602148656461168 ) ) ;
#31162 = CARTESIAN_POINT ( 'NONE',  ( 771.1735550268778070, -81.18005720387481006, 316.3353852180827630 ) ) ;
#31163 = VECTOR ( 'NONE', #41049, 1000.000000000000000 ) ;
#31164 = DIRECTION ( 'NONE',  ( 1.000000000000000000, 0.000000000000000000, -0.000000000000000000 ) ) ;
#31165 = DIRECTION ( 'NONE',  ( -0.3826814224632300032, 0.000000000000000000, -0.9238803650373347276 ) ) ;
#31166 = CARTESIAN_POINT ( 'NONE',  ( 768.8385539511368734, -263.2601417444141134, -306.4236121716840557 ) ) ;
#31167 = CARTESIAN_POINT ( 'NONE',  ( 807.2620300519052989, -432.0090635724247932, 318.0141637701419768 ) ) ;
#31168 = CARTESIAN_POINT ( 'NONE',  ( 746.8695393053150156, -269.9073299311468190, -327.6429770376306010 ) ) ;
#31169 = CARTESIAN_POINT ( 'NONE',  ( 799.9999999999993179, -512.9681489794448908, -309.9999999999998863 ) ) ;
#31170 = CARTESIAN_POINT ( 'NONE',  ( 749.2812353651451076, -414.4527844766010389, 323.2262854647983090 ) ) ;
#31171 = CARTESIAN_POINT ( 'NONE',  ( 759.0252816721024374, -0.9982390220569063999, 368.0189434323527280 ) ) ;
#31172 = CARTESIAN_POINT ( 'NONE',  ( 813.9316612368132837, -31.44195992623299674, -348.6739635108323228 ) ) ;
#31173 = CARTESIAN_POINT ( 'NONE',  ( 803.6646147819161570, -377.9073299311466485, -348.8264449731210561 ) ) ;
#31174 = CARTESIAN_POINT ( 'NONE',  ( 799.4546378042377910, -9.078323562596708030, 356.1575198192848006 ) ) ;
#31175 = COLOUR_RGB ( '',0.7921568627450980005, 0.8196078431372548767, 0.9333333333333333481 ) ;
#31176 = CARTESIAN_POINT ( 'NONE',  ( 795.6651683502461765, -58.71468719896019905, -371.3240766477733814 ) ) ;
#31177 = CARTESIAN_POINT ( 'NONE',  ( 787.6308680596127942, -155.2601417444144261, -364.1105419155492768 ) ) ;
#31178 = EDGE_CURVE ( 'NONE', #27330, #5332, #29889, .T. ) ;
#31179 = CARTESIAN_POINT ( 'NONE',  ( 745.1769319972822814, -185.8055962898689302, 346.2694204179732083 ) ) ;
#31180 = CARTESIAN_POINT ( 'NONE',  ( 803.6646147819162707, -17.90732993114776406, 348.8264449731211130 ) ) ;
#31181 = EDGE_CURVE ( 'NONE', #41469, #20456, #1015, .T. ) ;
#31182 = EDGE_LOOP ( 'NONE', ( #20109, #28705, #43363, #12500 ) ) ;
#31183 = CARTESIAN_POINT ( 'NONE',  ( 755.0636971347428243, -52.27096629478401724, -341.7834795799807353 ) ) ;
#31184 = CARTESIAN_POINT ( 'NONE',  ( 773.3843516231979720, -181.4419599262325278, -364.4086373105754433 ) ) ;
#31185 = PRODUCT_DEFINITION_CONTEXT ( 'detailed design', #18153, 'design' ) ;
#31186 = CARTESIAN_POINT ( 'NONE',  ( 781.7834795799800531, -178.8164208402381519, 315.0636971347436202 ) ) ;
#31187 = CARTESIAN_POINT ( 'NONE',  ( 748.3538107759620743, 7.285312801039605546, -355.8262568251490165 ) ) ;
#31188 = CARTESIAN_POINT ( 'NONE',  ( 768.0187753319979720, -296.6346026584195670, 318.0580252608186242 ) ) ;
#31189 = CARTESIAN_POINT ( 'NONE',  ( 919.9999999999993179, 154.9999999999998863, 360.0000000000000000 ) ) ;
#31190 = ORIENTED_EDGE ( 'NONE', *, *, #40721, .T. ) ;
#31191 = CARTESIAN_POINT ( 'NONE',  ( 804.9511171171677688, -29.80559628986937781, 335.8780910478229202 ) ) ;
#31192 = CARTESIAN_POINT ( 'NONE',  ( 813.5763878283155464, -291.8272453906071746, -351.1614460488615350 ) ) ;
#31193 = CARTESIAN_POINT ( 'NONE',  ( 744.7301800767020268, -244.8164208402379245, 337.4774526936615189 ) ) ;
#31194 = CARTESIAN_POINT ( 'NONE',  ( 801.5560724626406000, -336.5545181178796952, 326.7756240680316182 ) ) ;
#31195 = CARTESIAN_POINT ( 'NONE',  ( 759.8311093483677041, 25.83076734649409545, 310.9282345327691814 ) ) ;
#31196 = CARTESIAN_POINT ( 'NONE',  ( 786.5483106153019435, -151.6454272087892718, -364.1601925771022366 ) ) ;
#31197 = CARTESIAN_POINT ( 'NONE',  ( 803.6646147819161570, -161.9073299311472454, -348.8264449731210561 ) ) ;
#31198 = CIRCLE ( 'NONE', #9802, 6.118999999999985562 ) ;
#31199 = CARTESIAN_POINT ( 'NONE',  ( 804.6798772138710092, -303.7255117493286889, -334.6312213355106451 ) ) ;
#31200 = ORIENTED_EDGE ( 'NONE', *, *, #29809, .T. ) ;
#31201 = PRODUCT_DEFINITION_FORMATION_WITH_SPECIFIED_SOURCE ( 'ANY', '', #21103, .NOT_KNOWN. ) ;
#31202 = EDGE_CURVE ( 'NONE', #24474, #37455, #15179, .T. ) ;
#31203 = CARTESIAN_POINT ( 'NONE',  ( 761.2382568024794409, -327.6237781080502600, 356.9571628226838129 ) ) ;
#31204 = CARTESIAN_POINT ( 'NONE',  ( -39.63011601220123481, -494.6608068873671300, -357.6536686473015720 ) ) ;
#31205 = EDGE_CURVE ( 'NONE', #8202, #3566, #3806, .T. ) ;
#31206 = CARTESIAN_POINT ( 'NONE',  ( 769.9779781133707957, -139.0999726633348530, 316.7813123517150871 ) ) ;
#31207 = CARTESIAN_POINT ( 'NONE',  ( 755.5713283507202505, -5.361875385693257279, 334.6858677611754729 ) ) ;
#31208 = ORIENTED_EDGE ( 'NONE', *, *, #24136, .F. ) ;
#31209 = CARTESIAN_POINT ( 'NONE',  ( 754.3581564841646241, -377.4636090269704596, -316.1443688327762516 ) ) ;
#31210 = DIRECTION ( 'NONE',  ( -0.000000000000000000, -1.110223024625155554E-15, 1.000000000000000000 ) ) ;
#31211 = CARTESIAN_POINT ( 'NONE',  ( 760.0363995740630116, -226.9181544815163534, 368.7758568127991907 ) ) ;
#31212 = CARTESIAN_POINT ( 'NONE',  ( 769.1273215169530886, -190.7146871989597798, 317.4527132478988847 ) ) ;
#31213 = CARTESIAN_POINT ( 'NONE',  ( 762.3223304703356007, -343.5436935675103314, -322.3223304703362828 ) ) ;
#31214 = LINE ( 'NONE', #30990, #25927 ) ;
#31215 = CARTESIAN_POINT ( 'NONE',  ( 763.0428371773158460, -227.4636090269709143, -358.7617431975195359 ) ) ;
#31216 = EDGE_CURVE ( 'NONE', #26139, #34942, #34344, .T. ) ;
#31217 = CARTESIAN_POINT ( 'NONE',  ( 746.8695393053150156, -77.90732993114757221, 327.6429770376306010 ) ) ;
#31218 = DIRECTION ( 'NONE',  ( -1.000000000000000000, 0.000000000000000000, 0.000000000000000000 ) ) ;
#31219 = CARTESIAN_POINT ( 'NONE',  ( 772.5602148656447525, -417.7255117493283478, -305.7998596910095443 ) ) ;
#31220 = PLANE ( 'NONE',  #15797 ) ;
#31221 = CARTESIAN_POINT ( 'NONE',  ( 750.9282345327678740, -352.9181544815159555, 319.8311093483690115 ) ) ;
#31222 = CARTESIAN_POINT ( 'NONE',  ( 792.0613484971601110, -458.0032201311295807, -367.4685979341032294 ) ) ;
#31223 = CARTESIAN_POINT ( 'NONE',  ( 772.4837098697144029, -287.3618753856923718, 374.5518280994205611 ) ) ;
#31224 = CARTESIAN_POINT ( 'NONE',  ( 751.9810565676468741, -50.08914811296584446, -360.9747183278973921 ) ) ;
#31225 = CARTESIAN_POINT ( 'NONE',  ( 791.9812246680005501, -236.6346026584198228, -361.9419747391813189 ) ) ;
#31226 = FACE_BOUND ( 'NONE', #28761, .T. ) ;
#31227 = CARTESIAN_POINT ( 'NONE',  ( 765.0180583372156207, -408.9982390220556567, 360.0135310231089534 ) ) ;
#31228 = AXIS2_PLACEMENT_3D ( 'NONE', #19804, #5474, #9413 ) ;
#31229 = CARTESIAN_POINT ( 'NONE',  ( 755.5913626894240451, -157.6454272087893287, 346.6156483768012890 ) ) ;
#31230 = CARTESIAN_POINT ( 'NONE',  ( 745.5313806188320314, -15.28179084515340058, -333.7943932421247268 ) ) ;
#31231 = CARTESIAN_POINT ( 'NONE',  ( 784.0799538623451781, -59.80559628986927834, -364.6971507214555572 ) ) ;
#31232 = CARTESIAN_POINT ( 'NONE',  ( 813.2346286133761168, -53.26014174441475291, 328.9521613784389160 ) ) ;
#31233 = CARTESIAN_POINT ( 'NONE',  ( 778.2165204200184689, -382.8164208402374697, 364.9363028652563230 ) ) ;
#31234 = AXIS2_PLACEMENT_3D ( 'NONE', #35568, #32359, #5520 ) ;
#31235 = CARTESIAN_POINT ( 'NONE',  ( 777.4774526936600978, 13.72903370521577315, 304.7301800767028226 ) ) ;
#31236 = DIRECTION ( 'NONE',  ( -1.000000000000000000, 0.000000000000000000, -0.000000000000000000 ) ) ;
#31237 = CARTESIAN_POINT ( 'NONE',  ( 778.2165204200184689, -430.8164208402374129, 364.9363028652563230 ) ) ;
#31238 = ORIENTED_EDGE ( 'NONE', *, *, #30653, .F. ) ;
#31239 = CARTESIAN_POINT ( 'NONE',  ( 771.2633955100217236, -71.90732993114760063, -363.4237431249939618 ) ) ;
#31240 = CARTESIAN_POINT ( 'NONE',  ( 760.5453621957607311, -357.0783235625956422, -323.8424801807151425 ) ) ;
#31242 = CARTESIAN_POINT ( 'NONE',  ( 758.0580252608178853, -198.4527844766017495, 328.0187753319985404 ) ) ;
#31241 = CARTESIAN_POINT ( 'NONE',  ( 788.8264449731200330, -189.1800572038744122, 363.6646147819171233 ) ) ;
#31243 = ORIENTED_EDGE ( 'NONE', *, *, #6551, .T. ) ;
#31244 = CARTESIAN_POINT ( 'NONE',  ( 754.0944755984390895, -375.6237781080501463, -364.1009440267246760 ) ) ;
#31245 = DIRECTION ( 'NONE',  ( 0.000000000000000000, 0.9238795325112891810, -0.3826834323650838421 ) ) ;
#31246 = VERTEX_POINT ( 'NONE', #42615 ) ;
#31247 = CARTESIAN_POINT ( 'NONE',  ( 797.6776695296629214, -379.5436935675102745, 357.6776695296636603 ) ) ;
#31248 = CIRCLE ( 'NONE', #23382, 9.999999999999982236 ) ;
#31249 = ORIENTED_EDGE ( 'NONE', *, *, #25229, .T. ) ;
#31250 = CARTESIAN_POINT ( 'NONE',  ( 755.2512626584698410, -223.5436935675107577, -315.2512626584710915 ) ) ;
#31251 = ORIENTED_EDGE ( 'NONE', *, *, #32638, .T. ) ;
#31252 = CARTESIAN_POINT ( 'NONE',  ( 798.0661480581538854, -194.5328690171415644, 309.5768839229118043 ) ) ;
#31253 = CARTESIAN_POINT ( 'NONE',  ( 788.8264449731201466, -213.1800572038743837, -363.6646147819170665 ) ) ;
#31254 = ORIENTED_EDGE ( 'NONE', *, *, #22184, .T. ) ;
#31255 = CARTESIAN_POINT ( 'NONE',  ( 778.1981804954714335, -346.2709662947830793, -314.8072714833589885 ) ) ;
#31256 = CARTESIAN_POINT ( 'NONE',  ( 785.3687786644884454, -11.36187538569323863, -315.3201227861279676 ) ) ;
#31257 = EDGE_CURVE ( 'NONE', #19781, #26699, #7506, .T. ) ;
#31258 = CARTESIAN_POINT ( 'NONE',  ( 783.0433043558608688, -216.8965053807778816, 315.1538015810313027 ) ) ;
#31259 = DIRECTION ( 'NONE',  ( 1.000000000000000000, 0.000000000000000000, 0.000000000000000000 ) ) ;
#31260 = LINE ( 'NONE', #6324, #22825 ) ;
#31261 = VERTEX_POINT ( 'NONE', #18134 ) ;
#31262 = CARTESIAN_POINT ( 'NONE',  ( 804.1105419155481968, -459.8272453906066062, -347.6308680596136469 ) ) ;
#31263 = DIRECTION ( 'NONE',  ( 0.000000000000000000, 0.000000000000000000, 1.000000000000000000 ) ) ;
#31264 = DIRECTION ( 'NONE',  ( -0.000000000000000000, -0.000000000000000000, -1.000000000000000000 ) ) ;
#31265 = CARTESIAN_POINT ( 'NONE',  ( 810.4231160770870019, -288.5545181178798657, -321.9338519418446936 ) ) ;
#31266 = AXIS2_PLACEMENT_3D ( 'NONE', #2650, #37529, #16512 ) ;
#31267 = CARTESIAN_POINT ( 'NONE',  ( 809.0717654672305343, -124.9181544815167086, 360.1688906516309885 ) ) ;
#31269 = CARTESIAN_POINT ( 'NONE',  ( 797.6776695296629214, -211.5436935675107861, -357.6776695296636603 ) ) ;
#31268 = CARTESIAN_POINT ( 'NONE',  ( 571.1634899080285095, 259.9999999999999432, -206.1189999999981239 ) ) ;
#31270 = CARTESIAN_POINT ( 'NONE',  ( 783.0433043558608688, -384.8965053807772847, -315.1538015810313027 ) ) ;
#31271 = FACE_OUTER_BOUND ( 'NONE', #26622, .T. ) ;
#31272 = CARTESIAN_POINT ( 'NONE',  ( 771.1735550268780344, 14.81994279612486309, -316.3353852180828198 ) ) ;
#31273 = CARTESIAN_POINT ( 'NONE',  ( 793.9708237608222134, -94.91815448151677970, -319.2295555964448681 ) ) ;
#31274 = CARTESIAN_POINT ( 'NONE',  ( 809.0717654672305343, -388.9181544815158986, 360.1688906516309885 ) ) ;
#31275 = CARTESIAN_POINT ( 'NONE',  ( 51.16348990802859475, 260.0000000000000568, -193.8809999999945148 ) ) ;
#31276 = CARTESIAN_POINT ( 'NONE',  ( 771.2368401574024119, 10.55804007376686826, -374.2805881961240857 ) ) ;
#31277 = CARTESIAN_POINT ( 'NONE',  ( 787.5162901302840055, -299.3618753856923149, -305.4481719005793252 ) ) ;
#31278 = CARTESIAN_POINT ( 'NONE',  ( -521.6730038022808458, 200.0000000000001421, -122.7905160835438068 ) ) ;
#31279 = CARTESIAN_POINT ( 'NONE',  ( 756.3353852180819104, -77.90732993114757221, -331.1735550268788302 ) ) ;
#31280 = CIRCLE ( 'NONE', #3987, 10.00000000000000888 ) ;
#31281 = CARTESIAN_POINT ( 'NONE',  ( 807.2620300519052989, -240.0090635724253900, 318.0141637701419768 ) ) ;
#31282 = CARTESIAN_POINT ( 'NONE',  ( 751.2241431872005251, -184.1692326535052757, -359.9636004259367610 ) ) ;
#31283 = CARTESIAN_POINT ( 'NONE',  ( 745.7998596910086917, -197.3618753856926560, 332.5602148656461168 ) ) ;
#31284 = CARTESIAN_POINT ( 'NONE',  ( 814.5518280994195948, -447.7255117493280636, -332.4837098697145734 ) ) ;
#31285 = DIRECTION ( 'NONE',  ( 0.000000000000000000, -1.000000000000000000, 1.110223024625155554E-15 ) ) ;
#31286 = CARTESIAN_POINT ( 'NONE',  ( 797.6776695296629214, -283.5436935675105019, 357.6776695296636603 ) ) ;
#31287 = CARTESIAN_POINT ( 'NONE',  ( 775.8780910478218402, -57.28179084515326736, 364.9511171171680530 ) ) ;
#31288 = CARTESIAN_POINT ( 'NONE',  ( 792.1044303154645831, -420.4527844766009252, -317.8323909638837677 ) ) ;
#31289 = CARTESIAN_POINT ( 'NONE',  ( -746.4999999999993179, -365.3551492539851893, -8.132432514707076621 ) ) ;
#31290 = DIRECTION ( 'NONE',  ( 0.000000000000000000, 0.000000000000000000, -1.000000000000000000 ) ) ;
#31292 = CARTESIAN_POINT ( 'NONE',  ( 800.0135310231082713, -326.0891481129649492, 325.0180583372163028 ) ) ;
#31291 = CARTESIAN_POINT ( 'NONE',  ( 789.9200121543843807, -121.9874144716872593, 317.0176451133914384 ) ) ;
#31293 = VERTEX_POINT ( 'NONE', #32212 ) ;
#31294 = CARTESIAN_POINT ( 'NONE',  ( 780.5290396650775619, -252.3510508353232353, -365.2837595273619513 ) ) ;
#31295 = CARTESIAN_POINT ( 'NONE',  ( 794.9819416627830151, -84.99823902205663728, 319.9864689768909898 ) ) ;
#31296 = CARTESIAN_POINT ( 'NONE',  ( 811.6461892240364477, -268.7146871989595525, -324.1737431748509835 ) ) ;
#31297 = CARTESIAN_POINT ( 'NONE',  ( -746.4999999999993179, -365.3551492539851893, -18.13243251470705886 ) ) ;
#31298 = CARTESIAN_POINT ( 'NONE',  ( 758.0141637701419768, -399.0783235625955285, 367.2620300519063790 ) ) ;
#31299 = EDGE_LOOP ( 'NONE', ( #4338, #23106, #31151, #2109 ) ) ;
#31300 = CARTESIAN_POINT ( 'NONE',  ( 781.7834795799800531, -298.8164208402377540, 315.0636971347436202 ) ) ;
#31301 = CARTESIAN_POINT ( 'NONE',  ( 800.7704444035546203, -52.16923265350567362, -326.0291762391768771 ) ) ;
#31302 = CARTESIAN_POINT ( 'NONE',  ( 803.6646147819161570, -161.9073299311472454, -348.8264449731210561 ) ) ;
#31303 = CARTESIAN_POINT ( 'NONE',  ( 758.0580252608178853, -198.4527844766017495, -328.0187753319985404 ) ) ;
#31304 = CARTESIAN_POINT ( 'NONE',  ( 785.3687786644884454, -419.3618753856918033, 315.3201227861279676 ) ) ;
#31305 = CARTESIAN_POINT ( 'NONE',  ( 745.0891759886404770, -100.2709662947838609, -342.4968714119734159 ) ) ;
#31306 = CARTESIAN_POINT ( 'NONE',  ( 755.0636971347428243, -124.2709662947837899, -341.7834795799807353 ) ) ;
#31307 = ORIENTED_EDGE ( 'NONE', *, *, #39390, .F. ) ;
#31308 = CARTESIAN_POINT ( 'NONE',  ( 802.5472867521000353, -28.37269993606244967, -350.8726784830461156 ) ) ;
#31309 = CARTESIAN_POINT ( 'NONE',  ( 755.1538015810308480, -398.1908817542431507, -343.0433043558613804 ) ) ;
#31310 = AXIS2_PLACEMENT_3D ( 'NONE', #12446, #1584, #36925 ) ;
#31312 = CARTESIAN_POINT ( 'NONE',  ( 796.9571628226829034, -431.4636090269702322, 321.2382568024804641 ) ) ;
#31311 = CARTESIAN_POINT ( 'NONE',  ( 756.3353852180819104, -125.9073299311474159, 331.1735550268788302 ) ) ;
#31313 = CARTESIAN_POINT ( 'NONE',  ( 794.1144889064781864, -106.1692326535054889, 360.9840315886528401 ) ) ;
#31316 = CARTESIAN_POINT ( 'NONE',  ( 813.9316612368132837, -343.4419599262320162, 348.6739635108323228 ) ) ;
#31315 = CARTESIAN_POINT ( 'NONE',  ( 799.9999999999993179, -462.9681489794448339, 309.9999999999998863 ) ) ;
#31314 = CARTESIAN_POINT ( 'NONE',  ( 939.9999999999993179, 56.78581973499407809, -212.6378164459127618 ) ) ;
#31317 = VECTOR ( 'NONE', #1967, 1000.000000000000000 ) ;
#31318 = EDGE_LOOP ( 'NONE', ( #40677, #8277, #23398, #12441 ) ) ;
#31319 = CARTESIAN_POINT ( 'NONE',  ( 805.2837595273609850, -362.7363362996977116, -340.5290396650784714 ) ) ;
#31320 = CARTESIAN_POINT ( 'NONE',  ( 803.4237431249931660, -351.1800572038740142, -331.2633955100225194 ) ) ;
#31321 = CARTESIAN_POINT ( 'NONE',  ( 762.1177392798416577, -138.5545181178802636, -309.8865473780659272 ) ) ;
#31322 = CARTESIAN_POINT ( 'NONE',  ( 812.3518521366052028, -49.09997266333511590, 326.5853460496235243 ) ) ;
#31324 = LINE ( 'NONE', #27627, #10009 ) ;
#31323 = DIRECTION ( 'NONE',  ( -1.000000000000000000, -0.000000000000000000, -0.000000000000000000 ) ) ;
#31325 = CARTESIAN_POINT ( 'NONE',  ( 756.1348686366196716, -281.2601417444139997, -347.5531968255698416 ) ) ;
#31326 = CARTESIAN_POINT ( 'NONE',  ( 790.8050863131179540, -452.8379544210779954, -362.5841948692291226 ) ) ;
#31327 = CARTESIAN_POINT ( 'NONE',  ( 745.1792804349281596, -158.1908817542438612, -343.7566961878542884 ) ) ;
#31328 = CARTESIAN_POINT ( 'NONE',  ( 51.16348990802859475, 256.5000000000000568, -202.7499999999944009 ) ) ;
#31329 = CARTESIAN_POINT ( 'NONE',  ( 939.9999999999992042, 74.99999999999984368, -360.0000000000000000 ) ) ;
#31330 = CARTESIAN_POINT ( 'NONE',  ( 763.8424801807145741, -354.0090635724250774, 320.5453621957614700 ) ) ;
#31331 = CARTESIAN_POINT ( 'NONE',  ( 744.6391490659812007, -350.7363362996978253, 338.7502325331110455 ) ) ;
#31332 = AXIS2_PLACEMENT_3D ( 'NONE', #41567, #24451, #16867 ) ;
#31333 = CARTESIAN_POINT ( 'NONE',  ( 796.7737145352015204, -188.6346026584199365, -370.7187646348536987 ) ) ;
#31334 = CARTESIAN_POINT ( 'NONE',  ( 999.9999999999992042, 248.9999999999998863, 359.0000000000000000 ) ) ;
#31335 = VECTOR ( 'NONE', #9526, 1000.000000000000000 ) ;
#31336 = CARTESIAN_POINT ( 'NONE',  ( 799.9636004259356241, -118.9181544815167229, 311.2241431872006956 ) ) ;
#31337 = CARTESIAN_POINT ( 'NONE',  ( 808.3070685750230950, -306.9982390220558273, -361.1904061080339261 ) ) ;
#31338 = CARTESIAN_POINT ( 'NONE',  ( 779.9999999999992042, 126.4563064324884465, -339.9999999999999432 ) ) ;
#31339 = DIRECTION ( 'NONE',  ( 0.000000000000000000, 0.9235249282889856914, 0.3835384033298670503 ) ) ;
#31340 = CARTESIAN_POINT ( 'NONE',  ( 755.5713283507202505, -173.3618753856927128, 334.6858677611754729 ) ) ;
#31341 = EDGE_LOOP ( 'NONE', ( #15310, #18381, #41477, #18335 ) ) ;
#31342 = CARTESIAN_POINT ( 'NONE',  ( 773.7305795820266212, -441.2817908451521021, 374.8230680027170365 ) ) ;
#31343 = CARTESIAN_POINT ( 'NONE',  ( 746.0683387631852383, -379.4419599262318457, -331.3260364891676204 ) ) ;
#31344 = CARTESIAN_POINT ( 'NONE',  ( 772.5602148656447525, -129.7255117493292289, -305.7998596910095443 ) ) ;
#31345 = AXIS2_PLACEMENT_3D ( 'NONE', #10553, #45687, #17735 ) ;
#31346 = CARTESIAN_POINT ( 'NONE',  ( 787.5162901302840055, -395.3618753856918602, -305.4481719005792684 ) ) ;
#31347 = FACE_OUTER_BOUND ( 'NONE', #41199, .T. ) ;
#31348 = CARTESIAN_POINT ( 'NONE',  ( 793.4146539503750546, -1.987414471687640294, 307.6481478633938877 ) ) ;
#31349 = ORIENTED_EDGE ( 'NONE', *, *, #19921, .F. ) ;
#31350 = AXIS2_PLACEMENT_3D ( 'NONE', #37541, #19988, #34064 ) ;
#31351 = CIRCLE ( 'NONE', #39490, 10.00000000000000888 ) ;
#31352 = CARTESIAN_POINT ( 'NONE',  ( 781.2497674668890113, -156.3510508353235480, -375.3608509340180603 ) ) ;
#31353 = DIRECTION ( 'NONE',  ( -0.000000000000000000, 1.000000000000000000, -0.000000000000000000 ) ) ;
#31354 = CARTESIAN_POINT ( 'NONE',  ( 810.1134526219336749, -296.5328690171411949, 357.8822607201570349 ) ) ;
#31355 = CARTESIAN_POINT ( 'NONE',  ( 756.3353852180820240, -125.9073299311474159, 331.1735550268787733 ) ) ;
#31356 = ORIENTED_EDGE ( 'NONE', *, *, #21571, .F. ) ;
#31357 = CARTESIAN_POINT ( 'NONE',  ( 805.1927285166397041, -304.8164208402376403, 341.8018195045277707 ) ) ;
#31358 = VECTOR ( 'NONE', #23819, 1000.000000000000000 ) ;
#31359 = CARTESIAN_POINT ( 'NONE',  ( 782.5225473063381969, -22.27096629478410250, -375.2698199232970637 ) ) ;
#31360 = DIRECTION ( 'NONE',  ( -0.000000000000000000, 1.000000000000000000, -0.000000000000000000 ) ) ;
#31361 = AXIS2_PLACEMENT_3D ( 'NONE', #4357, #28607, #43148 ) ;
#31362 = ORIENTED_EDGE ( 'NONE', *, *, #3268, .T. ) ;
#31363 = CARTESIAN_POINT ( 'NONE',  ( 814.4686193811664907, -411.2817908451521589, -346.2056067578752732 ) ) ;
#31364 = AXIS2_PLACEMENT_3D ( 'NONE', #24742, #42757, #38860 ) ;
#31365 = ORIENTED_EDGE ( 'NONE', *, *, #41330, .F. ) ;
#31366 = CARTESIAN_POINT ( 'NONE',  ( 804.4286716492782716, -17.36187538569322086, 345.3141322388244703 ) ) ;
#31367 = CARTESIAN_POINT ( 'NONE',  ( 756.5762568750052424, -267.1800572038742985, -348.7366044899774238 ) ) ;
#31369 = CARTESIAN_POINT ( 'NONE',  ( 808.7758568127978833, -268.1692326535049347, 320.0363995740631822 ) ) ;
#31368 = CARTESIAN_POINT ( 'NONE',  ( 767.6429770376291799, -345.1800572038739574, 306.8695393053162093 ) ) ;
#31370 = CARTESIAN_POINT ( 'NONE',  ( 804.6971507214547046, -243.2817908451526705, -344.0799538623459739 ) ) ;
#31371 = CARTESIAN_POINT ( 'NONE',  ( 754.8072714833581358, -244.8164208402378961, -338.1981804954720587 ) ) ;
#31372 = CARTESIAN_POINT ( 'NONE',  ( 785.3687786644885591, -443.3618753856917465, -315.3201227861280813 ) ) ;
#31373 = CARTESIAN_POINT ( 'NONE',  ( 778.2165204200184689, -94.81642084023843609, -364.9363028652563230 ) ) ;
#31374 = AXIS2_PLACEMENT_3D ( 'NONE', #37415, #26335, #16389 ) ;
#31375 = CARTESIAN_POINT ( 'NONE',  ( 801.9419747391806368, -234.4527844766016358, 351.9812246680014027 ) ) ;
#31376 = ORIENTED_EDGE ( 'NONE', *, *, #43267, .T. ) ;
#31377 = CARTESIAN_POINT ( 'NONE',  ( 763.2262854647970016, -392.6346026584193396, 309.2812353651462445 ) ) ;
#31378 = CIRCLE ( 'NONE', #8513, 2.749999999999919176 ) ;
#31379 = CYLINDRICAL_SURFACE ( 'NONE', #24819, 2.749999999999835687 ) ;
#31380 = CARTESIAN_POINT ( 'NONE',  ( 791.0478386215596629, -45.82724539060783542, -306.7653713866226326 ) ) ;
#31381 = CARTESIAN_POINT ( 'NONE',  ( -338.8365100919713200, 256.5000000000001137, -206.1189999999917859 ) ) ;
#31382 = DIRECTION ( 'NONE',  ( 0.000000000000000000, -1.000000000000000000, 0.000000000000000000 ) ) ;
#31383 = VECTOR ( 'NONE', #33559, 1000.000000000000000 ) ;
#31384 = CARTESIAN_POINT ( 'NONE',  ( 783.0745993439762742, -224.1908817542436623, 365.1016975059196739 ) ) ;
#31385 = CARTESIAN_POINT ( 'NONE',  ( 802.1676090361156639, -134.6346026584201070, 327.8955696845344505 ) ) ;
#31386 = VERTEX_POINT ( 'NONE', #108 ) ;
#31387 = CARTESIAN_POINT ( 'NONE',  ( 769.9779781133707957, 4.900027336664720679, -316.7813123517150871 ) ) ;
#31388 = CARTESIAN_POINT ( 'NONE',  ( 811.0346526505617248, -62.63460265842032726, -323.0537975583478101 ) ) ;
#31389 = CARTESIAN_POINT ( 'NONE',  ( 764.0069404352550464, -303.0783235625957559, 359.2566176426627180 ) ) ;
#31390 = CARTESIAN_POINT ( 'NONE',  ( 803.4237431249931660, -447.1800572038736732, -331.2633955100225194 ) ) ;
#31391 = CARTESIAN_POINT ( 'NONE',  ( 766.4474001241216001, -19.09997266333520116, 307.3154664389482491 ) ) ;
#31392 = CARTESIAN_POINT ( 'NONE',  ( 808.3070685750230950, -210.9982390220561967, -361.1904061080339261 ) ) ;
#31393 = EDGE_CURVE ( 'NONE', #15014, #13142, #39553, .T. ) ;
#31394 = CARTESIAN_POINT ( 'NONE',  ( 814.9108240113580450, -184.2709662947835909, 337.5031285880265273 ) ) ;
#31395 = CARTESIAN_POINT ( 'NONE',  ( 778.2165204200184689, -94.81642084023843609, 364.9363028652563230 ) ) ;
#31396 = DIRECTION ( 'NONE',  ( -0.000000000000000000, 1.000000000000000000, -0.000000000000000000 ) ) ;
#31397 = AXIS2_PLACEMENT_3D ( 'NONE', #1218, #39593, #7702 ) ;
#31398 = DIRECTION ( 'NONE',  ( -0.000000000000000000, -4.857225732735055920E-15, 1.000000000000000000 ) ) ;
#31399 = CARTESIAN_POINT ( 'NONE',  ( 747.3154664389472828, -283.9874144716867477, -326.4474001241230781 ) ) ;
#31400 = VECTOR ( 'NONE', #19787, 1000.000000000000000 ) ;
#31401 = CARTESIAN_POINT ( 'NONE',  ( 776.2046728542105711, -428.1908817542430938, 304.8212110874238761 ) ) ;
#31402 = CARTESIAN_POINT ( 'NONE',  ( 744.7301800767019131, -292.8164208402376971, -337.4774526936615757 ) ) ;
#31403 = DIRECTION ( 'NONE',  ( 1.000000000000000000, 0.000000000000000000, -0.000000000000000000 ) ) ;
#31404 = CARTESIAN_POINT ( 'NONE',  ( 757.2208543904082489, -352.7146871989593251, 350.9844846989624330 ) ) ;
#31405 = CARTESIAN_POINT ( 'NONE',  ( 748.9653473494365699, -50.63460265842038410, 356.9462024416520762 ) ) ;
#31406 = CARTESIAN_POINT ( 'NONE',  ( 803.4237431249931660, -375.1800572038739574, -331.2633955100225194 ) ) ;
#31407 = CARTESIAN_POINT ( 'NONE',  ( 758.6633372737375112, -20.53286901714212931, 326.9102291470432533 ) ) ;
#31408 = CARTESIAN_POINT ( 'NONE',  ( 800.1688906516307043, -34.16923265350572336, -369.0717654672308186 ) ) ;
#31409 = CARTESIAN_POINT ( 'NONE',  ( 795.9930595647434757, -195.0783235625961538, -320.7433823573372820 ) ) ;
#31410 = CARTESIAN_POINT ( 'NONE',  ( 795.6651683502461765, -178.7146871989598083, 371.3240766477733814 ) ) ;
#31411 = VECTOR ( 'NONE', #16017, 1000.000000000000000 ) ;
#31412 = ORIENTED_EDGE ( 'NONE', *, *, #19891, .T. ) ;
#31413 = CARTESIAN_POINT ( 'NONE',  ( 754.8983024940795303, -186.8965053807779668, -336.9254006560228163 ) ) ;
#31414 = CARTESIAN_POINT ( 'NONE',  ( 781.7834795799800531, -202.8164208402380950, 315.0636971347436202 ) ) ;
#31415 = CIRCLE ( 'NONE', #29226, 30.00000000000008171 ) ;
#31416 = EDGE_CURVE ( 'NONE', #41897, #21010, #4841, .T. ) ;
#31417 = CARTESIAN_POINT ( 'NONE',  ( 749.8865473780648472, -44.53286901714205470, -322.1177392798429082 ) ) ;
#31418 = CARTESIAN_POINT ( 'NONE',  ( 797.6776695296629214, -331.5436935675104451, 357.6776695296636603 ) ) ;
#31419 = CARTESIAN_POINT ( 'NONE',  ( 311.1634899080286232, 260.0000000000000000, -199.9999999999963336 ) ) ;
#31420 = EDGE_LOOP ( 'NONE', ( #2604, #1027, #32044, #24649, #8655, #9028 ) ) ;
#31421 = CARTESIAN_POINT ( 'NONE',  ( 763.2154366446407039, -45.62377810805114109, 321.4292242960311228 ) ) ;
#31422 = CARTESIAN_POINT ( 'NONE',  ( 805.6418435158337843, -293.4636090269707438, -363.8556311672236916 ) ) ;
#31423 = EDGE_CURVE ( 'NONE', #43869, #12054, #28977, .T. ) ;
#31424 = CARTESIAN_POINT ( 'NONE',  ( 745.4481719005789273, -267.7255117493287457, 347.5162901302853697 ) ) ;
#31425 = CARTESIAN_POINT ( 'NONE',  ( 787.5531968255692163, -333.8272453906070041, 316.1348686366205811 ) ) ;
#31426 = CARTESIAN_POINT ( 'NONE',  ( 756.1443688327750579, 26.37622189194863509, 314.3581564841659315 ) ) ;
#31427 = CARTESIAN_POINT ( 'NONE',  ( 793.0897708529556667, -150.5545181178802352, -361.3366627262616362 ) ) ;
#31428 = CARTESIAN_POINT ( 'NONE',  ( 755.3201227861273992, -147.7255117493291152, -345.3687786644892981 ) ) ;
#31429 = CARTESIAN_POINT ( 'NONE',  ( 765.0180583372156207, -360.9982390220557704, -360.0135310231089534 ) ) ;
#31430 = EDGE_LOOP ( 'NONE', ( #43462, #37841, #31142, #32780 ) ) ;
#31431 = AXIS2_PLACEMENT_3D ( 'NONE', #45129, #2627, #6550 ) ;
#31432 = CARTESIAN_POINT ( 'NONE',  ( 758.8095938919642549, -272.0891481129651197, 311.6929314249763365 ) ) ;
#31433 = CARTESIAN_POINT ( 'NONE',  ( 770.0799878456142551, -325.9874144716865771, 362.9823548866085616 ) ) ;
#31434 = VECTOR ( 'NONE', #39649, 1000.000000000000000 ) ;
#31435 = DIRECTION ( 'NONE',  ( -1.000000000000000000, -0.000000000000000000, -0.000000000000000000 ) ) ;
#31436 = CARTESIAN_POINT ( 'NONE',  ( 757.4527132478984868, -112.3726999360621761, 329.1273215169538844 ) ) ;
#31437 = CARTESIAN_POINT ( 'NONE',  ( 774.6858677611749044, -9.725511749329603717, 315.5713283507209894 ) ) ;
#31438 = ORIENTED_EDGE ( 'NONE', *, *, #17957, .F. ) ;
#31439 = CARTESIAN_POINT ( 'NONE',  ( 812.3518521366052028, -385.0999726633340856, -326.5853460496235243 ) ) ;
#31440 = CARTESIAN_POINT ( 'NONE',  ( -199.6009925648704098, 290.0000000000001137, -244.9999999999999716 ) ) ;
#31441 = EDGE_CURVE ( 'NONE', #8149, #30790, #39619, .T. ) ;
#31442 = CARTESIAN_POINT ( 'NONE',  ( 810.4231160770870019, -240.5545181178798941, 321.9338519418446936 ) ) ;
#31443 = CARTESIAN_POINT ( 'NONE',  ( 803.8651313633788504, -173.2601417444143692, 332.4468031744301015 ) ) ;
#31444 = MECHANICAL_DESIGN_GEOMETRIC_PRESENTATION_REPRESENTATION (  '', ( #8579 ), #38817 ) ;
#31445 = CARTESIAN_POINT ( 'NONE',  ( 804.4286716492782716, -329.3618753856922581, -345.3141322388244703 ) ) ;
#31446 = EDGE_CURVE ( 'NONE', #5298, #10119, #40050, .T. ) ;
#31447 = CARTESIAN_POINT ( 'NONE',  ( 775.8780910478218402, -225.2817908451527273, -364.9511171171680530 ) ) ;
#31448 = VECTOR ( 'NONE', #23973, 1000.000000000000000 ) ;
#31449 = CARTESIAN_POINT ( 'NONE',  ( 772.4837098697144029, -23.36187538569318889, 374.5518280994205611 ) ) ;
#31450 = ADVANCED_FACE ( 'NONE', ( #9313 ), #15563, .F. ) ;
#31451 = CARTESIAN_POINT ( 'NONE',  ( 796.7737145352015204, -68.63460265842033436, 370.7187646348536987 ) ) ;
#31452 = CARTESIAN_POINT ( 'NONE',  ( 775.4999999999993179, -110.5936016518799221, 750.6326042729449455 ) ) ;
#31453 = CARTESIAN_POINT ( 'NONE',  ( 787.4397851343537695, -405.7255117493283478, -374.2001403089903988 ) ) ;
#31454 = CARTESIAN_POINT ( 'NONE',  ( 794.9999999999993179, -365.3551492539851893, -18.13243251470705886 ) ) ;
#31455 = CARTESIAN_POINT ( 'NONE',  ( 793.5525998758768083, -343.0999726633342561, 372.6845335610516941 ) ) ;
#31456 = CARTESIAN_POINT ( 'NONE',  ( 799.9999999999993179, 205.0000000000000568, -255.0000000000000000 ) ) ;
#31457 = CARTESIAN_POINT ( 'NONE',  ( 754.9967657858570647, -289.5436935675103882, 365.0032342141425374 ) ) ;
#31458 = CARTESIAN_POINT ( 'NONE',  ( 787.5162901302840055, -59.36187538569306810, -305.4481719005792684 ) ) ;
#31459 = CARTESIAN_POINT ( 'NONE',  ( 774.6858677611749044, -273.7255117493288026, -315.5713283507209894 ) ) ;
#31460 = FACE_BOUND ( 'NONE', #17404, .T. ) ;
#31461 = CARTESIAN_POINT ( 'NONE',  ( 756.5762568750052424, -411.1800572038738437, 348.7366044899774238 ) ) ;
#31462 = CARTESIAN_POINT ( 'NONE',  ( 772.4468031744293057, -153.8272453906075157, 363.8651313633793620 ) ) ;
#31463 = CARTESIAN_POINT ( 'NONE',  ( 756.1348686366196716, -89.26014174441463922, -347.5531968255698416 ) ) ;
#31464 = CARTESIAN_POINT ( 'NONE',  ( 795.6651683502461765, -82.71468719896012090, 371.3240766477733814 ) ) ;
#31465 = CARTESIAN_POINT ( 'NONE',  ( 785.3687786644885591, -395.3618753856919739, 315.3201227861280813 ) ) ;
#31466 = AXIS2_PLACEMENT_3D ( 'NONE', #23114, #8832, #4909 ) ;
#31467 = CARTESIAN_POINT ( 'NONE',  ( 808.0189434323515343, 9.910851887033969021, 319.0252816721025511 ) ) ;
#31468 = ADVANCED_FACE ( 'NONE', ( #29643 ), #29870, .T. ) ;
#31469 = CARTESIAN_POINT ( 'NONE',  ( -180.7583438952258348, 394.6698570112193920, -274.9999999999999432 ) ) ;
#31470 = CARTESIAN_POINT ( 'NONE',  ( 771.1735550268778070, -417.1800572038736163, 316.3353852180827630 ) ) ;
#31471 = EDGE_LOOP ( 'NONE', ( #27200, #44763, #31124, #1693 ) ) ;
#31472 = CARTESIAN_POINT ( 'NONE',  ( 759.7806653035534055, -54.99823902205672255, -324.8639956371180801 ) ) ;
#31473 = CIRCLE ( 'NONE', #20384, 2.749999999999891642 ) ;
#31474 = ADVANCED_FACE ( 'NONE', ( #1909 ), #29430, .F. ) ;
#31475 = CARTESIAN_POINT ( 'NONE',  ( 770.0799878456142551, -373.9874144716864066, -362.9823548866085616 ) ) ;
#31477 = CARTESIAN_POINT ( 'NONE',  ( 759.7806653035535192, -222.9982390220561683, 324.8639956371181370 ) ) ;
#31476 = CARTESIAN_POINT ( 'NONE',  ( 757.8323909638827445, -242.6346026584197659, 352.1044303154654358 ) ) ;
#31478 = CARTESIAN_POINT ( 'NONE',  ( 773.7943932421234194, -383.8055962898682765, -305.5313806188329409 ) ) ;
#31479 = CARTESIAN_POINT ( 'NONE',  ( 759.9999999999992042, -462.9681489794448339, 362.3606797749978909 ) ) ;
#31480 = VERTEX_POINT ( 'NONE', #22707 ) ;
#31481 = CARTESIAN_POINT ( 'NONE',  ( 774.6858677611749044, -393.7255117493283478, 315.5713283507209894 ) ) ;
#31482 = CIRCLE ( 'NONE', #30021, 8.024999999999948841 ) ;
#31483 = ORIENTED_EDGE ( 'NONE', *, *, #35606, .T. ) ;
#31484 = AXIS2_PLACEMENT_3D ( 'NONE', #28361, #39237, #32998 ) ;
#31485 = EDGE_CURVE ( 'NONE', #17814, #28471, #12099, .T. ) ;
#31486 = CARTESIAN_POINT ( 'NONE',  ( 813.1304606946830518, -257.9073299311469896, -352.3570229623690580 ) ) ;
#31487 = CARTESIAN_POINT ( 'NONE',  ( 812.7932403749906598, -135.1800572038746679, 327.7687537140311633 ) ) ;
#31488 = ORIENTED_EDGE ( 'NONE', *, *, #8063, .F. ) ;
#31489 = CARTESIAN_POINT ( 'NONE',  ( 757.8323909638828582, -218.6346026584198228, -352.1044303154654358 ) ) ;
#31490 = ORIENTED_EDGE ( 'NONE', *, *, #29361, .T. ) ;
#31491 = CARTESIAN_POINT ( 'NONE',  ( 762.3223304703356007, -343.5436935675103314, -322.3223304703362828 ) ) ;
#31492 = CARTESIAN_POINT ( 'NONE',  ( 778.2165204200184689, 1.183579159761269040, -364.9363028652563230 ) ) ;
#31493 = CARTESIAN_POINT ( 'NONE',  ( 804.1601925771018387, -223.4419599262323857, 346.5483106153029098 ) ) ;
#31494 = CARTESIAN_POINT ( 'NONE',  ( -521.6730038022808458, 230.0000000000002274, 339.9999999999999432 ) ) ;
#31495 = CARTESIAN_POINT ( 'NONE',  ( 784.4999999999993179, -496.5085659523897448, -356.8883017825714319 ) ) ;
#31496 = ORIENTED_EDGE ( 'NONE', *, *, #40773, .T. ) ;
#31497 = CARTESIAN_POINT ( 'NONE',  ( 766.9102291470427417, -450.5545181178793541, -318.6633372737382501 ) ) ;
#31498 = DIRECTION ( 'NONE',  ( -1.880165489482579047E-16, -1.000000000000000000, -0.000000000000000000 ) ) ;
#31499 = CARTESIAN_POINT ( 'NONE',  ( 989.9999999999992042, 469.9999999999999432, -360.0000000000000000 ) ) ;
#31500 = ORIENTED_EDGE ( 'NONE', *, *, #3230, .F. ) ;
#31501 = CARTESIAN_POINT ( 'NONE',  ( 795.8262568251477660, -262.3726999360617924, -308.3538107759623585 ) ) ;
#31502 = CARTESIAN_POINT ( 'NONE',  ( 795.8262568251477660, -142.3726999360620766, 308.3538107759623585 ) ) ;
#31504 = CARTESIAN_POINT ( 'NONE',  ( 767.8955696845333705, -216.4527844766016926, -362.1676090361162323 ) ) ;
#31503 = DIRECTION ( 'NONE',  ( 1.000000000000000000, 0.000000000000000000, -0.000000000000000000 ) ) ;
#31505 = CARTESIAN_POINT ( 'NONE',  ( 763.2154366446407039, -405.6237781080500326, -321.4292242960311228 ) ) ;
#31506 = EDGE_CURVE ( 'NONE', #6890, #12560, #11870, .T. ) ;
#31507 = DIRECTION ( 'NONE',  ( -0.000000000000000000, 1.000000000000000000, -0.000000000000000000 ) ) ;
#31508 = DIRECTION ( 'NONE',  ( -0.000000000000000000, 1.000000000000000000, -0.000000000000000000 ) ) ;
#31509 = CARTESIAN_POINT ( 'NONE',  ( 804.6971507214547046, -123.2817908451530542, -344.0799538623459739 ) ) ;
#31510 = AXIS2_PLACEMENT_3D ( 'NONE', #42695, #35069, #2982 ) ;
#31511 = CARTESIAN_POINT ( 'NONE',  ( 804.1009440267234822, -383.4636090269704596, 314.0944755984392600 ) ) ;
#31512 = CARTESIAN_POINT ( 'NONE',  ( 190.7583438952259485, 394.6698570112193920, -244.9999999999999716 ) ) ;
#31513 = CARTESIAN_POINT ( 'NONE',  ( 783.7566961878529810, 23.10349461922137237, -305.1792804349288417 ) ) ;
#31514 = CARTESIAN_POINT ( 'NONE',  ( 782.4968714119720516, -298.8164208402377540, -305.0891759886411023 ) ) ;
#31515 = CARTESIAN_POINT ( 'NONE',  ( 779.9999999999992042, -462.9681489794448339, 339.9999999999999432 ) ) ;
#31516 = CARTESIAN_POINT ( 'NONE',  ( 804.9363028652555840, 7.729033705215793582, 338.2165204200192079 ) ) ;
#31517 = CARTESIAN_POINT ( 'NONE',  ( 800.0135310231082713, -86.08914811296573077, -325.0180583372163028 ) ) ;
#31518 = VECTOR ( 'NONE', #9082, 1000.000000000000000 ) ;
#31519 = CARTESIAN_POINT ( 'NONE',  ( 754.3581564841646241, -257.4636090269708575, 316.1443688327762516 ) ) ;
#31520 = CARTESIAN_POINT ( 'NONE',  ( 744.8212110874229666, -186.8965053807779668, -336.2046728542121627 ) ) ;
#31521 = CARTESIAN_POINT ( 'NONE',  ( 751.9810565676468741, -194.0891481129654039, 360.9747183278973921 ) ) ;
#31522 = CARTESIAN_POINT ( 'NONE',  ( 748.9653473494363425, -434.6346026584190554, -356.9462024416521331 ) ) ;
#31523 = CIRCLE ( 'NONE', #26338, 2.749999999999919176 ) ;
#31524 = CARTESIAN_POINT ( 'NONE',  ( -26.63011601220122060, -512.9681489794448908, -329.9999999999999432 ) ) ;
#31525 = CARTESIAN_POINT ( 'NONE',  ( 756.3353852180819104, -293.9073299311468759, 331.1735550268788302 ) ) ;
#31526 = CARTESIAN_POINT ( 'NONE',  ( 763.8424801807145741, -90.00906357242590161, 320.5453621957614700 ) ) ;
#31527 = CARTESIAN_POINT ( 'NONE',  ( 758.0580252608178853, -438.4527844766009821, -328.0187753319985404 ) ) ;
#31528 = ADVANCED_BREP_SHAPE_REPRESENTATION ( '', ( #32965, #26858 ), #32022 ) ;
#31529 = FACE_OUTER_BOUND ( 'NONE', #2752, .T. ) ;
#31530 = EDGE_CURVE ( 'NONE', #16954, #3483, #9075, .T. ) ;
#31531 = DIRECTION ( 'NONE',  ( 0.000000000000000000, -0.6438296778008192334, -0.7651688349527138167 ) ) ;
#31533 = CARTESIAN_POINT ( 'NONE',  ( 781.8018195045266339, -310.2709662947832499, 365.1927285166406705 ) ) ;
#31532 = CARTESIAN_POINT ( 'NONE',  ( 790.8726784830453198, -130.7146871989599504, 362.5472867521010585 ) ) ;
#31534 = ORIENTED_EDGE ( 'NONE', *, *, #35423, .F. ) ;
#31535 = EDGE_CURVE ( 'NONE', #36984, #38205, #13719, .T. ) ;
#31536 = CARTESIAN_POINT ( 'NONE',  ( 805.1016975059191054, -270.8965053807777394, -343.0745993439771837 ) ) ;
#31537 = CARTESIAN_POINT ( 'NONE',  ( 771.1735550268778070, -81.18005720387481006, 316.3353852180827630 ) ) ;
#31538 = CARTESIAN_POINT ( 'NONE',  ( 746.0683387631852383, -283.4419599262321867, -331.3260364891676204 ) ) ;
#31539 = DIRECTION ( 'NONE',  ( -1.000000000000000000, -0.000000000000000000, -0.000000000000000000 ) ) ;
#31540 = CARTESIAN_POINT ( 'NONE',  ( 748.3538107759620743, -400.7146871989590977, 355.8262568251490165 ) ) ;
#31541 = ORIENTED_EDGE ( 'NONE', *, *, #8626, .F. ) ;
#31542 = CARTESIAN_POINT ( 'NONE',  ( 795.1360043628807261, -284.0891481129650629, 360.2193346964456282 ) ) ;
#31543 = CARTESIAN_POINT ( 'NONE',  ( 805.0264073115434940, -54.35105083532383219, -339.4763451958999099 ) ) ;
#31544 = CARTESIAN_POINT ( 'NONE',  ( 755.3201227861273992, -195.7255117493289731, -345.3687786644892981 ) ) ;
#31545 = CARTESIAN_POINT ( 'NONE',  ( 803.6646147819161570, -401.9073299311463643, 348.8264449731210561 ) ) ;
#31546 = EDGE_CURVE ( 'NONE', #8526, #20178, #10749, .T. ) ;
#31547 = CARTESIAN_POINT ( 'NONE',  ( 745.4481719005789273, -99.72551174932928575, -347.5162901302853129 ) ) ;
#31548 = CARTESIAN_POINT ( 'NONE',  ( 756.5762568750052424, -123.1800572038747106, -348.7366044899774238 ) ) ;
#31549 = ORIENTED_EDGE ( 'NONE', *, *, #33987, .T. ) ;
#31550 = AXIS2_PLACEMENT_3D ( 'NONE', #27727, #27490, #9717 ) ;
#31551 = CARTESIAN_POINT ( 'NONE',  ( 755.8894580844503253, -375.8272453906069472, -332.3691319403863531 ) ) ;
#31553 = CARTESIAN_POINT ( 'NONE',  ( 793.0897708529556667, -438.5545181178793541, 361.3366627262616362 ) ) ;
#31552 = CARTESIAN_POINT ( 'NONE',  ( 797.8594530101008786, -133.5436935675110135, 322.1405469898980982 ) ) ;
#31554 = CARTESIAN_POINT ( 'NONE',  ( 756.1348686366196716, -137.2601417444144829, 347.5531968255698416 ) ) ;
#31557 = CARTESIAN_POINT ( 'NONE',  ( 747.3154664389472828, -379.9874144716865203, 326.4474001241230781 ) ) ;
#31556 = FACE_OUTER_BOUND ( 'NONE', #29211, .T. ) ;
#31555 = DIRECTION ( 'NONE',  ( -0.000000000000000000, -3.700743415417198493E-16, 1.000000000000000000 ) ) ;
#31558 = ORIENTED_EDGE ( 'NONE', *, *, #20111, .T. ) ;
#31559 = CARTESIAN_POINT ( 'NONE',  ( 787.5531968255692163, -357.8272453906068904, -316.1348686366205811 ) ) ;
#31560 = CARTESIAN_POINT ( 'NONE',  ( 804.9363028652555840, -352.2709662947830225, -338.2165204200192079 ) ) ;
#31561 = CARTESIAN_POINT ( 'NONE',  ( 795.8262568251477660, -166.3726999360620198, -308.3538107759623585 ) ) ;
#31562 = CARTESIAN_POINT ( 'NONE',  ( 746.4236121716829757, -39.82724539060786384, 328.8385539511384650 ) ) ;
#31564 = CYLINDRICAL_SURFACE ( 'NONE', #1141, 2.749999999999863665 ) ;
#31563 = LINE ( 'NONE', #20692, #32216 ) ;
#31565 = CARTESIAN_POINT ( 'NONE',  ( 799.4546378042377910, -297.0783235625957559, -356.1575198192848006 ) ) ;
#31566 = CARTESIAN_POINT ( 'NONE',  ( 959.5497976682736407, 229.9999999999998579, -122.7905160835436362 ) ) ;
#31567 = CARTESIAN_POINT ( 'NONE',  ( 744.6391490659812007, -158.7363362996984222, -338.7502325331110455 ) ) ;
#31568 = CARTESIAN_POINT ( 'NONE',  ( 939.9999999999993179, -179.7356316342496712, -69.11609595480024382 ) ) ;
#31569 = DIRECTION ( 'NONE',  ( 0.000000000000000000, 0.000000000000000000, 1.000000000000000000 ) ) ;
#31570 = CARTESIAN_POINT ( 'NONE',  ( 763.8424801807145741, -378.0090635724250774, 320.5453621957614700 ) ) ;
#31571 = CARTESIAN_POINT ( 'NONE',  ( 771.3260364891663130, -331.6454272087888171, 306.0683387631859773 ) ) ;
#31572 = CARTESIAN_POINT ( 'NONE',  ( 745.0891759886404770, -196.2709662947835909, -342.4968714119734159 ) ) ;
#31573 = CARTESIAN_POINT ( 'NONE',  ( 989.9999999999992042, -428.4497686941065808, 352.6378164459125060 ) ) ;
#31574 = CARTESIAN_POINT ( 'NONE',  ( 749.5768839229115201, -132.5545181178802920, 358.0661480581553064 ) ) ;
#31575 = CARTESIAN_POINT ( 'NONE',  ( 767.6429770376289525, -345.1800572038739006, -306.8695393053162093 ) ) ;
#31576 = DIRECTION ( 'NONE',  ( 0.000000000000000000, 0.000000000000000000, 1.000000000000000000 ) ) ;
#31577 = DIRECTION ( 'NONE',  ( 0.000000000000000000, 0.000000000000000000, 1.000000000000000000 ) ) ;
#31578 = CARTESIAN_POINT ( 'NONE',  ( 774.6312213355099630, -191.3618753856925991, 364.6798772138717482 ) ) ;
#31579 = EDGE_LOOP ( 'NONE', ( #6138, #6503, #41146, #40953 ) ) ;
#31580 = CARTESIAN_POINT ( 'NONE',  ( 793.5525998758768083, -415.0999726633340288, 372.6845335610516941 ) ) ;
#31581 = CARTESIAN_POINT ( 'NONE',  ( 807.5423716828161105, -393.0783235625954717, -362.2119215644372048 ) ) ;
#31582 = VECTOR ( 'NONE', #31339, 1000.000000000000114 ) ;
#31583 = CARTESIAN_POINT ( 'NONE',  ( 808.3070685750230950, -138.9982390220563957, -361.1904061080339261 ) ) ;
#31584 = CARTESIAN_POINT ( 'NONE',  ( 744.7301800767019131, -436.8164208402372992, -337.4774526936615757 ) ) ;
#31585 = DIRECTION ( 'NONE',  ( 0.000000000000000000, 0.000000000000000000, 1.000000000000000000 ) ) ;
#31586 = CARTESIAN_POINT ( 'NONE',  ( 752.4576283171824116, 2.921676437403253779, 317.7880784355627952 ) ) ;
#31587 = ORIENTED_EDGE ( 'NONE', *, *, #10295, .F. ) ;
#31588 = CARTESIAN_POINT ( 'NONE',  ( 788.7631598425961101, -193.4419599262325278, -305.7194118038759143 ) ) ;
#31589 =( LENGTH_UNIT ( ) NAMED_UNIT ( * ) SI_UNIT ( .MILLI., .METRE. ) );
#31590 = CARTESIAN_POINT ( 'NONE',  ( 813.9316612368132837, -319.4419599262320730, 348.6739635108323228 ) ) ;
#31591 = CARTESIAN_POINT ( 'NONE',  ( 804.4286716492782716, -113.3618753856929260, 345.3141322388244703 ) ) ;
#31592 = ORIENTED_EDGE ( 'NONE', *, *, #42741, .T. ) ;
#31593 = CARTESIAN_POINT ( 'NONE',  ( 774.6312213355099630, -287.3618753856923718, 364.6798772138717482 ) ) ;
#31594 = CARTESIAN_POINT ( 'NONE',  ( 772.5602148656447525, -9.725511749329603717, -305.7998596910095443 ) ) ;
#31595 = CARTESIAN_POINT ( 'NONE',  ( 789.5584187865343893, -452.9681489794450613, 363.1011989789364520 ) ) ;
#31596 = ORIENTED_EDGE ( 'NONE', *, *, #19046, .F. ) ;
#31597 = CARTESIAN_POINT ( 'NONE',  ( 797.8822607201568644, -414.5545181178795247, -370.1134526219340160 ) ) ;
#31598 = ORIENTED_EDGE ( 'NONE', *, *, #30859, .T. ) ;
#31599 = CARTESIAN_POINT ( 'NONE',  ( 804.9363028652555840, -16.27096629478413092, 338.2165204200192079 ) ) ;
#31600 = CARTESIAN_POINT ( 'NONE',  ( 778.1981804954714335, -274.2709662947833067, -314.8072714833589885 ) ) ;
#31602 = CARTESIAN_POINT ( 'NONE',  ( 758.0141637701419768, -255.0783235625958980, 367.2620300519063790 ) ) ;
#31601 = CARTESIAN_POINT ( 'NONE',  ( 745.4481719005789273, -363.7255117493284615, 347.5162901302853697 ) ) ;
#31603 = CARTESIAN_POINT ( 'NONE',  ( 800.1688906516307043, -82.16923265350558836, 369.0717654672308186 ) ) ;
#31604 = CARTESIAN_POINT ( 'NONE',  ( 757.0176451133909268, -253.0999726633345119, -349.9200121543848354 ) ) ;
#31605 = CARTESIAN_POINT ( 'NONE',  ( 768.0187753319979720, -248.6346026584197659, -318.0580252608186242 ) ) ;
#31606 = CARTESIAN_POINT ( 'NONE',  ( 265.7583438952258916, -600.0000000000000000, -320.0000000000000000 ) ) ;
#31607 = CARTESIAN_POINT ( 'NONE',  ( 778.1981804954714335, -130.2709662947837899, -314.8072714833589885 ) ) ;
#31608 = CARTESIAN_POINT ( 'NONE',  ( 800.0135310231082713, -254.0891481129652334, 325.0180583372163028 ) ) ;
#31609 = AXIS2_PLACEMENT_3D ( 'NONE', #33176, #8697, #37700 ) ;
#31610 = CARTESIAN_POINT ( 'NONE',  ( 754.9967657858570647, -385.5436935675102745, 365.0032342141425374 ) ) ;
#31611 = LINE ( 'NONE', #14289, #36602 ) ;
#31612 = CARTESIAN_POINT ( 'NONE',  ( 807.2620300519052989, -48.00906357242602951, -318.0141637701419768 ) ) ;
#31613 = CARTESIAN_POINT ( 'NONE',  ( 779.9999999999992042, 16.45630643248849267, 339.9999999999999432 ) ) ;
#31614 = CARTESIAN_POINT ( 'NONE',  ( 799.9999999999993179, 205.0000000000000568, 339.9999999999999432 ) ) ;
#31615 = CARTESIAN_POINT ( 'NONE',  ( 798.5707757039680246, -245.4636090269709143, 356.7845633553585003 ) ) ;
#31616 = CARTESIAN_POINT ( 'NONE',  ( 795.1360043628807261, -116.0891481129656029, 360.2193346964456282 ) ) ;
#31617 = EDGE_LOOP ( 'NONE', ( #41768, #27999, #14986, #35446 ) ) ;
#31618 = CARTESIAN_POINT ( 'NONE',  ( 786.5483106153019435, -7.645427208789786100, -364.1601925771022366 ) ) ;
#31619 = CARTESIAN_POINT ( 'NONE',  ( 810.7187646348534145, -114.4527844766020053, -356.7737145352016341 ) ) ;
#31620 = CARTESIAN_POINT ( 'NONE',  ( 796.7845633553578182, -297.6237781080502600, 358.5707757039688204 ) ) ;
#31621 = DIRECTION ( 'NONE',  ( -0.000000000000000000, 1.000000000000000000, -0.000000000000000000 ) ) ;
#31622 = CARTESIAN_POINT ( 'NONE',  ( 814.2805881961230625, -49.64542720878965554, 331.2368401574024119 ) ) ;
#31623 = CARTESIAN_POINT ( 'NONE',  ( 751.9810565676468741, -218.0891481129653187, -360.9747183278973921 ) ) ;
#31624 = CARTESIAN_POINT ( 'NONE',  ( 759.9864689768902508, -74.08914811296577341, 354.9819416627836404 ) ) ;
#31625 = CYLINDRICAL_SURFACE ( 'NONE', #31332, 7.999999999999896083 ) ;
#31626 = CARTESIAN_POINT ( 'NONE',  ( 746.7653713866222915, -257.2601417444141134, -351.0478386215610271 ) ) ;
#31627 = CARTESIAN_POINT ( 'NONE',  ( 784.1219089521767955, 2.718209154846545683, 315.0488828828318333 ) ) ;
#31628 = CARTESIAN_POINT ( 'NONE',  ( 804.7487373415286811, -331.5436935675104451, -364.7487373415288516 ) ) ;
#31629 = CARTESIAN_POINT ( 'NONE',  ( 701.1634899080286232, 256.4999999999999432, -197.2499999999991189 ) ) ;
#31630 = CARTESIAN_POINT ( 'NONE',  ( 775.9200461376533440, -359.8055962898683333, 315.3028492785443291 ) ) ;
#31631 = CARTESIAN_POINT ( 'NONE',  ( 800.9747183278959710, -36.99823902205679360, 311.9810565676471583 ) ) ;
#31632 = CARTESIAN_POINT ( 'NONE',  ( 758.0580252608178853, -390.4527844766011526, -328.0187753319985404 ) ) ;
#31633 = CARTESIAN_POINT ( 'NONE',  ( 763.2154366446407039, -45.62377810805114109, 321.4292242960311228 ) ) ;
#31634 = CARTESIAN_POINT ( 'NONE',  ( 744.9990715423526808, -66.35105083532378956, -341.2370466360926002 ) ) ;
#31635 = CARTESIAN_POINT ( 'NONE',  ( 766.7756240680305382, -206.5328690171415360, -361.5560724626415663 ) ) ;
#31636 = CARTESIAN_POINT ( 'NONE',  ( 801.9858362298568863, -195.0783235625961538, 312.7379699480935642 ) ) ;
#31637 = CARTESIAN_POINT ( 'NONE',  ( 804.6798772138710092, -15.72551174932958951, 334.6312213355106451 ) ) ;
#31638 = ORIENTED_EDGE ( 'NONE', *, *, #35350, .T. ) ;
#31639 = CARTESIAN_POINT ( 'NONE',  ( 773.3843516231979720, -205.4419599262324425, -364.4086373105754433 ) ) ;
#31640 = CARTESIAN_POINT ( 'NONE',  ( 803.6646147819161570, -209.9073299311470748, 348.8264449731210561 ) ) ;
#31641 = CARTESIAN_POINT ( 'NONE',  ( 768.8385539511368734, -23.26014174441484883, -306.4236121716840557 ) ) ;
#31642 = CARTESIAN_POINT ( 'NONE',  ( 771.2633955100217236, -311.9073299311468759, 363.4237431249939618 ) ) ;
#31643 = DIRECTION ( 'NONE',  ( 0.000000000000000000, 0.000000000000000000, -1.000000000000000000 ) ) ;
#31644 = EDGE_LOOP ( 'NONE', ( #14694, #18823, #44062, #33631 ) ) ;
#31645 = CARTESIAN_POINT ( 'NONE',  ( 803.2186876482843445, -55.98741447168748664, 350.0220218866286928 ) ) ;
#31646 = CARTESIAN_POINT ( 'NONE',  ( 746.4236121716829757, -303.8272453906071178, -328.8385539511384650 ) ) ;
#31647 = CARTESIAN_POINT ( 'NONE',  ( 808.0189434323515343, -254.0891481129652334, 319.0252816721025511 ) ) ;
#31648 = CARTESIAN_POINT ( 'NONE',  ( 744.8212110874229666, 5.103494619221427442, 336.2046728542121627 ) ) ;
#31649 = CARTESIAN_POINT ( 'NONE',  ( 772.4468031744293057, -153.8272453906075157, -363.8651313633793620 ) ) ;
#31650 = CARTESIAN_POINT ( 'NONE',  ( 800.0135310231082713, -158.0891481129655176, -325.0180583372163028 ) ) ;
#31651 = CARTESIAN_POINT ( 'NONE',  ( 788.8264449731201466, -333.1800572038740142, -363.6646147819170665 ) ) ;
#31652 = ORIENTED_EDGE ( 'NONE', *, *, #2160, .T. ) ;
#31653 = CARTESIAN_POINT ( 'NONE',  ( 804.4286716492782716, -449.3618753856918602, -345.3141322388244703 ) ) ;
#31654 = CARTESIAN_POINT ( 'NONE',  ( 810.7187646348534145, -306.4527844766013800, 356.7737145352016341 ) ) ;
#31655 = LINE ( 'NONE', #3497, #32920 ) ;
#31656 = CARTESIAN_POINT ( 'NONE',  ( 789.9200121543843807, -337.9874144716865771, 317.0176451133914384 ) ) ;
#31657 = CARTESIAN_POINT ( 'NONE',  ( 831.1634899080286232, 239.9999999999999147, -199.9999999999999432 ) ) ;
#31658 = CARTESIAN_POINT ( 'NONE',  ( 790.0220218866281812, -151.0999726633347677, 363.2186876482849129 ) ) ;
#31659 = CARTESIAN_POINT ( 'NONE',  ( 804.9363028652555840, -16.27096629478413092, 338.2165204200192079 ) ) ;
#31660 = EDGE_LOOP ( 'NONE', ( #13925, #18996 ) ) ;
#31661 = CARTESIAN_POINT ( 'NONE',  ( 791.0478386215596629, -381.8272453906068336, -306.7653713866226326 ) ) ;
#31662 = FACE_OUTER_BOUND ( 'NONE', #24888, .T. ) ;
#31663 = CARTESIAN_POINT ( 'NONE',  ( 752.7379699480933368, -252.0090635724254184, 361.9858362298580232 ) ) ;
#31664 = CARTESIAN_POINT ( 'NONE',  ( 784.0799538623451781, -179.8055962898688733, 364.6971507214555572 ) ) ;
#31665 = CARTESIAN_POINT ( 'NONE',  ( 771.1735550268778070, -369.1800572038739574, -316.3353852180827630 ) ) ;
#31666 = DIRECTION ( 'NONE',  ( -0.000000000000000000, 1.000000000000000000, -0.000000000000000000 ) ) ;
#31667 = CARTESIAN_POINT ( 'NONE',  ( 793.0897708529556667, -222.5545181178800362, -361.3366627262616362 ) ) ;
#31668 = CARTESIAN_POINT ( 'NONE',  ( 811.0346526505616112, -14.63460265842049424, 323.0537975583477532 ) ) ;
#31669 = CARTESIAN_POINT ( 'NONE',  ( 809.6099558218720631, -452.9681489794449476, 335.1781210895659342 ) ) ;
#31670 = CARTESIAN_POINT ( 'NONE',  ( 801.1904061080338124, -404.0891481129646650, -368.3070685750236066 ) ) ;
#31671 = DIRECTION ( 'NONE',  ( 0.000000000000000000, 0.000000000000000000, -1.000000000000000000 ) ) ;
#31672 = CARTESIAN_POINT ( 'NONE',  ( 814.4686193811664907, -363.2817908451523294, 346.2056067578752732 ) ) ;
#31673 = PLANE ( 'NONE',  #28683 ) ;
#31674 = CARTESIAN_POINT ( 'NONE',  ( 812.7932403749906598, -327.1800572038741279, 327.7687537140311633 ) ) ;
#31675 = CARTESIAN_POINT ( 'NONE',  ( 782.4968714119720516, -58.81642084023854267, -305.0891759886411023 ) ) ;
#31676 = EDGE_CURVE ( 'NONE', #17002, #28334, #25943, .T. ) ;
#31677 = CARTESIAN_POINT ( 'NONE',  ( 804.9363028652555840, -280.2709662947833067, -338.2165204200192079 ) ) ;
#31678 = FACE_BOUND ( 'NONE', #9946, .T. ) ;
#31679 = CARTESIAN_POINT ( 'NONE',  ( 765.0180583372156207, -384.9982390220556567, 360.0135310231089534 ) ) ;
#31680 = CARTESIAN_POINT ( 'NONE',  ( 804.4086373105744769, -145.6454272087893287, 333.3843516231986541 ) ) ;
#31681 = CARTESIAN_POINT ( 'NONE',  ( 752.7379699480933368, -36.00906357242605793, -361.9858362298580232 ) ) ;
#31682 = CARTESIAN_POINT ( 'NONE',  ( 804.9511171171677688, -101.8055962898691718, -335.8780910478229202 ) ) ;
#31683 = CARTESIAN_POINT ( 'NONE',  ( 754.0944755984390895, -87.62377810805102740, 364.1009440267246760 ) ) ;
#31684 = CARTESIAN_POINT ( 'NONE',  ( 781.7834795799800531, -394.8164208402374697, 315.0636971347436202 ) ) ;
#31685 = CARTESIAN_POINT ( 'NONE',  ( 808.3070685750232087, 5.001760977943074948, 361.1904061080339829 ) ) ;
#31686 = LINE ( 'NONE', #18694, #32179 ) ;
#31687 = CARTESIAN_POINT ( 'NONE',  ( 767.8955696845333705, -0.4527844766023628176, -362.1676090361162323 ) ) ;
#31689 = ORIENTED_EDGE ( 'NONE', *, *, #37580, .F. ) ;
#31688 = CARTESIAN_POINT ( 'NONE',  ( 776.9566956441375396, -108.8965053807782084, -364.8461984189686405 ) ) ;
#31690 = CARTESIAN_POINT ( 'NONE',  ( 785.3687786644884454, -107.3618753856928976, -315.3201227861279676 ) ) ;
#31691 = CARTESIAN_POINT ( 'NONE',  ( 796.7845633553578182, -393.6237781080500326, -358.5707757039688204 ) ) ;
#31693 = CARTESIAN_POINT ( 'NONE',  ( 768.0187753319979720, -224.6346026584198228, 318.0580252608186242 ) ) ;
#31692 = CARTESIAN_POINT ( 'NONE',  ( 788.8264449731200330, -237.1800572038742985, 363.6646147819171233 ) ) ;
#31694 = CARTESIAN_POINT ( 'NONE',  ( 800.1688906516307043, -394.1692326535045368, -369.0717654672308186 ) ) ;
#31695 = CARTESIAN_POINT ( 'NONE',  ( 777.5031285880264704, 1.183579159761269040, 374.9108240113588408 ) ) ;
#31696 = FACE_OUTER_BOUND ( 'NONE', #19096, .T. ) ;
#31697 = ORIENTED_EDGE ( 'NONE', *, *, #27219, .F. ) ;
#31698 = CARTESIAN_POINT ( 'NONE',  ( 792.1044303154645831, -444.4527844766009821, 317.8323909638837677 ) ) ;
#31699 = ORIENTED_EDGE ( 'NONE', *, *, #6400, .T. ) ;
#31700 = CARTESIAN_POINT ( 'NONE',  ( 782.4968714119720516, -250.8164208402379245, -305.0891759886411023 ) ) ;
#31701 = CARTESIAN_POINT ( 'NONE',  ( 792.3570229623691148, -141.1800572038746395, 373.1304606946836770 ) ) ;
#31702 = ORIENTED_EDGE ( 'NONE', *, *, #31535, .F. ) ;
#31703 = CARTESIAN_POINT ( 'NONE',  ( 747.3154664389472828, -187.9874144716870603, 326.4474001241230781 ) ) ;
#31704 = CARTESIAN_POINT ( 'NONE',  ( 756.5762568750052424, -243.1800572038743269, -348.7366044899774238 ) ) ;
#31705 = VERTEX_POINT ( 'NONE', #40290 ) ;
#31706 = CARTESIAN_POINT ( 'NONE',  ( 801.9419747391806368, -354.4527844766012095, -351.9812246680014027 ) ) ;
#31707 = CARTESIAN_POINT ( 'NONE',  ( 781.8018195045266339, -22.27096629478410250, -365.1927285166406705 ) ) ;
#31708 = CARTESIAN_POINT ( 'NONE',  ( 757.2208543904082489, -232.7146871989596377, 350.9844846989624330 ) ) ;
#31709 = DIRECTION ( 'NONE',  ( 0.000000000000000000, 0.000000000000000000, 1.000000000000000000 ) ) ;
#31710 = LINE ( 'NONE', #32640, #28750 ) ;
#31711 = ORIENTED_EDGE ( 'NONE', *, *, #11972, .F. ) ;
#31712 = CARTESIAN_POINT ( 'NONE',  ( 771.1735550268778070, -33.18005720387498769, -316.3353852180827630 ) ) ;
#31713 = DIRECTION ( 'NONE',  ( 0.000000000000000000, 0.000000000000000000, 1.000000000000000000 ) ) ;
#31714 = DIRECTION ( 'NONE',  ( 1.000000000000000000, 0.000000000000000000, 0.000000000000000000 ) ) ;
#31715 = ORIENTED_EDGE ( 'NONE', *, *, #34881, .T. ) ;
#31716 = CARTESIAN_POINT ( 'NONE',  ( 752.7379699480933368, -276.0090635724253048, -361.9858362298580232 ) ) ;
#31717 = CARTESIAN_POINT ( 'NONE',  ( 755.8990559732751535, -131.4636090269711985, 365.9055244015606831 ) ) ;
#31719 = CARTESIAN_POINT ( 'NONE',  ( 801.9419747391806368, -210.4527844766016926, -351.9812246680014027 ) ) ;
#31718 = DIRECTION ( 'NONE',  ( 0.000000000000000000, 1.000000000000000000, 0.000000000000000000 ) ) ;
#31720 = CARTESIAN_POINT ( 'NONE',  ( 756.7813123517142913, -403.9874144716863498, -329.9779781133712504 ) ) ;
#31721 = DIRECTION ( 'NONE',  ( -1.000000000000000000, -0.000000000000000000, 0.000000000000000000 ) ) ;
#31722 = CARTESIAN_POINT ( 'NONE',  ( 769.9779781133707957, -115.0999726633348956, -316.7813123517150871 ) ) ;
#31723 = EDGE_CURVE ( 'NONE', #25938, #15578, #12333, .T. ) ;
#31724 = CARTESIAN_POINT ( 'NONE',  ( 764.1737431748507561, -370.3726999360613377, 371.6461892240376415 ) ) ;
#31725 = CARTESIAN_POINT ( 'NONE',  ( 911.9999999999994316, 154.9999999999998863, -360.0000000000000000 ) ) ;
#31726 = CARTESIAN_POINT ( 'NONE',  ( 748.3538107759620743, 7.285312801039605546, -355.8262568251490165 ) ) ;
#31727 = CARTESIAN_POINT ( 'NONE',  ( 751.6929314249750860, -318.9982390220558841, -318.8095938919659034 ) ) ;
#31728 = CARTESIAN_POINT ( 'NONE',  ( 768.0187753319979720, -8.634602658420517329, 318.0580252608186242 ) ) ;
#31729 = CARTESIAN_POINT ( 'NONE',  ( 767.8955696845333705, -72.45278447660213317, -362.1676090361162323 ) ) ;
#31730 = CARTESIAN_POINT ( 'NONE',  ( 781.2370466360911223, -260.7363362996981095, 304.9990715423533629 ) ) ;
#31731 = CARTESIAN_POINT ( 'NONE',  ( 811.6461892240364477, -196.7146871989598083, -324.1737431748509835 ) ) ;
#31732 = CARTESIAN_POINT ( 'NONE',  ( 811.0346526505616112, -230.6346026584197659, 323.0537975583477532 ) ) ;
#31733 = CARTESIAN_POINT ( 'NONE',  ( 766.4474001241216001, 4.900027336664720679, -307.3154664389482491 ) ) ;
#31734 = EDGE_CURVE ( 'NONE', #41282, #5516, #8408, .T. ) ;
#31735 = DIRECTION ( 'NONE',  ( 0.000000000000000000, 0.000000000000000000, 1.000000000000000000 ) ) ;
#31736 = CARTESIAN_POINT ( 'NONE',  ( 781.7834795799800531, -298.8164208402377540, 315.0636971347436202 ) ) ;
#31737 = CARTESIAN_POINT ( 'NONE',  ( 763.0428371773158460, -83.46360902697136908, 358.7617431975195359 ) ) ;
#31738 = CARTESIAN_POINT ( 'NONE',  ( 792.1044303154645831, -444.4527844766009821, -317.8323909638837677 ) ) ;
#31739 = CARTESIAN_POINT ( 'NONE',  ( 999.9999999999992042, -590.0000000000001137, 350.0000000000000000 ) ) ;
#31740 = CARTESIAN_POINT ( 'NONE',  ( 701.1634899080286232, 259.9999999999999432, -199.9999999999990337 ) ) ;
#31742 = CARTESIAN_POINT ( 'NONE',  ( 774.6858677611749044, -345.7255117493285184, 315.5713283507209894 ) ) ;
#31741 = CARTESIAN_POINT ( 'NONE',  ( 786.6156483768007774, -121.4419599262327267, 315.5913626894246136 ) ) ;
#31743 = EDGE_LOOP ( 'NONE', ( #32853, #20834, #1086, #37656 ) ) ;
#31744 = CARTESIAN_POINT ( 'NONE',  ( 773.3843516231979720, -301.4419599262320730, -364.4086373105754433 ) ) ;
#31745 = CARTESIAN_POINT ( 'NONE',  ( 804.9363028652555840, -88.27096629478390355, 338.2165204200192079 ) ) ;
#31746 = CARTESIAN_POINT ( 'NONE',  ( 744.8212110874229666, -282.8965053807776258, -336.2046728542121627 ) ) ;
#31747 = CYLINDRICAL_SURFACE ( 'NONE', #35205, 2.749999999999863665 ) ;
#31748 = CARTESIAN_POINT ( 'NONE',  ( 749.8865473780648472, -404.5328690171409107, 322.1177392798429082 ) ) ;
#31749 = EDGE_CURVE ( 'NONE', #43930, #11422, #22476, .T. ) ;
#31750 = ORIENTED_EDGE ( 'NONE', *, *, #34286, .T. ) ;
#31751 = CARTESIAN_POINT ( 'NONE',  ( 762.3223304703356007, -319.5436935675104451, 322.3223304703362828 ) ) ;
#31752 = EDGE_CURVE ( 'NONE', #19936, #24078, #32902, .T. ) ;
#31753 = CARTESIAN_POINT ( 'NONE',  ( 802.7791456095903868, -52.71468719896020616, -329.0155153010375102 ) ) ;
#31754 = CARTESIAN_POINT ( 'NONE',  ( 758.0580252608178853, -174.4527844766018063, -328.0187753319985404 ) ) ;
#31755 = CARTESIAN_POINT ( 'NONE',  ( 756.5762568750052424, -195.1800572038744974, -348.7366044899774238 ) ) ;
#31756 = CARTESIAN_POINT ( 'NONE',  ( 778.1981804954714335, -418.2709662947827383, 314.8072714833589885 ) ) ;
#31757 = CARTESIAN_POINT ( 'NONE',  ( 751.6929314249748586, -150.9982390220563957, -318.8095938919659034 ) ) ;
#31758 = EDGE_CURVE ( 'NONE', #22719, #16202, #44181, .T. ) ;
#31759 = CARTESIAN_POINT ( 'NONE',  ( 804.9363028652555840, -136.2709662947837330, -338.2165204200192079 ) ) ;
#31760 = ORIENTED_EDGE ( 'NONE', *, *, #202, .F. ) ;
#31761 = CARTESIAN_POINT ( 'NONE',  ( 805.2837595273609850, -386.7363362996977116, -340.5290396650784714 ) ) ;
#31763 = CARTESIAN_POINT ( 'NONE',  ( 773.4516893846965786, -427.6454272087885897, 315.8398074228977066 ) ) ;
#31762 = CARTESIAN_POINT ( 'NONE',  ( 778.1981804954714335, -130.2709662947837899, 314.8072714833589885 ) ) ;
#31764 = CARTESIAN_POINT ( 'NONE',  ( 798.7617431975189675, -123.6237781080508569, 323.0428371773161871 ) ) ;
#31767 = CARTESIAN_POINT ( 'NONE',  ( 776.2433038121456548, -396.8965053807772847, 374.8207195650711014 ) ) ;
#31766 = CYLINDRICAL_SURFACE ( 'NONE', #18132, 10.00000000000000888 ) ;
#31765 = CARTESIAN_POINT ( 'NONE',  ( 779.9999999999992042, -462.9681489794448339, 339.9999999999999432 ) ) ;
#31768 = ORIENTED_EDGE ( 'NONE', *, *, #12563, .F. ) ;
#31769 = CARTESIAN_POINT ( 'NONE',  ( 802.9823548866075953, -385.0999726633340856, -330.0799878456151077 ) ) ;
#31770 = CARTESIAN_POINT ( 'NONE',  ( 804.6798772138708955, -351.7255117493284047, -334.6312213355107019 ) ) ;
#31771 = CARTESIAN_POINT ( 'NONE',  ( 746.4236121716829757, -159.8272453906075157, -328.8385539511384650 ) ) ;
#31772 = CARTESIAN_POINT ( 'NONE',  ( 811.3240766477731540, -28.37269993606244967, 355.6651683502462902 ) ) ;
#31774 = DIRECTION ( 'NONE',  ( -1.000000000000000000, -0.000000000000000000, -0.000000000000000000 ) ) ;
#31773 = CYLINDRICAL_SURFACE ( 'NONE', #7934, 1.000000000000000888 ) ;
#31775 = ADVANCED_FACE ( 'NONE', ( #1463 ), #33332, .T. ) ;
#31776 = CARTESIAN_POINT ( 'NONE',  ( 783.0433043558608688, -288.8965053807775121, -315.1538015810313027 ) ) ;
#31777 = CARTESIAN_POINT ( 'NONE',  ( 805.1927285166397041, -448.8164208402371855, -341.8018195045277707 ) ) ;
#31778 = CARTESIAN_POINT ( 'NONE',  ( 812.3518521366052028, -169.0999726633347393, -326.5853460496235243 ) ) ;
#31779 = DIRECTION ( 'NONE',  ( -1.880165489482579047E-16, -1.000000000000000000, -0.000000000000000000 ) ) ;
#31780 = DIRECTION ( 'NONE',  ( 8.326672684688676025E-16, -1.000000000000000000, 0.000000000000000000 ) ) ;
#31781 = CARTESIAN_POINT ( 'NONE',  ( 801.5560724626406000, -360.5545181178796383, 326.7756240680316182 ) ) ;
#31782 = EDGE_CURVE ( 'NONE', #40120, #4703, #22925, .T. ) ;
#31783 = CARTESIAN_POINT ( 'NONE',  ( 757.7880784355613741, -330.0090635724251342, 312.4576283171834916 ) ) ;
#31784 = CARTESIAN_POINT ( 'NONE',  ( 747.2067596250078623, -195.1800572038744974, -352.2312462859687230 ) ) ;
#31785 = DIRECTION ( 'NONE',  ( 1.000000000000000000, 0.000000000000000000, 0.000000000000000000 ) ) ;
#31786 = CARTESIAN_POINT ( 'NONE',  ( 784.4999999999993179, -365.3551492539851893, -18.13243251470705886 ) ) ;
#31787 = CARTESIAN_POINT ( 'NONE',  ( 746.4236121716829757, -135.8272453906076009, 328.8385539511384650 ) ) ;
#31788 = CARTESIAN_POINT ( 'NONE',  ( 758.0141637701419768, -111.0783235625964096, -367.2620300519063790 ) ) ;
#31789 = CARTESIAN_POINT ( 'NONE',  ( 808.3070685750230950, -90.99823902205663728, 361.1904061080339261 ) ) ;
#31790 = CARTESIAN_POINT ( 'NONE',  ( 814.9108240113580450, -328.2709662947831362, -337.5031285880265273 ) ) ;
#31791 = CARTESIAN_POINT ( 'NONE',  ( -858.8365100919713768, 258.0940000000002215, -199.9999999999881481 ) ) ;
#31792 = PRODUCT ( 'Heavy Cast Iron Table Bed Base', 'Heavy Cast Iron Table Bed Base', '', ( #3663 ) ) ;
#31793 = CARTESIAN_POINT ( 'NONE',  ( -26.63011601220122060, -512.9681489794448908, -339.9999999999999432 ) ) ;
#31794 = CARTESIAN_POINT ( 'NONE',  ( 764.8639956371174549, -200.0891481129653187, 319.7806653035542013 ) ) ;
#31795 = CARTESIAN_POINT ( 'NONE',  ( 794.5607502887775127, -462.9631818684622999, 371.8524697363486666 ) ) ;
#31796 = CARTESIAN_POINT ( 'NONE',  ( 781.2497674668890113, -396.3510508353228374, -375.3608509340180603 ) ) ;
#31797 = CARTESIAN_POINT ( 'NONE',  ( 772.4837098697144029, -407.3618753856920307, -374.5518280994205611 ) ) ;
#31798 = CARTESIAN_POINT ( 'NONE',  ( 999.9999999999992042, 249.9999999999998863, 360.0000000000000000 ) ) ;
#31799 = CARTESIAN_POINT ( 'NONE',  ( 746.0683387631852383, 4.558040073766884248, 331.3260364891676204 ) ) ;
#31800 = VERTEX_POINT ( 'NONE', #33560 ) ;
#31801 = AXIS2_PLACEMENT_3D ( 'NONE', #33990, #33775, #29852 ) ;
#31802 = CARTESIAN_POINT ( 'NONE',  ( 791.1614460488616487, -179.2601417444143692, -373.5763878283158874 ) ) ;
#31803 = DIRECTION ( 'NONE',  ( 0.000000000000000000, 0.000000000000000000, -1.000000000000000000 ) ) ;
#31804 = CARTESIAN_POINT ( 'NONE',  ( 795.6651683502461765, -322.7146871989593819, 371.3240766477733814 ) ) ;
#31805 = CARTESIAN_POINT ( 'NONE',  ( 778.1981804954715471, -106.2709662947838467, 314.8072714833591021 ) ) ;
#31806 = ORIENTED_EDGE ( 'NONE', *, *, #39951, .F. ) ;
#31807 = CARTESIAN_POINT ( 'NONE',  ( 762.1405469898971887, -145.5436935675109851, -357.8594530101015607 ) ) ;
#31808 = CARTESIAN_POINT ( 'NONE',  ( 768.0187753319979720, -296.6346026584195670, 318.0580252608186242 ) ) ;
#31809 = CARTESIAN_POINT ( 'NONE',  ( 787.5162901302840055, -59.36187538569306810, -305.4481719005792684 ) ) ;
#31810 = CARTESIAN_POINT ( 'NONE',  ( 787.4397851343537695, -93.72551174932934259, 374.2001403089903988 ) ) ;
#31811 = VERTEX_POINT ( 'NONE', #27096 ) ;
#31812 = CARTESIAN_POINT ( 'NONE',  ( 809.0717654672305343, -436.9181544815157281, -360.1688906516309885 ) ) ;
#31813 = VERTEX_POINT ( 'NONE', #23384 ) ;
#31814 = APPLICATION_PROTOCOL_DEFINITION ( 'draft international standard', 'automotive_design', 1998, #11927 ) ;
#31815 = CARTESIAN_POINT ( 'NONE',  ( 803.6646147819161570, -17.90732993114776406, 348.8264449731210561 ) ) ;
#31816 = CARTESIAN_POINT ( 'NONE',  ( 771.2633955100217236, -287.9073299311468759, -363.4237431249939618 ) ) ;
#31818 = CARTESIAN_POINT ( 'NONE',  ( 744.9990715423526808, -282.3510508353230080, 341.2370466360926002 ) ) ;
#31817 = CARTESIAN_POINT ( 'NONE',  ( 800.9747183278959710, -372.9982390220557704, 311.9810565676471583 ) ) ;
#31819 = CARTESIAN_POINT ( 'NONE',  ( 773.7943932421234194, -71.80559628986922860, 305.5313806188329409 ) ) ;
#31820 = CARTESIAN_POINT ( 'NONE',  ( 796.9571628226829034, -263.4636090269708006, -321.2382568024804641 ) ) ;
#31821 = CARTESIAN_POINT ( 'NONE',  ( 781.7834795799800531, -250.8164208402379245, -315.0636971347436202 ) ) ;
#31822 = CARTESIAN_POINT ( 'NONE',  ( 797.8594530101009923, -445.5436935675099335, -322.1405469898982119 ) ) ;
#31823 = CARTESIAN_POINT ( 'NONE',  ( 804.6798772138708955, -111.7255117493293000, -334.6312213355107019 ) ) ;
#31824 = CARTESIAN_POINT ( 'NONE',  ( 773.4999999999993179, -365.3551492539851893, -18.13243251470705886 ) ) ;
#31825 = CARTESIAN_POINT ( 'NONE',  ( 745.4481719005789273, -387.7255117493283478, 347.5162901302853129 ) ) ;
#31826 =( BOUNDED_CURVE ( )  B_SPLINE_CURVE ( 2, ( #44044, #20016, #1762, #22799, #34093, #5033, #9629 ),
 .UNSPECIFIED., .F., .T. ) 
 B_SPLINE_CURVE_WITH_KNOTS ( ( 3, 2, 2, 3 ),
 ( 0.006081874955971018626, 0.006818181818181817851, 0.009090909090909090468, 0.01033270150184909669 ),
 .UNSPECIFIED. ) 
 CURVE ( )  GEOMETRIC_REPRESENTATION_ITEM ( )  RATIONAL_B_SPLINE_CURVE ( ( 0.4977709609702910543, 0.4983514209501199721, 0.5000002209606653203, 0.4949109396520706694, 0.5000002209606653203, 0.4972194953619585855, 0.4974774836351868457 ) ) 
 REPRESENTATION_ITEM ( '' )  );
#31828 = DIRECTION ( 'NONE',  ( -1.058954862565134068E-16, 0.6438296778008191223, 0.7651688349527137056 ) ) ;
#31827 = CARTESIAN_POINT ( 'NONE',  ( 799.9999999999993179, -462.9681489794448339, -370.0000000000000568 ) ) ;
#31829 = CARTESIAN_POINT ( 'NONE',  ( 746.4236121716829757, -63.82724539060779279, -328.8385539511384650 ) ) ;
#31830 = DIRECTION ( 'NONE',  ( 0.000000000000000000, 0.3826834323650836756, 0.9238795325112892920 ) ) ;
#31831 = LINE ( 'NONE', #7142, #178 ) ;
#31832 = CARTESIAN_POINT ( 'NONE',  ( 773.4516893846965786, -259.6454272087890445, 315.8398074228977066 ) ) ;
#31833 = CARTESIAN_POINT ( 'NONE',  ( 804.4286716492782716, -113.3618753856929260, 345.3141322388244703 ) ) ;
#31834 = ORIENTED_EDGE ( 'NONE', *, *, #24906, .T. ) ;
#31835 = CARTESIAN_POINT ( 'NONE',  ( 790.0220218866281812, -7.099972663335241130, -363.2186876482849129 ) ) ;
#31836 = VECTOR ( 'NONE', #45551, 1000.000000000000000 ) ;
#31837 = CARTESIAN_POINT ( 'NONE',  ( 782.4968714119720516, -106.8164208402383935, -305.0891759886411023 ) ) ;
#31838 = CARTESIAN_POINT ( 'NONE',  ( 772.3691319403857278, -287.2601417444140566, 315.8894580844506663 ) ) ;
#31839 = CARTESIAN_POINT ( 'NONE',  ( 779.9999999999992042, -462.9681489794448339, -339.9999999999999432 ) ) ;
#31840 = CARTESIAN_POINT ( 'NONE',  ( 814.8207195650702488, -50.19088175424420939, 336.2433038121456548 ) ) ;
#31841 = CARTESIAN_POINT ( 'NONE',  ( 755.2512626584698410, -223.5436935675107577, -315.2512626584710915 ) ) ;
#31842 = CARTESIAN_POINT ( 'NONE',  ( 758.8095938919642549, -176.0891481129653755, 311.6929314249763365 ) ) ;
#31843 = CARTESIAN_POINT ( 'NONE',  ( 754.8072714833581358, -76.81642084023845030, 338.1981804954720587 ) ) ;
#31844 = CARTESIAN_POINT ( 'NONE',  ( 749.8865473780648472, -284.5328690171412518, -322.1177392798429082 ) ) ;
#31845 = CARTESIAN_POINT ( 'NONE',  ( 805.6418435158337843, -437.4636090269703459, 363.8556311672236916 ) ) ;
#31846 = CARTESIAN_POINT ( 'NONE',  ( 777.5031285880264704, -310.8164208402377540, -374.9108240113588408 ) ) ;
#31847 = CARTESIAN_POINT ( 'NONE',  ( 794.9999999999993179, 205.0000000000000568, -235.0000000000000284 ) ) ;
#31848 = CARTESIAN_POINT ( 'NONE',  ( 773.3843516231979720, -373.4419599262319593, 364.4086373105754433 ) ) ;
#31849 = CARTESIAN_POINT ( 'NONE',  ( 815.2698199232962679, -40.81642084023859951, 342.5225473063383674 ) ) ;
#31850 = CARTESIAN_POINT ( 'NONE',  ( 794.9819416627830151, -396.9982390220556567, -319.9864689768909898 ) ) ;
#31851 = CARTESIAN_POINT ( 'NONE',  ( 787.6308680596127942, -59.26014174441473870, 364.1105419155492768 ) ) ;
#31852 = CARTESIAN_POINT ( 'NONE',  ( 794.9819416627830151, -204.9982390220562820, -319.9864689768909898 ) ) ;
#31853 = CARTESIAN_POINT ( 'NONE',  ( 814.8230680027162407, -77.80559628986920018, -333.7305795820267917 ) ) ;
#31854 = CARTESIAN_POINT ( 'NONE',  ( 764.3348316497523456, -190.7146871989597798, 308.6759233522265617 ) ) ;
#31855 = CARTESIAN_POINT ( 'NONE',  ( 755.0636971347428243, -28.27096629478409540, 341.7834795799807353 ) ) ;
#31856 = ORIENTED_EDGE ( 'NONE', *, *, #960, .F. ) ;
#31857 = CARTESIAN_POINT ( 'NONE',  ( 788.7366044899766848, -83.90732993114754379, -316.5762568750059813 ) ) ;
#31858 = CARTESIAN_POINT ( 'NONE',  ( 769.1273215169530886, -214.7146871989597230, -317.4527132478988847 ) ) ;
#31859 = CARTESIAN_POINT ( 'NONE',  ( 795.1360043628807261, -212.0891481129652902, 360.2193346964456282 ) ) ;
#31860 = CARTESIAN_POINT ( 'NONE',  ( 748.3538107759620743, -40.71468719896024879, -355.8262568251490165 ) ) ;
#31861 = CARTESIAN_POINT ( 'NONE',  ( 759.9864689768902508, -338.0891481129649492, 354.9819416627836404 ) ) ;
#31862 = VECTOR ( 'NONE', #12134, 1000.000000000000114 ) ;
#31863 = DIRECTION ( 'NONE',  ( 0.000000000000000000, 0.000000000000000000, 1.000000000000000000 ) ) ;
#31864 = ORIENTED_EDGE ( 'NONE', *, *, #1019, .F. ) ;
#31865 = CARTESIAN_POINT ( 'NONE',  ( 805.0264073115434940, -54.35105083532383219, 339.4763451958999099 ) ) ;
#31866 = CARTESIAN_POINT ( 'NONE',  ( 778.7629533639073998, -320.7363362996979390, -375.0009284576466371 ) ) ;
#31867 = CARTESIAN_POINT ( 'NONE',  ( 763.0537975583476964, -264.4527844766016074, 371.0346526505628617 ) ) ;
#31868 = MANIFOLD_SOLID_BREP ( 'Cut-Extrude5[2]', #29128 ) ;
#31869 = CARTESIAN_POINT ( 'NONE',  ( 815.0009284576459549, 17.64894916467593688, 338.7629533639073429 ) ) ;
#31870 = CARTESIAN_POINT ( 'NONE',  ( 757.4527132478984868, -136.3726999360621051, -329.1273215169538844 ) ) ;
#31871 = CARTESIAN_POINT ( 'NONE',  ( 778.1981804954714335, -154.2709662947836478, -314.8072714833589885 ) ) ;
#31872 = CARTESIAN_POINT ( 'NONE',  ( 757.8323909638828582, -338.6346026584195101, -352.1044303154654358 ) ) ;
#31873 = ORIENTED_EDGE ( 'NONE', *, *, #18116, .F. ) ;
#31874 = CARTESIAN_POINT ( 'NONE',  ( 767.7687537140311633, -287.9073299311468759, 372.7932403749916830 ) ) ;
#31875 = CARTESIAN_POINT ( 'NONE',  ( 181.1634899080285948, 260.0000000000000000, -199.9999999999953957 ) ) ;
#31876 = CARTESIAN_POINT ( 'NONE',  ( 783.0433043558608688, -336.8965053807774552, 315.1538015810313027 ) ) ;
#31877 = LINE ( 'NONE', #24, #17483 ) ;
#31878 = CARTESIAN_POINT ( 'NONE',  ( 787.5531968255692163, -165.8272453906074873, 316.1348686366205811 ) ) ;
#31879 = CARTESIAN_POINT ( 'NONE',  ( 774.6312213355099630, -23.36187538569318889, 364.6798772138717482 ) ) ;
#31880 = ORIENTED_EDGE ( 'NONE', *, *, #169, .T. ) ;
#31881 = CARTESIAN_POINT ( 'NONE',  ( 745.7194118038753459, -373.6454272087887034, -348.7631598425976449 ) ) ;
#31882 = VECTOR ( 'NONE', #19339, 1000.000000000000000 ) ;
#31883 = EDGE_CURVE ( 'NONE', #16263, #30441, #44879, .T. ) ;
#31884 = CARTESIAN_POINT ( 'NONE',  ( 787.5162901302840055, 12.63812461430668677, -305.4481719005793252 ) ) ;
#31885 = CARTESIAN_POINT ( 'NONE',  ( 744.6391490659812007, -230.7363362996981664, 338.7502325331110455 ) ) ;
#31886 = CARTESIAN_POINT ( 'NONE',  ( 803.2186876482843445, -199.9874144716870603, 350.0220218866286928 ) ) ;
#31887 = CARTESIAN_POINT ( 'NONE',  ( 755.5713283507202505, -365.3618753856920875, -334.6858677611754729 ) ) ;
#31888 = CARTESIAN_POINT ( 'NONE',  ( 785.3687786644884454, 12.63812461430668321, 315.3201227861279676 ) ) ;
#31889 = CARTESIAN_POINT ( 'NONE',  ( 754.7162404726377645, -206.7363362996982801, -339.4709603349214717 ) ) ;
#31890 = CARTESIAN_POINT ( 'NONE',  ( 763.2262854647970016, -8.634602658420517329, 309.2812353651462445 ) ) ;
#31891 = CARTESIAN_POINT ( 'NONE',  ( 767.6429770376289525, -81.18005720387481006, 306.8695393053162093 ) ) ;
#31892 = AXIS2_PLACEMENT_3D ( 'NONE', #45611, #7024, #21113 ) ;
#31893 = CARTESIAN_POINT ( 'NONE',  ( 772.4999999999993179, -512.9681489794448908, 339.9999999999999432 ) ) ;
#31894 = CARTESIAN_POINT ( 'NONE',  ( 800.9747183278959710, -420.9982390220555999, -311.9810565676471583 ) ) ;
#31895 = CARTESIAN_POINT ( 'NONE',  ( -78.83651009197140525, 258.0940000000000509, -199.9999999999936051 ) ) ;
#31896 = CARTESIAN_POINT ( 'NONE',  ( 786.2694204179717872, -357.2817908451523294, 305.1769319972829067 ) ) ;
#31897 = CARTESIAN_POINT ( 'NONE',  ( 806.6271908675616942, -455.4127378225107350, -353.8200110890837777 ) ) ;
#31898 = CARTESIAN_POINT ( 'NONE',  ( 782.5225473063381969, -334.2709662947829656, 375.2698199232970637 ) ) ;
#31899 = CARTESIAN_POINT ( 'NONE',  ( 792.2312462859673587, -59.90732993114762905, -307.2067596250082602 ) ) ;
#31900 = CARTESIAN_POINT ( 'NONE',  ( 804.6798772138708955, -279.7255117493288026, -334.6312213355107019 ) ) ;
#31901 = DIRECTION ( 'NONE',  ( -1.000000000000000000, -0.000000000000000000, 0.000000000000000000 ) ) ;
#31902 = CARTESIAN_POINT ( 'NONE',  ( 767.8955696845333705, -432.4527844766008684, 362.1676090361162323 ) ) ;
#31903 = CARTESIAN_POINT ( 'NONE',  ( 757.0176451133909268, -205.0999726633346256, 349.9200121543848354 ) ) ;
#31904 = CARTESIAN_POINT ( 'NONE',  ( 815.3608509340175488, -74.73633629969866377, -341.2497674668889545 ) ) ;
#31905 = CARTESIAN_POINT ( 'NONE',  ( 801.3366627262608972, -80.53286901714194812, -353.0897708529566899 ) ) ;
#31906 = CARTESIAN_POINT ( 'NONE',  ( 766.5853460496234675, -85.98741447168738716, 372.3518521366060554 ) ) ;
#31907 = CARTESIAN_POINT ( 'NONE',  ( 768.0187753319979720, -392.6346026584193396, 318.0580252608186242 ) ) ;
#31908 = CARTESIAN_POINT ( 'NONE',  ( 751.2241431872005251, -160.1692326535053326, 359.9636004259367610 ) ) ;
#31909 = CARTESIAN_POINT ( 'NONE',  ( 774.6312213355099630, 0.6381246143067236254, -364.6798772138717482 ) ) ;
#31910 = ORIENTED_EDGE ( 'NONE', *, *, #4150, .T. ) ;
#31911 = CARTESIAN_POINT ( 'NONE',  ( 801.9419747391806368, -114.4527844766020053, -351.9812246680014027 ) ) ;
#31912 = CARTESIAN_POINT ( 'NONE',  ( 755.8398074228967971, -403.4419599262317888, -333.4516893846970333 ) ) ;
#31914 = CARTESIAN_POINT ( 'NONE',  ( 781.8018195045267476, -214.2709662947834772, 365.1927285166407273 ) ) ;
#31913 = CARTESIAN_POINT ( 'NONE',  ( 791.9812246680005501, -212.6346026584198796, 361.9419747391813189 ) ) ;
#31915 = VECTOR ( 'NONE', #16966, 1000.000000000000000 ) ;
#31916 = CARTESIAN_POINT ( 'NONE',  ( 788.7631598425961101, -409.4419599262317320, -305.7194118038759143 ) ) ;
#31917 = FACE_OUTER_BOUND ( 'NONE', #9573, .T. ) ;
#31918 = ORIENTED_EDGE ( 'NONE', *, *, #24423, .F. ) ;
#31919 = CARTESIAN_POINT ( 'NONE',  ( 803.6646147819161570, -425.9073299311463074, 348.8264449731210561 ) ) ;
#31920 = VERTEX_POINT ( 'NONE', #19933 ) ;
#31921 = CARTESIAN_POINT ( 'NONE',  ( 801.1904061080336987, -260.0891481129650060, -368.3070685750235498 ) ) ;
#31922 = CARTESIAN_POINT ( 'NONE',  ( 792.3570229623691148, -165.1800572038745543, 373.1304606946836770 ) ) ;
#31923 = CARTESIAN_POINT ( 'NONE',  ( 801.5560724626406000, -264.5545181178798657, 326.7756240680316182 ) ) ;
#31924 = ORIENTED_EDGE ( 'NONE', *, *, #29481, .F. ) ;
#31925 = CARTESIAN_POINT ( 'NONE',  ( 768.8385539511368734, -191.2601417444143976, 306.4236121716840557 ) ) ;
#31926 = CARTESIAN_POINT ( 'NONE',  ( 771.1735550268780344, -249.1800572038742700, -316.3353852180828198 ) ) ;
#31927 = EDGE_CURVE ( 'NONE', #38417, #44323, #13007, .T. ) ;
#31928 = EDGE_LOOP ( 'NONE', ( #11622, #5802 ) ) ;
#31929 = CARTESIAN_POINT ( 'NONE',  ( 792.1044303154645831, -372.4527844766010958, -317.8323909638837677 ) ) ;
#31930 = CARTESIAN_POINT ( 'NONE',  ( 756.5762568750052424, -27.18005720387500901, -348.7366044899774238 ) ) ;
#31931 = CARTESIAN_POINT ( 'NONE',  ( 805.0264073115434940, -222.3510508353233206, 339.4763451958999099 ) ) ;
#31932 = FACE_OUTER_BOUND ( 'NONE', #7007, .T. ) ;
#31933 = ADVANCED_FACE ( 'NONE', ( #41187 ), #2362, .F. ) ;
#31934 = CARTESIAN_POINT ( 'NONE',  ( 799.9999999999993179, 205.0000000000000568, -329.9999999999999432 ) ) ;
#31935 = ORIENTED_EDGE ( 'NONE', *, *, #39941, .T. ) ;
#31936 = CARTESIAN_POINT ( 'NONE',  ( 755.3201227861273992, -3.725511749329622813, -345.3687786644892981 ) ) ;
#31937 = DIRECTION ( 'NONE',  ( -0.000000000000000000, -0.000000000000000000, 1.000000000000000000 ) ) ;
#31938 = ORIENTED_EDGE ( 'NONE', *, *, #32500, .F. ) ;
#31939 = CARTESIAN_POINT ( 'NONE',  ( 811.3240766477731540, -268.3726999360616787, -355.6651683502462902 ) ) ;
#31940 = CARTESIAN_POINT ( 'NONE',  ( 768.9521613784389729, -153.8272453906075157, 373.2346286133773106 ) ) ;
#31942 = CARTESIAN_POINT ( 'NONE',  ( 759.9864689768902508, -242.0891481129652618, -354.9819416627836404 ) ) ;
#31941 = DIRECTION ( 'NONE',  ( 0.000000000000000000, -0.3826834323650835645, -0.9238795325112892920 ) ) ;
#31943 = CARTESIAN_POINT ( 'NONE',  ( 758.6633372737375112, -380.5328690171409676, -326.9102291470432533 ) ) ;
#31944 = CARTESIAN_POINT ( 'NONE',  ( 441.1634899080286232, 256.4999999999999432, -202.7499999999971578 ) ) ;
#31945 = CARTESIAN_POINT ( 'NONE',  ( 786.5483106153019435, -127.6454272087894140, -364.1601925771022366 ) ) ;
#31946 = MANIFOLD_SOLID_BREP ( '<Treadle Extension Return Springs>-<Move Face1>', #12899 ) ;
#31947 = CONICAL_SURFACE ( 'NONE', #29741, 8.024999999999948841, 0.7853981633974337351 ) ;
#31948 = CARTESIAN_POINT ( 'NONE',  ( 571.1634899080285095, 256.4999999999999432, -206.1189999999981239 ) ) ;
#31949 = CARTESIAN_POINT ( 'NONE',  ( 801.9858362298568863, -3.078323562596726681, -312.7379699480935642 ) ) ;
#31950 = CARTESIAN_POINT ( 'NONE',  ( 804.7487373415286811, -307.5436935675104451, -364.7487373415288516 ) ) ;
#31951 = SURFACE_STYLE_USAGE ( .BOTH. , #34523 ) ;
#31952 = CARTESIAN_POINT ( 'NONE',  ( 774.6312213355099630, -23.36187538569318889, 364.6798772138717482 ) ) ;
#31953 = PRODUCT_DEFINITION_FORMATION_WITH_SPECIFIED_SOURCE ( 'ANY', '', #2631, .NOT_KNOWN. ) ;
#31954 = CARTESIAN_POINT ( 'NONE',  ( 776.2046728542105711, -236.1908817542436338, 304.8212110874238761 ) ) ;
#31955 = CARTESIAN_POINT ( 'NONE',  ( 761.9338519418445230, -206.5328690171415360, -370.4231160770881957 ) ) ;
#31956 = CARTESIAN_POINT ( 'NONE',  ( 814.9108240113580450, -232.2709662947834488, 337.5031285880265273 ) ) ;
#31957 = CARTESIAN_POINT ( 'NONE',  ( 754.9967657858570647, -433.5436935675099903, -365.0032342141425374 ) ) ;
#31958 = LINE ( 'NONE', #43050, #23948 ) ;
#31959 = CARTESIAN_POINT ( 'NONE',  ( 801.9419747391806368, -330.4527844766013231, 351.9812246680014027 ) ) ;
#31960 = CARTESIAN_POINT ( 'NONE',  ( 766.9102291470427417, -90.55451811788041994, 318.6633372737382501 ) ) ;
#31961 = CARTESIAN_POINT ( 'NONE',  ( 804.1105419155481968, -75.82724539060775726, 347.6308680596136469 ) ) ;
#31962 = CARTESIAN_POINT ( 'NONE',  ( 754.9735926884551418, 5.648949164675971524, -340.5236548041000333 ) ) ;
#31963 = CARTESIAN_POINT ( 'NONE',  ( -26.63011601220122060, -110.5936016518799221, 750.6326042729449455 ) ) ;
#31964 = VECTOR ( 'NONE', #14208, 1000.000000000000000 ) ;
#31965 = DIRECTION ( 'NONE',  ( 0.000000000000000000, 0.000000000000000000, 1.000000000000000000 ) ) ;
#31967 = CARTESIAN_POINT ( 'NONE',  ( 785.3687786644884454, -371.3618753856919739, 315.3201227861279676 ) ) ;
#31966 = CARTESIAN_POINT ( 'NONE',  ( 790.8726784830453198, -106.7146871989600498, 362.5472867521010585 ) ) ;
#31968 = ORIENTED_EDGE ( 'NONE', *, *, #41885, .T. ) ;
#31969 = CARTESIAN_POINT ( 'NONE',  ( 772.3691319403857278, -287.2601417444140566, -315.8894580844506663 ) ) ;
#31970 = CARTESIAN_POINT ( 'NONE',  ( 802.1676090361156639, -110.6346026584201638, 327.8955696845344505 ) ) ;
#31971 = CARTESIAN_POINT ( 'NONE',  ( 749.5768839229115201, -396.5545181178794678, 358.0661480581553064 ) ) ;
#31972 = CARTESIAN_POINT ( 'NONE',  ( 795.6651683502461765, -298.7146871989593251, -371.3240766477733814 ) ) ;
#31973 = PLANE ( 'NONE',  #30787 ) ;
#31974 = CARTESIAN_POINT ( 'NONE',  ( 749.8865473780648472, -428.5328690171409107, 322.1177392798429082 ) ) ;
#31975 = ORIENTED_EDGE ( 'NONE', *, *, #11683, .F. ) ;
#31976 = CARTESIAN_POINT ( 'NONE',  ( 800.2193346964447755, -306.9982390220558273, 355.1360043628815788 ) ) ;
#31977 = CARTESIAN_POINT ( 'NONE',  ( 780.5290396650775619, -60.35105083532383219, -365.2837595273619513 ) ) ;
#31978 = CARTESIAN_POINT ( 'NONE',  ( 755.0636971347428243, -172.2709662947836478, -341.7834795799807353 ) ) ;
#31979 = CARTESIAN_POINT ( 'NONE',  ( 795.1360043628807261, -212.0891481129652902, -360.2193346964456282 ) ) ;
#31980 = CARTESIAN_POINT ( 'NONE',  ( 802.1676090361156639, -422.6346026584192259, 327.8955696845344505 ) ) ;
#31981 = EDGE_CURVE ( 'NONE', #13477, #29782, #43217, .T. ) ;
#31982 = CARTESIAN_POINT ( 'NONE',  ( 804.7487373415286811, -139.5436935675110135, -364.7487373415288516 ) ) ;
#31983 = ORIENTED_EDGE ( 'NONE', *, *, #45264, .F. ) ;
#31984 = CONICAL_SURFACE ( 'NONE', #1737, 8.025000000000003908, 0.7853981633974482790 ) ;
#31985 = CARTESIAN_POINT ( 'NONE',  ( 756.3353852180820240, -149.9073299311473875, -331.1735550268787733 ) ) ;
#31986 = ORIENTED_EDGE ( 'NONE', *, *, #17642, .T. ) ;
#31987 = CIRCLE ( 'NONE', #18623, 6.118999999999985562 ) ;
#31988 = CARTESIAN_POINT ( 'NONE',  ( 784.1219089521767955, -405.2817908451522158, -315.0488828828318333 ) ) ;
#31989 = CARTESIAN_POINT ( 'NONE',  ( 763.8424801807145741, -450.0090635724248500, 320.5453621957614700 ) ) ;
#31990 = CARTESIAN_POINT ( 'NONE',  ( 764.0069404352550464, -135.0783235625962959, 359.2566176426627180 ) ) ;
#31993 = CARTESIAN_POINT ( 'NONE',  ( 744.8212110874229666, -378.8965053807772847, 336.2046728542121627 ) ) ;
#31992 = CARTESIAN_POINT ( 'NONE',  ( -773.4999999999993179, -512.9681489794448908, -350.0000000000000000 ) ) ;
#31991 = FACE_OUTER_BOUND ( 'NONE', #14910, .T. ) ;
#31994 = ADVANCED_FACE ( 'NONE', ( #16930 ), #31010, .F. ) ;
#31995 = ORIENTED_EDGE ( 'NONE', *, *, #37043, .T. ) ;
#31996 = CARTESIAN_POINT ( 'NONE',  ( 804.6971507214547046, -411.2817908451521589, -344.0799538623459739 ) ) ;
#31997 = DIRECTION ( 'NONE',  ( -0.000000000000000000, 1.000000000000000000, -0.000000000000000000 ) ) ;
#31998 = CARTESIAN_POINT ( 'NONE',  ( 768.9521613784389729, -153.8272453906075157, -373.2346286133773106 ) ) ;
#31999 = CARTESIAN_POINT ( 'NONE',  ( 810.4231160770870019, -48.55451811788057626, 321.9338519418446936 ) ) ;
#32000 = CIRCLE ( 'NONE', #38642, 2.749999999999863665 ) ;
#32002 = DIRECTION ( 'NONE',  ( -0.000000000000000000, -0.000000000000000000, -1.000000000000000000 ) ) ;
#32001 = CYLINDRICAL_SURFACE ( 'NONE', #35943, 20.00000000000004974 ) ;
#32003 = CARTESIAN_POINT ( 'NONE',  ( 764.0069404352550464, -303.0783235625957559, -359.2566176426627180 ) ) ;
#32004 = DIRECTION ( 'NONE',  ( -0.000000000000000000, 1.000000000000000000, -0.000000000000000000 ) ) ;
#32005 = CARTESIAN_POINT ( 'NONE',  ( 795.8262568251477660, -190.3726999360619629, -308.3538107759623585 ) ) ;
#32006 = CARTESIAN_POINT ( 'NONE',  ( 779.9999999999992042, 126.4563064324884465, -339.9999999999999432 ) ) ;
#32007 = DIRECTION ( 'NONE',  ( -1.000000000000000000, -0.000000000000000000, 0.000000000000000000 ) ) ;
#32008 = CARTESIAN_POINT ( 'NONE',  ( 755.3028492785439312, -375.2817908451523294, 335.9200461376539693 ) ) ;
#32009 = CARTESIAN_POINT ( 'NONE',  ( 747.6481478633932056, -325.0999726633342561, 353.4146539503763620 ) ) ;
#32010 = CARTESIAN_POINT ( 'NONE',  ( 767.6429770376291799, -201.1800572038744690, -306.8695393053162093 ) ) ;
#32011 = EDGE_CURVE ( 'NONE', #40960, #12731, #4136, .T. ) ;
#32012 = DIRECTION ( 'NONE',  ( 0.000000000000000000, 0.000000000000000000, -1.000000000000000000 ) ) ;
#32013 = DIRECTION ( 'NONE',  ( 0.000000000000000000, 0.000000000000000000, 1.000000000000000000 ) ) ;
#32014 = CARTESIAN_POINT ( 'NONE',  ( 766.4474001241216001, -139.0999726633348530, 307.3154664389482491 ) ) ;
#32015 = ADVANCED_FACE ( 'NONE', ( #20825 ), #17385, .F. ) ;
#32016 = CARTESIAN_POINT ( 'NONE',  ( 776.2433038121456548, -108.8965053807782084, -374.8207195650711014 ) ) ;
#32017 = CARTESIAN_POINT ( 'NONE',  ( 787.5162901302840055, -131.3618753856928834, 305.4481719005792684 ) ) ;
#32018 = CARTESIAN_POINT ( 'NONE',  ( 787.5162901302840055, -347.3618753856922012, -305.4481719005792684 ) ) ;
#32019 = CARTESIAN_POINT ( 'NONE',  ( 311.1634899080286232, 240.0000000000000000, -199.9999999999963336 ) ) ;
#32020 = DIRECTION ( 'NONE',  ( 0.000000000000000000, 0.000000000000000000, 1.000000000000000000 ) ) ;
#32021 = CARTESIAN_POINT ( 'NONE',  ( 774.6312213355099630, -215.3618753856925423, 364.6798772138717482 ) ) ;
#32022 =( GEOMETRIC_REPRESENTATION_CONTEXT ( 3 ) GLOBAL_UNCERTAINTY_ASSIGNED_CONTEXT ( ( #1468 ) ) GLOBAL_UNIT_ASSIGNED_CONTEXT ( ( #40729, #22722, #33804 ) ) REPRESENTATION_CONTEXT ( 'NONE', 'WORKASPACE' ) );
#32023 = VECTOR ( 'NONE', #21796, 1000.000000000000000 ) ;
#32024 = CARTESIAN_POINT ( 'NONE',  ( 784.1219089521767955, 2.718209154846545683, 315.0488828828318333 ) ) ;
#32025 = CARTESIAN_POINT ( 'NONE',  ( 748.3538107759620743, -424.7146871989589840, -355.8262568251490165 ) ) ;
#32026 = CARTESIAN_POINT ( 'NONE',  ( 751.9810565676468741, -410.0891481129647218, -360.9747183278973921 ) ) ;
#32027 = DIRECTION ( 'NONE',  ( 1.000000000000000000, 2.313994520913686024E-32, 2.750100768424433609E-32 ) ) ;
#32028 = CARTESIAN_POINT ( 'NONE',  ( 811.6461892240364477, -4.714687198960358039, 324.1737431748509835 ) ) ;
#32029 = ORIENTED_EDGE ( 'NONE', *, *, #18681, .T. ) ;
#32030 = CARTESIAN_POINT ( 'NONE',  ( 756.1443688327750579, -189.6237781080507148, -314.3581564841659315 ) ) ;
#32031 = DIRECTION ( 'NONE',  ( 1.000000000000000000, -0.000000000000000000, -0.000000000000000000 ) ) ;
#32032 = CARTESIAN_POINT ( 'NONE',  ( 758.0141637701419768, -327.0783235625956991, 367.2620300519063790 ) ) ;
#32033 = CARTESIAN_POINT ( 'NONE',  ( 774.6858677611749044, -129.7255117493292289, 315.5713283507209894 ) ) ;
#32034 = ORIENTED_EDGE ( 'NONE', *, *, #8094, .F. ) ;
#32035 = AXIS2_PLACEMENT_3D ( 'NONE', #33456, #5741, #29994 ) ;
#32036 = ADVANCED_FACE ( 'NONE', ( #22362 ), #1575, .F. ) ;
#32037 = CARTESIAN_POINT ( 'NONE',  ( 774.6858677611749044, -297.7255117493286889, 315.5713283507209894 ) ) ;
#32038 = AXIS2_PLACEMENT_3D ( 'NONE', #32019, #14252, #35484 ) ;
#32039 = EDGE_CURVE ( 'NONE', #19801, #3816, #4388, .T. ) ;
#32040 = CARTESIAN_POINT ( 'NONE',  ( 745.7998596910086917, -53.36187538569310362, -332.5602148656461168 ) ) ;
#32041 = CARTESIAN_POINT ( 'NONE',  ( 749.2812353651451076, -78.45278447660211896, 323.2262854647983090 ) ) ;
#32042 = ORIENTED_EDGE ( 'NONE', *, *, #33687, .F. ) ;
#32043 = CARTESIAN_POINT ( 'NONE',  ( 768.9521613784389729, -441.8272453906066630, -373.2346286133773106 ) ) ;
#32044 = ORIENTED_EDGE ( 'NONE', *, *, #6310, .T. ) ;
#32045 = CARTESIAN_POINT ( 'NONE',  ( 785.3141322388236176, -21.72551174932956641, 364.4286716492789537 ) ) ;
#32046 = CARTESIAN_POINT ( 'NONE',  ( 803.6646147819161570, -305.9073299311467622, -348.8264449731210561 ) ) ;
#32048 = CARTESIAN_POINT ( 'NONE',  ( 788.7631598425961101, -289.4419599262321299, 305.7194118038759143 ) ) ;
#32047 = CARTESIAN_POINT ( 'NONE',  ( 804.7487373415286811, -379.5436935675102745, 364.7487373415288516 ) ) ;
#32049 = ADVANCED_FACE ( 'NONE', ( #18478 ), #52, .F. ) ;
#32050 = CARTESIAN_POINT ( 'NONE',  ( 788.7631598425961101, -73.44195992623286884, 305.7194118038759143 ) ) ;
#32051 = CARTESIAN_POINT ( 'NONE',  ( 772.4468031744293057, -297.8272453906070041, -363.8651313633793620 ) ) ;
#32052 = CARTESIAN_POINT ( 'NONE',  ( 802.1676090361156639, -254.6346026584196238, -327.8955696845344505 ) ) ;
#32053 = DIRECTION ( 'NONE',  ( 0.000000000000000000, 0.000000000000000000, 1.000000000000000000 ) ) ;
#32054 = CARTESIAN_POINT ( 'NONE',  ( 768.0187753319979720, -128.6346026584201354, -318.0580252608186242 ) ) ;
#32055 = VECTOR ( 'NONE', #15288, 1000.000000000000000 ) ;
#32056 = DIRECTION ( 'NONE',  ( -2.750100768424433062E-32, 1.672022627447525240E-16, 1.000000000000000000 ) ) ;
#32057 = CARTESIAN_POINT ( 'NONE',  ( 777.5031285880264704, -406.8164208402375266, 374.9108240113588408 ) ) ;
#32058 = VECTOR ( 'NONE', #43489, 1000.000000000000000 ) ;
#32060 = CARTESIAN_POINT ( 'NONE',  ( 759.9999999999992042, 166.4563064324884465, -319.9999999999999432 ) ) ;
#32059 = DIRECTION ( 'NONE',  ( -0.000000000000000000, -0.000000000000000000, 1.000000000000000000 ) ) ;
#32061 = CARTESIAN_POINT ( 'NONE',  ( 805.6418435158337843, -77.46360902697138329, -363.8556311672236916 ) ) ;
#32062 = DIRECTION ( 'NONE',  ( 0.000000000000000000, -0.6594541114781790059, -0.7517448203044204691 ) ) ;
#32063 = PLANE ( 'NONE',  #43691 ) ;
#32064 = CARTESIAN_POINT ( 'NONE',  ( 800.9840315886518738, -268.9181544815162397, 354.1144889064786412 ) ) ;
#32065 = CARTESIAN_POINT ( 'NONE',  ( 771.2633955100217236, -167.9073299311473022, 363.4237431249939618 ) ) ;
#32066 = ORIENTED_EDGE ( 'NONE', *, *, #38002, .T. ) ;
#32067 = CARTESIAN_POINT ( 'NONE',  ( 799.2566176426618085, -48.00906357242602951, -324.0069404352559559 ) ) ;
#32068 = CARTESIAN_POINT ( 'NONE',  ( 763.0537975583476964, -96.45278447660204790, -371.0346526505628617 ) ) ;
#32069 = CARTESIAN_POINT ( 'NONE',  ( 793.2243759319678702, -314.5328690171411949, 318.4439275373583200 ) ) ;
#32070 = PLANE ( 'NONE',  #19690 ) ;
#32071 = AXIS2_PLACEMENT_3D ( 'NONE', #36184, #15406, #42428 ) ;
#32072 = CARTESIAN_POINT ( 'NONE',  ( 771.3260364891663130, -43.64542720878966975, 306.0683387631859773 ) ) ;
#32073 = CARTESIAN_POINT ( 'NONE',  ( 747.2067596250078623, -219.1800572038744122, -352.2312462859687230 ) ) ;
#32074 = VECTOR ( 'NONE', #23439, 1000.000000000000000 ) ;
#32075 = CIRCLE ( 'NONE', #7028, 6.118999999999985562 ) ;
#32076 = CARTESIAN_POINT ( 'NONE',  ( 777.5031285880264704, -214.8164208402380666, 374.9108240113588408 ) ) ;
#32077 = CARTESIAN_POINT ( 'NONE',  ( 781.8018195045266339, -70.27096629478397460, 365.1927285166406705 ) ) ;
#32078 = DIRECTION ( 'NONE',  ( -1.000000000000000000, 0.000000000000000000, 0.000000000000000000 ) ) ;
#32079 = CARTESIAN_POINT ( 'NONE',  ( 815.1787889125755555, -294.8965053807775689, -343.7953271457877804 ) ) ;
#32080 = CARTESIAN_POINT ( 'NONE',  ( 788.6739635108323228, -439.6454272087884760, 373.9316612368139090 ) ) ;
#32081 = CARTESIAN_POINT ( 'NONE',  ( 792.3570229623688874, -309.1800572038740711, -373.1304606946836202 ) ) ;
#32082 = DIRECTION ( 'NONE',  ( 1.000000000000000000, 0.000000000000000000, 0.000000000000000000 ) ) ;
#32083 = CARTESIAN_POINT ( 'NONE',  ( 770.0799878456142551, -373.9874144716864066, 362.9823548866085616 ) ) ;
#32084 = CARTESIAN_POINT ( 'NONE',  ( 814.5518280994195948, -39.72551174932951312, 332.4837098697145166 ) ) ;
#32085 = CARTESIAN_POINT ( 'NONE',  ( 757.8323909638827445, -386.6346026584191691, -352.1044303154654358 ) ) ;
#32086 = CARTESIAN_POINT ( 'NONE',  ( 769.1273215169530886, -70.71468719896014932, 317.4527132478988847 ) ) ;
#32087 = CARTESIAN_POINT ( 'NONE',  ( 805.1927285166397041, -208.8164208402380666, -341.8018195045277707 ) ) ;
#32088 = AXIS2_PLACEMENT_3D ( 'NONE', #20312, #3459, #45043 ) ;
#32089 = CARTESIAN_POINT ( 'NONE',  ( 808.7758568127978833, -76.16923265350557415, -320.0363995740631822 ) ) ;
#32090 = CARTESIAN_POINT ( 'NONE',  ( 808.7758568127978833, -196.1692326535052473, 320.0363995740631822 ) ) ;
#32091 = CARTESIAN_POINT ( 'NONE',  ( 774.6858677611749044, -9.725511749329603717, 315.5713283507209894 ) ) ;
#32092 = ADVANCED_BREP_SHAPE_REPRESENTATION ( '', ( #32652, #26858 ), #21701 ) ;
#32093 = AXIS2_PLACEMENT_3D ( 'NONE', #17825, #10659, #18054 ) ;
#32094 = EDGE_CURVE ( 'NONE', #12779, #7478, #14146, .T. ) ;
#32095 = CARTESIAN_POINT ( 'NONE',  ( 764.0069404352550464, -375.0783235625955285, 359.2566176426627180 ) ) ;
#32096 = ORIENTED_EDGE ( 'NONE', *, *, #20154, .F. ) ;
#32097 = CARTESIAN_POINT ( 'NONE',  ( 755.0488828828309806, -185.8055962898689302, -344.1219089521771934 ) ) ;
#32098 = CARTESIAN_POINT ( 'NONE',  ( 767.8955696845333705, -216.4527844766016926, 362.1676090361162323 ) ) ;
#32099 = CARTESIAN_POINT ( 'NONE',  ( 749.8865473780648472, -20.53286901714212931, -322.1177392798429082 ) ) ;
#32100 = CARTESIAN_POINT ( 'NONE',  ( 757.8323909638828582, -338.6346026584195101, 352.1044303154654358 ) ) ;
#32101 = CONICAL_SURFACE ( 'NONE', #29179, 8.024999999999948841, 0.7853981633974337351 ) ;
#32102 = CARTESIAN_POINT ( 'NONE',  ( 796.9142768083648889, -452.9681489794446634, -358.6301678913937963 ) ) ;
#32103 = LINE ( 'NONE', #28176, #22019 ) ;
#32104 = ORIENTED_EDGE ( 'NONE', *, *, #7473, .T. ) ;
#32105 = CARTESIAN_POINT ( 'NONE',  ( 804.9511171171677688, -53.80559628986930676, 335.8780910478229202 ) ) ;
#32106 = CARTESIAN_POINT ( 'NONE',  ( 750.9282345327678740, -352.9181544815159555, -319.8311093483690115 ) ) ;
#32107 = VECTOR ( 'NONE', #24350, 1000.000000000000000 ) ;
#32108 = ADVANCED_FACE ( 'NONE', ( #22151 ), #15675, .F. ) ;
#32109 = AXIS2_PLACEMENT_3D ( 'NONE', #40716, #37245, #36583 ) ;
#32110 = CARTESIAN_POINT ( 'NONE',  ( 805.0032342141413437, -301.5436935675105588, 314.9967657858572352 ) ) ;
#32111 = CARTESIAN_POINT ( 'NONE',  ( 791.1614460488616487, -11.26014174441488258, 373.5763878283158874 ) ) ;
#32112 = CARTESIAN_POINT ( 'NONE',  ( 793.9708237608222134, -190.9181544815164955, -319.2295555964448681 ) ) ;
#32113 = CARTESIAN_POINT ( 'NONE',  ( 792.1044303154645831, -156.4527844766018916, -317.8323909638837677 ) ) ;
#32114 = CARTESIAN_POINT ( 'NONE',  ( 765.0180583372156207, -336.9982390220558273, -360.0135310231089534 ) ) ;
#32115 = ORIENTED_EDGE ( 'NONE', *, *, #24682, .T. ) ;
#32116 = CARTESIAN_POINT ( 'NONE',  ( 773.3843516231979720, 10.55804007376686826, -364.4086373105754433 ) ) ;
#32117 = CARTESIAN_POINT ( 'NONE',  ( 767.6429770376289525, -273.1800572038742985, 306.8695393053162093 ) ) ;
#32118 = DIRECTION ( 'NONE',  ( 0.000000000000000000, 0.000000000000000000, -1.000000000000000000 ) ) ;
#32119 = CARTESIAN_POINT ( 'NONE',  ( 773.3843516231979720, -349.4419599262320162, 364.4086373105754433 ) ) ;
#32120 = FACE_OUTER_BOUND ( 'NONE', #9089, .T. ) ;
#32121 = CARTESIAN_POINT ( 'NONE',  ( 755.1538015810308480, -158.1908817542438612, 343.0433043558613804 ) ) ;
#32122 = CARTESIAN_POINT ( 'NONE',  ( 797.8594530101008786, -37.54369356751132614, 322.1405469898980982 ) ) ;
#32123 = ORIENTED_EDGE ( 'NONE', *, *, #40670, .T. ) ;
#32124 = CARTESIAN_POINT ( 'NONE',  ( 783.7953271457878373, -368.1908817542433212, -375.1787889125761239 ) ) ;
#32125 = AXIS2_PLACEMENT_3D ( 'NONE', #15215, #7364, #43377 ) ;
#32126 = CARTESIAN_POINT ( 'NONE',  ( 787.4397851343537695, 2.274488250670355871, -374.2001403089903988 ) ) ;
#32127 = CARTESIAN_POINT ( 'NONE',  ( 748.6759233522253680, -280.3726999360616787, 324.3348316497537098 ) ) ;
#32128 = CARTESIAN_POINT ( 'NONE',  ( 787.6308680596127942, -179.2601417444143692, 364.1105419155492768 ) ) ;
#32129 = AXIS2_PLACEMENT_3D ( 'NONE', #17922, #11221, #3833 ) ;
#32130 = CARTESIAN_POINT ( 'NONE',  ( 794.9819416627830151, -348.9982390220558273, -319.9864689768909898 ) ) ;
#32131 = CARTESIAN_POINT ( 'NONE',  ( 764.8639956371174549, 15.91085188703394238, 319.7806653035542013 ) ) ;
#32132 = LINE ( 'NONE', #10898, #6744 ) ;
#32133 = CARTESIAN_POINT ( 'NONE',  ( 772.4468031744293057, -225.8272453906072599, -363.8651313633793620 ) ) ;
#32134 = CARTESIAN_POINT ( 'NONE',  ( 787.5162901302840055, -11.36187538569323863, 305.4481719005792684 ) ) ;
#32135 = CARTESIAN_POINT ( 'NONE',  ( 744.7301800767019131, -124.8164208402383508, 337.4774526936615757 ) ) ;
#32136 = LINE ( 'NONE', #7656, #33572 ) ;
#32137 = CARTESIAN_POINT ( 'NONE',  ( 763.0537975583476964, -432.4527844766009252, -371.0346526505628617 ) ) ;
#32138 = CARTESIAN_POINT ( 'NONE',  ( 355.8971257818259915, 290.0000000000001137, -244.9999999999999716 ) ) ;
#32139 = AXIS2_PLACEMENT_3D ( 'NONE', #9541, #34702, #20607 ) ;
#32140 = CARTESIAN_POINT ( 'NONE',  ( 764.1737431748507561, -370.3726999360613377, 371.6461892240376415 ) ) ;
#32141 = FACE_OUTER_BOUND ( 'NONE', #41660, .T. ) ;
#32142 = CARTESIAN_POINT ( 'NONE',  ( 810.7187646348534145, -330.4527844766013231, 356.7737145352016341 ) ) ;
#32143 = CARTESIAN_POINT ( 'NONE',  ( 813.1304606946830518, -41.90732993114767169, -352.3570229623690580 ) ) ;
#32144 = CARTESIAN_POINT ( 'NONE',  ( 755.5713283507202505, -293.3618753856923718, -334.6858677611754729 ) ) ;
#32145 = CIRCLE ( 'NONE', #6325, 6.118999999999985562 ) ;
#32146 = LINE ( 'NONE', #16748, #9244 ) ;
#32147 = CARTESIAN_POINT ( 'NONE',  ( 762.3223304703356007, -439.5436935675101040, 322.3223304703362828 ) ) ;
#32148 = CARTESIAN_POINT ( 'NONE',  ( 775.8780910478218402, -177.2817908451528695, 364.9511171171680530 ) ) ;
#32149 = CARTESIAN_POINT ( 'NONE',  ( 804.1009440267234822, -71.46360902697141171, -314.0944755984392600 ) ) ;
#32150 = CARTESIAN_POINT ( 'NONE',  ( 796.7845633553578182, -81.62377810805104161, -358.5707757039688204 ) ) ;
#32151 = CARTESIAN_POINT ( 'NONE',  ( 746.0683387631852383, -91.44195992623282621, 331.3260364891676204 ) ) ;
#32152 = CARTESIAN_POINT ( 'NONE',  ( 759.7806653035535192, -390.9982390220556567, 324.8639956371181370 ) ) ;
#32153 = CARTESIAN_POINT ( 'NONE',  ( 815.1787889125755555, -150.8965053807781089, 343.7953271457877804 ) ) ;
#32154 = CARTESIAN_POINT ( 'NONE',  ( 792.1044303154645831, 11.54721552339760038, -317.8323909638837677 ) ) ;
#32155 = VERTEX_POINT ( 'NONE', #36698 ) ;
#32156 = CARTESIAN_POINT ( 'NONE',  ( 804.6798772138708955, -87.72551174932937101, -334.6312213355107019 ) ) ;
#32157 = CARTESIAN_POINT ( 'NONE',  ( 756.1348686366196716, -401.2601417444137155, -347.5531968255698416 ) ) ;
#32159 = CARTESIAN_POINT ( 'NONE',  ( 803.6646147819162707, -209.9073299311471317, 348.8264449731211130 ) ) ;
#32158 = CARTESIAN_POINT ( 'NONE',  ( 757.8323909638827445, -218.6346026584197944, 352.1044303154654358 ) ) ;
#32160 = CARTESIAN_POINT ( 'NONE',  ( 811.6461892240364477, -412.7146871989590409, -324.1737431748509835 ) ) ;
#32161 = CYLINDRICAL_SURFACE ( 'NONE', #24913, 6.118999999999985562 ) ;
#32162 = ORIENTED_EDGE ( 'NONE', *, *, #12587, .F. ) ;
#32163 = CARTESIAN_POINT ( 'NONE',  ( 797.6776695296629214, -427.5436935675101040, 357.6776695296636603 ) ) ;
#32164 = CIRCLE ( 'NONE', #42484, 10.00000000000000888 ) ;
#32165 = CIRCLE ( 'NONE', #14364, 2.749999999999919176 ) ;
#32166 = EDGE_LOOP ( 'NONE', ( #18595, #39455, #4546, #24949 ) ) ;
#32167 = SHAPE_REPRESENTATION_RELATIONSHIP ( 'NONE' , 'NONE' ,  #36841, #3952 ) ;
#32168 = VECTOR ( 'NONE', #35697, 1000.000000000000000 ) ;
#32169 = CARTESIAN_POINT ( 'NONE',  ( 777.4774526936600978, -250.2709662947832783, -304.7301800767027657 ) ) ;
#32170 = CARTESIAN_POINT ( 'NONE',  ( 745.0891759886404770, -148.2709662947837330, 342.4968714119734159 ) ) ;
#32171 = CARTESIAN_POINT ( 'NONE',  ( 780.5236548040995785, -260.7363362996981095, 314.9735926884559944 ) ) ;
#32172 = ORIENTED_EDGE ( 'NONE', *, *, #1561, .F. ) ;
#32173 = CARTESIAN_POINT ( 'NONE',  ( 769.0155153010367712, -58.37269993606236085, -362.7791456095907279 ) ) ;
#32174 = CARTESIAN_POINT ( 'NONE',  ( 746.7653713866222915, -185.2601417444143692, 351.0478386215610271 ) ) ;
#32175 = CARTESIAN_POINT ( 'NONE',  ( 804.6798772138710092, -231.7255117493288594, -334.6312213355106451 ) ) ;
#32176 = ORIENTED_EDGE ( 'NONE', *, *, #18259, .T. ) ;
#32177 = CARTESIAN_POINT ( 'NONE',  ( 805.1927285166397041, -352.8164208402374129, -341.8018195045277707 ) ) ;
#32178 = CARTESIAN_POINT ( 'NONE',  ( 767.8955696845333705, -48.45278447660219712, -362.1676090361162323 ) ) ;
#32179 = VECTOR ( 'NONE', #21071, 1000.000000000000000 ) ;
#32180 = CARTESIAN_POINT ( 'NONE',  ( 769.1273215169530886, -238.7146871989596661, 317.4527132478988847 ) ) ;
#32181 = DIRECTION ( 'NONE',  ( 0.000000000000000000, 0.000000000000000000, 1.000000000000000000 ) ) ;
#32182 = DIRECTION ( 'NONE',  ( 0.000000000000000000, 4.857225732735055920E-15, -1.000000000000000000 ) ) ;
#32183 = VECTOR ( 'NONE', #18718, 1000.000000000000000 ) ;
#32184 = ORIENTED_EDGE ( 'NONE', *, *, #32833, .F. ) ;
#32185 = CARTESIAN_POINT ( 'NONE',  ( 759.7806653035534055, -6.998239022056885972, -324.8639956371180801 ) ) ;
#32186 = CARTESIAN_POINT ( 'NONE',  ( 939.9999999999993179, -419.8175818341089780, -209.9999999999999716 ) ) ;
#32187 = FACE_OUTER_BOUND ( 'NONE', #18498, .T. ) ;
#32188 = ORIENTED_EDGE ( 'NONE', *, *, #20717, .T. ) ;
#32189 = CARTESIAN_POINT ( 'NONE',  ( 766.4474001241216001, -283.0999726633344267, -307.3154664389482491 ) ) ;
#32190 = CARTESIAN_POINT ( 'NONE',  ( 745.5313806188320314, -183.2817908451528695, 333.7943932421247268 ) ) ;
#32192 = CARTESIAN_POINT ( 'NONE',  ( 805.1927285166397041, -256.8164208402379245, -341.8018195045277707 ) ) ;
#32191 = LINE ( 'NONE', #22020, #21685 ) ;
#32193 = FACE_BOUND ( 'NONE', #6538, .T. ) ;
#32194 = CARTESIAN_POINT ( 'NONE',  ( 755.3028492785439312, -111.2817908451530968, -335.9200461376539693 ) ) ;
#32195 = DIRECTION ( 'NONE',  ( 1.000000000000000000, -0.000000000000000000, -0.000000000000000000 ) ) ;
#32196 = CARTESIAN_POINT ( 'NONE',  ( 744.8212110874229666, -18.89650538077849617, -336.2046728542121627 ) ) ;
#32197 = CARTESIAN_POINT ( 'NONE',  ( 763.2262854647970016, -296.6346026584195670, -309.2812353651462445 ) ) ;
#32198 = FACE_OUTER_BOUND ( 'NONE', #19166, .T. ) ;
#32199 = CARTESIAN_POINT ( 'NONE',  ( 781.7834795799800531, -10.81642084023869543, 315.0636971347436202 ) ) ;
#32200 = CARTESIAN_POINT ( 'NONE',  ( 750.9282345327678740, -256.9181544815163534, 319.8311093483690115 ) ) ;
#32201 = CARTESIAN_POINT ( 'NONE',  ( 745.1769319972822814, -209.8055962898687881, -346.2694204179732083 ) ) ;
#32202 = CARTESIAN_POINT ( 'NONE',  ( 814.2001403089898304, -233.3618753856925423, 347.4397851343538264 ) ) ;
#32203 = CARTESIAN_POINT ( 'NONE',  ( 814.9108240113580450, -448.2709662947827951, -337.5031285880265273 ) ) ;
#32204 = VECTOR ( 'NONE', #16043, 1000.000000000000000 ) ;
#32205 = CARTESIAN_POINT ( 'NONE',  ( 200.7583438952259485, 394.6698570112193920, -244.9999999999999716 ) ) ;
#32206 = CARTESIAN_POINT ( 'NONE',  ( 774.6312213355099630, -311.3618753856922581, 364.6798772138717482 ) ) ;
#32207 = CIRCLE ( 'NONE', #13789, 9.999999999999982236 ) ;
#32208 = CARTESIAN_POINT ( 'NONE',  ( 790.0220218866281812, -79.09997266333503774, 363.2186876482849129 ) ) ;
#32209 = CARTESIAN_POINT ( 'NONE',  ( 804.8461984189677878, -74.19088175424410281, 336.9566956441385628 ) ) ;
#32210 = CARTESIAN_POINT ( 'NONE',  ( 794.1144889064781864, 13.83076734649413098, -360.9840315886528401 ) ) ;
#32211 = DIRECTION ( 'NONE',  ( 1.000000000000000000, 0.000000000000000000, 0.000000000000000000 ) ) ;
#32212 = CARTESIAN_POINT ( 'NONE',  ( 789.9999999999992042, 240.0000000000000853, -360.0000000000000000 ) ) ;
#32214 = CARTESIAN_POINT ( 'NONE',  ( 805.1927285166397041, -352.8164208402374129, 341.8018195045277707 ) ) ;
#32213 = CARTESIAN_POINT ( 'NONE',  ( 789.9200121543843807, -145.9874144716871740, 317.0176451133914384 ) ) ;
#32215 = EDGE_LOOP ( 'NONE', ( #2496, #9234, #1572, #19898 ) ) ;
#32216 = VECTOR ( 'NONE', #16797, 1000.000000000000000 ) ;
#32217 = CARTESIAN_POINT ( 'NONE',  ( 765.8855110935204493, -286.1692326535048778, -319.0159684113471599 ) ) ;
#32218 = CARTESIAN_POINT ( 'NONE',  ( 795.1360043628807261, -140.0891481129654892, 360.2193346964456282 ) ) ;
#32219 = ADVANCED_FACE ( 'NONE', ( #19148 ), #11546, .T. ) ;
#32220 = CARTESIAN_POINT ( 'NONE',  ( 746.7653713866222915, -281.2601417444139997, -351.0478386215610271 ) ) ;
#32221 = CARTESIAN_POINT ( 'NONE',  ( -879.9999999999992042, 240.0000000000002274, -244.9999999999999716 ) ) ;
#32222 = CARTESIAN_POINT ( 'NONE',  ( 747.3154664389472828, -427.9874144716862929, 326.4474001241230781 ) ) ;
#32223 = ORIENTED_EDGE ( 'NONE', *, *, #24269, .T. ) ;
#32224 = CARTESIAN_POINT ( 'NONE',  ( 803.4237431249931660, -327.1800572038741279, 331.2633955100225194 ) ) ;
#32225 = CARTESIAN_POINT ( 'NONE',  ( 764.0069404352550464, -63.07832356259653750, -359.2566176426627180 ) ) ;
#32226 = CARTESIAN_POINT ( 'NONE',  ( 764.8639956371174549, -152.0891481129655460, -319.7806653035542013 ) ) ;
#32227 = CARTESIAN_POINT ( 'NONE',  ( 774.6312213355099630, -215.3618753856925423, -364.6798772138717482 ) ) ;
#32228 = CARTESIAN_POINT ( 'NONE',  ( 755.3201227861273992, -435.7255117493282341, 345.3687786644892981 ) ) ;
#32229 = CARTESIAN_POINT ( 'NONE',  ( 808.0189434323515343, -134.0891481129655745, -319.0252816721025511 ) ) ;
#32230 = ORIENTED_EDGE ( 'NONE', *, *, #27552, .T. ) ;
#32231 = CARTESIAN_POINT ( 'NONE',  ( 778.2165204200184689, -142.8164208402382656, -364.9363028652563230 ) ) ;
#32232 = VERTEX_POINT ( 'NONE', #43622 ) ;
#32233 = CARTESIAN_POINT ( 'NONE',  ( 802.9823548866075953, -385.0999726633340856, -330.0799878456151077 ) ) ;
#32234 = CARTESIAN_POINT ( 'NONE',  ( 791.9812246680005501, 3.365397341579444479, 361.9419747391813189 ) ) ;
#32235 = CARTESIAN_POINT ( 'NONE',  ( 808.0189434323515343, -230.0891481129652618, 319.0252816721025511 ) ) ;
#32236 = CARTESIAN_POINT ( 'NONE',  ( 766.7756240680305382, -110.5328690171418629, 361.5560724626415663 ) ) ;
#32237 = VECTOR ( 'NONE', #15650, 1000.000000000000000 ) ;
#32240 = CARTESIAN_POINT ( 'NONE',  ( 800.1688906516307043, -394.1692326535045368, 369.0717654672308186 ) ) ;
#32239 = DIRECTION ( 'NONE',  ( 1.000000000000000000, 0.000000000000000000, 0.000000000000000000 ) ) ;
#32238 = CARTESIAN_POINT ( 'NONE',  ( 779.9999999999992042, 126.4563064324884465, -339.9999999999999432 ) ) ;
#32241 = ORIENTED_EDGE ( 'NONE', *, *, #18664, .T. ) ;
#32242 = CARTESIAN_POINT ( 'NONE',  ( 784.1219089521767955, -381.2817908451523294, -315.0488828828318333 ) ) ;
#32243 = LINE ( 'NONE', #14704, #24774 ) ;
#32244 = CARTESIAN_POINT ( 'NONE',  ( 811.3240766477731540, -172.3726999360619914, -355.6651683502462902 ) ) ;
#32245 = CARTESIAN_POINT ( 'NONE',  ( 812.3518521366052028, -25.09997266333519050, 326.5853460496235243 ) ) ;
#32246 = CONICAL_SURFACE ( 'NONE', #18250, 8.025000000000003908, 0.7853981633974410625 ) ;
#32248 = FACE_OUTER_BOUND ( 'NONE', #2381, .T. ) ;
#32247 = DIRECTION ( 'NONE',  ( -0.000000000000000000, 1.000000000000000000, -0.000000000000000000 ) ) ;
#32249 = CARTESIAN_POINT ( 'NONE',  ( 783.0433043558608688, -312.8965053807775689, -315.1538015810313027 ) ) ;
#32250 = CARTESIAN_POINT ( 'NONE',  ( 755.3201227861273992, -435.7255117493282341, -345.3687786644892981 ) ) ;
#32251 = CARTESIAN_POINT ( 'NONE',  ( 810.4231160770870019, -192.5545181178801215, -321.9338519418446936 ) ) ;
#32252 = PLANE ( 'NONE',  #39269 ) ;
#32253 = CARTESIAN_POINT ( 'NONE',  ( -858.8365100919713768, 256.5000000000002274, -199.9999999999881481 ) ) ;
#32254 = AXIS2_PLACEMENT_3D ( 'NONE', #16047, #40080, #2399 ) ;
#32255 = CARTESIAN_POINT ( 'NONE',  ( 776.9254006560222479, -380.1908817542431507, 314.8983024940802125 ) ) ;
#32256 = CARTESIAN_POINT ( 'NONE',  ( 778.7629533639073998, -344.7363362996978253, 375.0009284576466371 ) ) ;
#32257 = CARTESIAN_POINT ( 'NONE',  ( 814.2001403089898304, -209.3618753856926276, -347.4397851343538264 ) ) ;
#32258 = DIRECTION ( 'NONE',  ( -0.000000000000000000, 1.000000000000000000, -0.000000000000000000 ) ) ;
#32259 = CARTESIAN_POINT ( 'NONE',  ( 754.8072714833581358, -4.816420840238714085, -338.1981804954720587 ) ) ;
#32260 = CARTESIAN_POINT ( 'NONE',  ( 791.0478386215596629, -141.8272453906075157, 306.7653713866226326 ) ) ;
#32261 = CARTESIAN_POINT ( 'NONE',  ( 745.1769319972822814, -89.80559628986918597, -346.2694204179732083 ) ) ;
#32262 = CARTESIAN_POINT ( 'NONE',  ( 815.2698199232961542, -112.8164208402383508, 342.5225473063383106 ) ) ;
#32263 = CARTESIAN_POINT ( 'NONE',  ( 796.9462024416508257, -348.4527844766012663, -308.9653473494370246 ) ) ;
#32264 = EDGE_CURVE ( 'NONE', #25758, #42149, #18932, .T. ) ;
#32265 = CARTESIAN_POINT ( 'NONE',  ( 799.9999999999993179, 166.4563064324884465, 360.0000000000000000 ) ) ;
#32266 = CARTESIAN_POINT ( 'NONE',  ( -858.8365100919713768, 240.0000000000002274, -202.7499999999880345 ) ) ;
#32267 = CARTESIAN_POINT ( 'NONE',  ( 754.8072714833581358, -220.8164208402379529, 338.1981804954720587 ) ) ;
#32268 = CARTESIAN_POINT ( 'NONE',  ( 749.5768839229115201, -444.5545181178792973, 358.0661480581553064 ) ) ;
#32269 = CARTESIAN_POINT ( 'NONE',  ( 815.0009284576459549, -414.3510508353227237, -338.7629533639073429 ) ) ;
#32270 = VECTOR ( 'NONE', #43162, 1000.000000000000000 ) ;
#32271 = CARTESIAN_POINT ( 'NONE',  ( 801.1904061080336987, -428.0891481129644944, -368.3070685750235498 ) ) ;
#32272 = DIRECTION ( 'NONE',  ( -1.880165489482579047E-16, -1.000000000000000000, -0.000000000000000000 ) ) ;
#32273 = CARTESIAN_POINT ( 'NONE',  ( 791.1614460488616487, 12.73985825558503926, 373.5763878283158874 ) ) ;
#32274 = ORIENTED_EDGE ( 'NONE', *, *, #29765, .T. ) ;
#32275 = EDGE_CURVE ( 'NONE', #5448, #39395, #25842, .T. ) ;
#32276 = CARTESIAN_POINT ( 'NONE',  ( 762.3223304703356007, -31.54369356751135456, 322.3223304703362828 ) ) ;
#32277 = CARTESIAN_POINT ( 'NONE',  ( 813.2346286133761168, -173.2601417444143692, -328.9521613784389160 ) ) ;
#32278 = FILL_AREA_STYLE_COLOUR ( '', #17236 ) ;
#32279 = CARTESIAN_POINT ( 'NONE',  ( 807.5423716828161105, -297.0783235625957559, 362.2119215644372048 ) ) ;
#32280 = CARTESIAN_POINT ( 'NONE',  ( 759.9864689768902508, -170.0891481129654608, 354.9819416627836404 ) ) ;
#32281 = VERTEX_POINT ( 'NONE', #5056 ) ;
#32282 = AXIS2_PLACEMENT_3D ( 'NONE', #32221, #581, #28527 ) ;
#32283 = CARTESIAN_POINT ( 'NONE',  ( 755.0636971347428243, -292.2709662947831930, 341.7834795799807353 ) ) ;
#32284 = CARTESIAN_POINT ( 'NONE',  ( 767.7687537140311633, -47.90732993114767169, -372.7932403749916830 ) ) ;
#32285 = CARTESIAN_POINT ( 'NONE',  ( 813.1304606946831655, -89.90732993114752958, 352.3570229623691716 ) ) ;
#32286 = EDGE_LOOP ( 'NONE', ( #21158, #21079 ) ) ;
#32287 = CARTESIAN_POINT ( 'NONE',  ( 781.2370466360911223, -452.7363362996975411, -304.9990715423533629 ) ) ;
#32288 = ORIENTED_EDGE ( 'NONE', *, *, #14771, .F. ) ;
#32289 = APPLICATION_PROTOCOL_DEFINITION ( 'draft international standard', 'automotive_design', 1998, #27853 ) ;
#32290 = ADVANCED_FACE ( 'NONE', ( #42311 ), #30689, .F. ) ;
#32292 = CARTESIAN_POINT ( 'NONE',  ( 802.9823548866075953, -337.0999726633342561, 330.0799878456151077 ) ) ;
#32291 = CARTESIAN_POINT ( 'NONE',  ( 755.3201227861273992, -75.72551174932937101, 345.3687786644892981 ) ) ;
#32293 = CARTESIAN_POINT ( 'NONE',  ( 755.5713283507202505, -293.3618753856923718, -334.6858677611754729 ) ) ;
#32295 = CARTESIAN_POINT ( 'NONE',  ( 759.8311093483677041, -286.1692326535048778, 310.9282345327691814 ) ) ;
#32294 = CARTESIAN_POINT ( 'NONE',  ( 787.4397851343537695, -381.7255117493284615, 374.2001403089903988 ) ) ;
#32296 = CARTESIAN_POINT ( 'NONE',  ( 791.1614460488616487, -83.26014174441466764, 373.5763878283158874 ) ) ;
#32297 = EDGE_CURVE ( 'NONE', #31480, #41889, #36239, .T. ) ;
#32298 = CARTESIAN_POINT ( 'NONE',  ( 763.0428371773158460, -299.4636090269707438, -358.7617431975195359 ) ) ;
#32299 = CARTESIAN_POINT ( 'NONE',  ( 764.8639956371174549, -296.0891481129650629, -319.7806653035542013 ) ) ;
#32300 = PLANE ( 'NONE',  #36409 ) ;
#32301 = CARTESIAN_POINT ( 'NONE',  ( 804.4286716492782716, -113.3618753856929260, -345.3141322388244703 ) ) ;
#32302 = DIRECTION ( 'NONE',  ( 5.551115123125783688E-16, -1.000000000000000000, 0.000000000000000000 ) ) ;
#32303 = ORIENTED_EDGE ( 'NONE', *, *, #21571, .T. ) ;
#32304 = CARTESIAN_POINT ( 'NONE',  ( 751.6929314249748586, -390.9982390220557136, 318.8095938919659034 ) ) ;
#32306 = DIRECTION ( 'NONE',  ( 1.000000000000000000, 0.000000000000000000, 0.000000000000000000 ) ) ;
#32305 = CARTESIAN_POINT ( 'NONE',  ( 939.9999999999992042, 240.0000000000000568, -210.0000000000000000 ) ) ;
#32307 = CARTESIAN_POINT ( 'NONE',  ( 746.4236121716829757, -87.82724539060770041, -328.8385539511384650 ) ) ;
#32308 = DIRECTION ( 'NONE',  ( 0.000000000000000000, 0.000000000000000000, 1.000000000000000000 ) ) ;
#32309 = FACE_BOUND ( 'NONE', #30576, .T. ) ;
#32310 = CARTESIAN_POINT ( 'NONE',  ( 804.1105419155481968, -267.8272453906071746, 347.6308680596136469 ) ) ;
#32311 = CARTESIAN_POINT ( 'NONE',  ( 788.8264449731200330, -141.1800572038746395, 363.6646147819171233 ) ) ;
#32312 = ORIENTED_EDGE ( 'NONE', *, *, #728, .F. ) ;
#32313 = CARTESIAN_POINT ( 'NONE',  ( 755.1538015810308480, -38.19088175424422360, -343.0433043558613804 ) ) ;
#32314 = CARTESIAN_POINT ( 'NONE',  ( 814.9108240113580450, -88.27096629478390355, -337.5031285880265273 ) ) ;
#32315 = CARTESIAN_POINT ( 'NONE',  ( 793.2243759319678702, -338.5328690171411381, 318.4439275373583200 ) ) ;
#32316 = VECTOR ( 'NONE', #8360, 1000.000000000000000 ) ;
#32317 = DIRECTION ( 'NONE',  ( 0.000000000000000000, 0.000000000000000000, 1.000000000000000000 ) ) ;
#32318 = EDGE_CURVE ( 'NONE', #5395, #7469, #31686, .T. ) ;
#32319 = CARTESIAN_POINT ( 'NONE',  ( 797.8822607201568644, -30.55451811788062244, 370.1134526219340160 ) ) ;
#32320 = CARTESIAN_POINT ( 'NONE',  ( 814.2001403089898304, -233.3618753856925423, -347.4397851343538264 ) ) ;
#32321 = ADVANCED_FACE ( 'NONE', ( #15468 ), #35154, .F. ) ;
#32322 = CARTESIAN_POINT ( 'NONE',  ( 745.7998596910086917, -197.3618753856926560, 332.5602148656461168 ) ) ;
#32323 = CARTESIAN_POINT ( 'NONE',  ( 792.1044303154645831, -108.4527844766019911, 317.8323909638837677 ) ) ;
#32324 = CYLINDRICAL_SURFACE ( 'NONE', #1132, 12.00000000000001066 ) ;
#32325 = CARTESIAN_POINT ( 'NONE',  ( 800.1688906516307043, -298.1692326535049347, -369.0717654672308186 ) ) ;
#32326 = CARTESIAN_POINT ( 'NONE',  ( 809.0717654672305343, -460.9181544815156713, 360.1688906516309885 ) ) ;
#32327 = CARTESIAN_POINT ( 'NONE',  ( 805.0032342141412300, -325.5436935675105019, -314.9967657858571783 ) ) ;
#32328 = DIRECTION ( 'NONE',  ( 0.000000000000000000, 0.000000000000000000, 1.000000000000000000 ) ) ;
#32329 = CARTESIAN_POINT ( 'NONE',  ( 759.2295555964440155, -352.1692326535046504, 353.9708237608231229 ) ) ;
#32330 = CARTESIAN_POINT ( 'NONE',  ( 782.5225473063383106, -46.27096629478403855, 375.2698199232970637 ) ) ;
#32331 = CARTESIAN_POINT ( 'NONE',  ( 771.1735550268778070, -417.1800572038736163, -316.3353852180827630 ) ) ;
#32332 = EDGE_CURVE ( 'NONE', #5125, #42219, #11549, .T. ) ;
#32333 = CARTESIAN_POINT ( 'NONE',  ( 795.9930595647434757, -51.07832356259657303, 320.7433823573372820 ) ) ;
#32334 = CARTESIAN_POINT ( 'NONE',  ( 759.9864689768902508, -194.0891481129654039, -354.9819416627836404 ) ) ;
#32335 = CARTESIAN_POINT ( 'NONE',  ( 771.2368401574024119, -85.44195992623282621, -374.2805881961240857 ) ) ;
#32336 = CARTESIAN_POINT ( 'NONE',  ( 783.7566961878529810, -192.8965053807779668, 305.1792804349288417 ) ) ;
#32337 = CARTESIAN_POINT ( 'NONE',  ( 795.1360043628808398, -44.08914811296585157, 360.2193346964456282 ) ) ;
#32338 = ORIENTED_EDGE ( 'NONE', *, *, #2117, .T. ) ;
#32339 = CARTESIAN_POINT ( 'NONE',  ( 760.5453621957607311, -189.0783235625961822, -323.8424801807151425 ) ) ;
#32340 = CARTESIAN_POINT ( 'NONE',  ( 771.1735550268778070, -201.1800572038744690, 316.3353852180827630 ) ) ;
#32341 = CARTESIAN_POINT ( 'NONE',  ( 756.1443688327750579, -21.62377810805121570, -314.3581564841659315 ) ) ;
#32342 = CARTESIAN_POINT ( 'NONE',  ( 758.0580252608178853, -342.4527844766013231, 328.0187753319985404 ) ) ;
#32343 = CARTESIAN_POINT ( 'NONE',  ( 799.9999999999993179, -357.6843811873878280, 0.3380660510726891665 ) ) ;
#32344 = DIRECTION ( 'NONE',  ( -1.000000000000000000, -0.000000000000000000, -0.000000000000000000 ) ) ;
#32345 = EDGE_CURVE ( 'NONE', #8411, #39568, #21301, .T. ) ;
#32346 = ORIENTED_EDGE ( 'NONE', *, *, #19891, .F. ) ;
#32347 = CARTESIAN_POINT ( 'NONE',  ( 759.2295555964440155, -64.16923265350563099, 353.9708237608231229 ) ) ;
#32348 = CARTESIAN_POINT ( 'NONE',  ( 745.5313806188320314, -351.2817908451523294, -333.7943932421247268 ) ) ;
#32349 = EDGE_CURVE ( 'NONE', #13695, #11328, #33234, .T. ) ;
#32350 = CARTESIAN_POINT ( 'NONE',  ( 804.7487373415286811, -307.5436935675104451, 364.7487373415288516 ) ) ;
#32351 = CARTESIAN_POINT ( 'NONE',  ( 810.1134526219336749, 15.46713098285775878, 357.8822607201570349 ) ) ;
#32352 = CARTESIAN_POINT ( 'NONE',  ( 757.4527132478984868, -184.3726999360619629, -329.1273215169538844 ) ) ;
#32353 = CARTESIAN_POINT ( 'NONE',  ( 756.3353852180819104, -197.9073299311472169, -331.1735550268788302 ) ) ;
#32354 = CARTESIAN_POINT ( 'NONE',  ( 767.8955696845334842, -360.4527844766011526, -362.1676090361161755 ) ) ;
#32355 = VERTEX_POINT ( 'NONE', #40166 ) ;
#32356 = CARTESIAN_POINT ( 'NONE',  ( 796.9462024416508257, -300.4527844766012663, 308.9653473494370246 ) ) ;
#32357 = CARTESIAN_POINT ( 'NONE',  ( -858.8365100919713768, 256.5000000000002274, -199.9999999999881481 ) ) ;
#32358 = CARTESIAN_POINT ( 'NONE',  ( 798.7617431975189675, -363.6237781080502032, 323.0428371773161871 ) ) ;
#32359 = DIRECTION ( 'NONE',  ( 0.000000000000000000, 0.000000000000000000, 1.000000000000000000 ) ) ;
#32360 = CARTESIAN_POINT ( 'NONE',  ( 766.9102291470427417, -162.5545181178802352, 318.6633372737382501 ) ) ;
#32361 = CARTESIAN_POINT ( 'NONE',  ( 788.7366044899766848, -35.90732993114770011, 316.5762568750059813 ) ) ;
#32362 = ORIENTED_EDGE ( 'NONE', *, *, #31077, .T. ) ;
#32363 = CARTESIAN_POINT ( 'NONE',  ( 745.1792804349281596, -398.1908817542431507, -343.7566961878542884 ) ) ;
#32364 = EDGE_CURVE ( 'NONE', #43290, #7811, #15004, .T. ) ;
#32365 = CARTESIAN_POINT ( 'NONE',  ( 814.5518280994195948, 8.274488250670337663, -332.4837098697145166 ) ) ;
#32366 = CARTESIAN_POINT ( 'NONE',  ( 778.7629533639073998, -272.7363362996981095, 375.0009284576466371 ) ) ;
#32367 = CARTESIAN_POINT ( 'NONE',  ( 772.3691319403857278, -215.2601417444141987, 315.8894580844506663 ) ) ;
#32368 = ADVANCED_FACE ( 'NONE', ( #20042, #26295 ), #15899, .T. ) ;
#32369 = CARTESIAN_POINT ( 'NONE',  ( 801.9419747391806368, -354.4527844766012095, -351.9812246680014027 ) ) ;
#32370 = LINE ( 'NONE', #8122, #38619 ) ;
#32371 = EDGE_CURVE ( 'NONE', #27126, #15586, #20358, .T. ) ;
#32372 = CARTESIAN_POINT ( 'NONE',  ( 788.7366044899766848, 12.09267006885214180, 316.5762568750059813 ) ) ;
#32373 = PLANE ( 'NONE',  #38470 ) ;
#32374 = CARTESIAN_POINT ( 'NONE',  ( 786.5483106153019435, -271.6454272087889876, -364.1601925771022366 ) ) ;
#32375 = EDGE_CURVE ( 'NONE', #7404, #69, #29986, .T. ) ;
#32376 = CARTESIAN_POINT ( 'NONE',  ( 745.0891759886404770, -4.270966294784170003, 342.4968714119734159 ) ) ;
#32377 = CARTESIAN_POINT ( 'NONE',  ( 792.2312462859673587, -107.9073299311474727, 307.2067596250082602 ) ) ;
#32378 = DIRECTION ( 'NONE',  ( 1.000000000000000000, 0.000000000000000000, -0.000000000000000000 ) ) ;
#32379 = CARTESIAN_POINT ( 'NONE',  ( -786.4999999999993179, 26.27639943461401018, 900.0000000000001137 ) ) ;
#32380 = CYLINDRICAL_SURFACE ( 'NONE', #23895, 6.118999999999985562 ) ;
#32381 = AXIS2_PLACEMENT_3D ( 'NONE', #3860, #17950, #32020 ) ;
#32382 = CARTESIAN_POINT ( 'NONE',  ( 745.1792804349281596, -374.1908817542432075, 343.7566961878542884 ) ) ;
#32383 = CARTESIAN_POINT ( 'NONE',  ( 779.9999999999992042, 166.4563064324884465, -350.0000000000000000 ) ) ;
#32384 = CARTESIAN_POINT ( 'NONE',  ( 763.0537975583475827, -336.4527844766012095, 371.0346526505627480 ) ) ;
#32385 = CARTESIAN_POINT ( 'NONE',  ( 749.2812353651451076, -78.45278447660211896, -323.2262854647983090 ) ) ;
#32386 = EDGE_CURVE ( 'NONE', #11665, #35548, #41077, .T. ) ;
#32387 = CARTESIAN_POINT ( 'NONE',  ( 797.6776695296629214, -307.5436935675104451, -357.6776695296636603 ) ) ;
#32388 = DIRECTION ( 'NONE',  ( 1.000000000000000000, 0.000000000000000000, 0.000000000000000000 ) ) ;
#32389 = CARTESIAN_POINT ( 'NONE',  ( 758.0580252608178853, -414.4527844766010389, 328.0187753319985404 ) ) ;
#32390 = CARTESIAN_POINT ( 'NONE',  ( 758.4439275373578084, -180.5545181178801499, 353.2243759319684386 ) ) ;
#32391 = CARTESIAN_POINT ( 'NONE',  ( 744.6391490659812007, -62.73633629969871350, -338.7502325331110455 ) ) ;
#32392 = CARTESIAN_POINT ( 'NONE',  ( 799.4546378042377910, -81.07832356259649487, -356.1575198192848006 ) ) ;
#32393 = CARTESIAN_POINT ( 'NONE',  ( 766.5853460496234675, -109.9874144716873019, 372.3518521366060554 ) ) ;
#32394 = CARTESIAN_POINT ( 'NONE',  ( 756.3353852180820240, -413.9073299311465348, 331.1735550268787733 ) ) ;
#32395 =( BOUNDED_CURVE ( )  B_SPLINE_CURVE ( 3, ( #19059, #36373, #1697, #37273 ),
 .UNSPECIFIED., .F., .T. ) 
 B_SPLINE_CURVE_WITH_KNOTS ( ( 4, 4 ),
 ( 1.570796326794896558, 3.141592653589793116 ),
 .UNSPECIFIED. ) 
 CURVE ( )  GEOMETRIC_REPRESENTATION_ITEM ( )  RATIONAL_B_SPLINE_CURVE ( ( 1.000000000000000000, 0.8047378541243649375, 0.8047378541243649375, 1.000000000000000000 ) ) 
 REPRESENTATION_ITEM ( '' )  );
#32396 = CARTESIAN_POINT ( 'NONE',  ( 781.2497674668890113, -156.3510508353235480, 375.3608509340180603 ) ) ;
#32397 = CARTESIAN_POINT ( 'NONE',  ( 803.6646147819161570, 6.092670068852159559, -348.8264449731210561 ) ) ;
#32399 = ORIENTED_EDGE ( 'NONE', *, *, #10302, .T. ) ;
#32398 = CARTESIAN_POINT ( 'NONE',  ( 761.2382568024794409, -111.6237781080509279, -356.9571628226838129 ) ) ;
#32400 = CARTESIAN_POINT ( 'NONE',  ( 759.7806653035534055, -102.9982390220565520, -324.8639956371180801 ) ) ;
#32401 = CARTESIAN_POINT ( 'NONE',  ( 764.0069404352550464, -399.0783235625955285, -359.2566176426627180 ) ) ;
#32403 = CARTESIAN_POINT ( 'NONE',  ( 762.1405469898973024, -217.5436935675107293, 357.8594530101016176 ) ) ;
#32402 = CARTESIAN_POINT ( 'NONE',  ( 759.7806653035534055, -246.9982390220560546, 324.8639956371180801 ) ) ;
#32404 = CARTESIAN_POINT ( 'NONE',  ( 800.1688906516307043, -442.1692326535044231, -369.0717654672308186 ) ) ;
#32405 = DIRECTION ( 'NONE',  ( -0.000000000000000000, 0.000000000000000000, 1.000000000000000000 ) ) ;
#32406 = VERTEX_POINT ( 'NONE', #5492 ) ;
#32407 = CARTESIAN_POINT ( 'NONE',  ( 754.8072714833581358, -436.8164208402372992, 338.1981804954720587 ) ) ;
#32408 = ORIENTED_EDGE ( 'NONE', *, *, #14716, .F. ) ;
#32409 = CARTESIAN_POINT ( 'NONE',  ( 745.0891759886404770, -172.2709662947836478, 342.4968714119734159 ) ) ;
#32410 = CARTESIAN_POINT ( 'NONE',  ( 773.4516893846965786, -259.6454272087890445, 315.8398074228977066 ) ) ;
#32411 = VERTEX_POINT ( 'NONE', #26737 ) ;
#32412 = CARTESIAN_POINT ( 'NONE',  ( 798.5707757039680246, -77.46360902697138329, -356.7845633553585003 ) ) ;
#32413 = CARTESIAN_POINT ( 'NONE',  ( 746.7653713866222915, -233.2601417444141987, 351.0478386215610271 ) ) ;
#32414 = CARTESIAN_POINT ( 'NONE',  ( 805.1927285166399315, -232.8164208402379529, -341.8018195045277707 ) ) ;
#32415 = ORIENTED_EDGE ( 'NONE', *, *, #29809, .F. ) ;
#32416 = VECTOR ( 'NONE', #13179, 1000.000000000000000 ) ;
#32417 = CARTESIAN_POINT ( 'NONE',  ( 774.6312213355099630, -383.3618753856921444, -364.6798772138717482 ) ) ;
#32418 = CARTESIAN_POINT ( 'NONE',  ( 778.2165204200184689, -46.81642084023858530, -364.9363028652563230 ) ) ;
#32419 = CARTESIAN_POINT ( 'NONE',  ( 759.2295555964440155, -256.1692326535049915, 353.9708237608231229 ) ) ;
#32420 = DIRECTION ( 'NONE',  ( -1.880165489482579047E-16, -1.000000000000000000, -0.000000000000000000 ) ) ;
#32421 = CARTESIAN_POINT ( 'NONE',  ( 879.9999999999992042, 239.9999999999998863, -244.9999999999999716 ) ) ;
#32422 = CARTESIAN_POINT ( 'NONE',  ( 767.8955696845333705, -24.45278447660229304, -362.1676090361162323 ) ) ;
#32423 = DIRECTION ( 'NONE',  ( -0.000000000000000000, 1.000000000000000000, -0.000000000000000000 ) ) ;
#32424 = CARTESIAN_POINT ( 'NONE',  ( 939.9999999999993179, -190.2822455671962985, 69.00746428064724114 ) ) ;
#32425 = ORIENTED_EDGE ( 'NONE', *, *, #20172, .T. ) ;
#32426 = CARTESIAN_POINT ( 'NONE',  ( 802.2119215644370342, -318.0090635724251911, -367.5423716828165084 ) ) ;
#32427 = CARTESIAN_POINT ( 'NONE',  ( 744.6391490659812007, -158.7363362996984222, 338.7502325331110455 ) ) ;
#32429 = CARTESIAN_POINT ( 'NONE',  ( 762.1405469898971887, -265.5436935675106156, -357.8594530101015607 ) ) ;
#32428 = FACE_OUTER_BOUND ( 'NONE', #39244, .T. ) ;
#32430 = CARTESIAN_POINT ( 'NONE',  ( 959.5497976682736407, 120.6654763175833693, 350.0000000000000000 ) ) ;
#32431 = CARTESIAN_POINT ( 'NONE',  ( 754.7162404726377645, -110.7363362996985501, -339.4709603349214717 ) ) ;
#32432 = CARTESIAN_POINT ( 'NONE',  ( 777.4774526936600978, -10.27096629478414691, 304.7301800767027657 ) ) ;
#32433 = CARTESIAN_POINT ( 'NONE',  ( -200.7583438952258916, 294.6698570112193920, -274.9999999999999432 ) ) ;
#32434 = CARTESIAN_POINT ( 'NONE',  ( 751.2241431872005251, -16.16923265350578021, -359.9636004259367610 ) ) ;
#32435 = CARTESIAN_POINT ( 'NONE',  ( 782.5225473063383106, -334.2709662947830793, -375.2698199232970637 ) ) ;
#32436 = CARTESIAN_POINT ( 'NONE',  ( -190.7583438952259485, 394.6698570112193920, -274.9999999999999432 ) ) ;
#32437 = CARTESIAN_POINT ( 'NONE',  ( 754.8072714833581358, -4.816420840238714085, 338.1981804954720587 ) ) ;
#32438 = CARTESIAN_POINT ( 'NONE',  ( 746.4236121716829757, -279.8272453906071746, 328.8385539511384650 ) ) ;
#32439 = CARTESIAN_POINT ( 'NONE',  ( 805.9055244015594326, -195.6237781080506863, -315.8990559732753240 ) ) ;
#32440 = CARTESIAN_POINT ( 'NONE',  ( 782.5225473063381969, -238.2709662947833920, 375.2698199232970637 ) ) ;
#32441 = CARTESIAN_POINT ( 'NONE',  ( 808.0189434323515343, 9.910851887033969021, -319.0252816721025511 ) ) ;
#32442 = FACE_OUTER_BOUND ( 'NONE', #11782, .T. ) ;
#32443 = VERTEX_POINT ( 'NONE', #27211 ) ;
#32444 = CARTESIAN_POINT ( 'NONE',  ( 788.7366044899766848, -323.9073299311468190, 316.5762568750059813 ) ) ;
#32445 = CARTESIAN_POINT ( 'NONE',  ( 804.4086373105744769, -73.64542720878957027, 333.3843516231986541 ) ) ;
#32446 = CARTESIAN_POINT ( 'NONE',  ( 790.8726784830453198, 13.28531280103958423, -362.5472867521010585 ) ) ;
#32447 = CARTESIAN_POINT ( 'NONE',  ( 919.9999999999993179, 219.9999999999998863, 360.0000000000000000 ) ) ;
#32448 = DIRECTION ( 'NONE',  ( 0.000000000000000000, 0.000000000000000000, 1.000000000000000000 ) ) ;
#32450 = CARTESIAN_POINT ( 'NONE',  ( 788.7366044899766848, -371.9073299311465917, 316.5762568750059813 ) ) ;
#32449 = CARTESIAN_POINT ( 'NONE',  ( 800.7704444035546203, -148.1692326535053610, 326.0291762391768771 ) ) ;
#32451 = VERTEX_POINT ( 'NONE', #19587 ) ;
#32452 = CARTESIAN_POINT ( 'NONE',  ( 804.9511171171677688, -293.8055962898685607, -335.8780910478229202 ) ) ;
#32453 = CARTESIAN_POINT ( 'NONE',  ( 773.7943932421234194, -311.8055962898685038, -305.5313806188329409 ) ) ;
#32454 = DIRECTION ( 'NONE',  ( 0.000000000000000000, -1.000000000000000000, 0.000000000000000000 ) ) ;
#32455 = CARTESIAN_POINT ( 'NONE',  ( 815.2698199232961542, 7.183579159761247723, 342.5225473063383106 ) ) ;
#32456 = ORIENTED_EDGE ( 'NONE', *, *, #38309, .T. ) ;
#32457 = CARTESIAN_POINT ( 'NONE',  ( 757.8323909638827445, -338.6346026584195101, 352.1044303154654358 ) ) ;
#32458 = CARTESIAN_POINT ( 'NONE',  ( 779.4709603349208464, -72.35105083532378956, -314.7162404726379918 ) ) ;
#32459 = CARTESIAN_POINT ( 'NONE',  ( 759.9864689768902508, -434.0891481129646081, 354.9819416627836404 ) ) ;
#32460 = CARTESIAN_POINT ( 'NONE',  ( 796.9462024416508257, -156.4527844766018916, -308.9653473494370246 ) ) ;
#32461 = ORIENTED_EDGE ( 'NONE', *, *, #6908, .F. ) ;
#32462 = CARTESIAN_POINT ( 'NONE',  ( 794.9819416627830151, -156.9982390220564241, -319.9864689768909898 ) ) ;
#32463 = ORIENTED_EDGE ( 'NONE', *, *, #34849, .T. ) ;
#32464 = CARTESIAN_POINT ( 'NONE',  ( 772.4468031744293057, -441.8272453906066630, -363.8651313633793620 ) ) ;
#32465 = CARTESIAN_POINT ( 'NONE',  ( 768.0187753319979720, 15.36539734157940629, 318.0580252608186242 ) ) ;
#32466 = CARTESIAN_POINT ( 'NONE',  ( 805.0032342141412300, -229.5436935675106440, 314.9967657858571783 ) ) ;
#32467 = CARTESIAN_POINT ( 'NONE',  ( 802.7791456095903868, -124.7146871989599930, 329.0155153010375102 ) ) ;
#32470 = CARTESIAN_POINT ( 'NONE',  ( 791.1614460488616487, -395.2601417444136587, 373.5763878283158874 ) ) ;
#32469 = DIRECTION ( 'NONE',  ( 8.659560562354807133E-17, 0.7071067811865578978, -0.7071067811865372477 ) ) ;
#32468 = CARTESIAN_POINT ( 'NONE',  ( 799.9999999999993179, -462.9681489794448339, 370.0000000000000568 ) ) ;
#32471 = EDGE_LOOP ( 'NONE', ( #36197, #11781 ) ) ;
#32472 = CARTESIAN_POINT ( 'NONE',  ( 759.0159684113467620, -376.9181544815159555, -325.8855110935213020 ) ) ;
#32473 = DIRECTION ( 'NONE',  ( 0.7071067811857625340, 0.000000000000000000, 0.7071067811873326114 ) ) ;
#32474 = CARTESIAN_POINT ( 'NONE',  ( 745.1792804349281596, -158.1908817542438612, -343.7566961878542884 ) ) ;
#32475 = CARTESIAN_POINT ( 'NONE',  ( 745.7194118038753459, -85.64542720878952764, 348.7631598425976449 ) ) ;
#32477 = DIRECTION ( 'NONE',  ( 0.000000000000000000, -0.7651688349527138167, 0.6438296778008192334 ) ) ;
#32476 = DIRECTION ( 'NONE',  ( -1.000000000000000000, -0.000000000000000000, -0.000000000000000000 ) ) ;
#32478 = CARTESIAN_POINT ( 'NONE',  ( 786.6156483768007774, -313.4419599262320730, -315.5913626894246136 ) ) ;
#32479 = DIRECTION ( 'NONE',  ( -0.000000000000000000, 1.000000000000000000, -0.000000000000000000 ) ) ;
#32480 = CARTESIAN_POINT ( 'NONE',  ( 778.7629533639073998, -176.7363362996983369, -375.0009284576466371 ) ) ;
#32481 = DIRECTION ( 'NONE',  ( -0.000000000000000000, -0.000000000000000000, 1.000000000000000000 ) ) ;
#32482 = DIRECTION ( 'NONE',  ( 0.000000000000000000, 0.3826834323650838421, 0.9238795325112891810 ) ) ;
#32483 = CARTESIAN_POINT ( 'NONE',  ( 755.3028492785439312, -399.2817908451522726, 335.9200461376539693 ) ) ;
#32484 = CARTESIAN_POINT ( 'NONE',  ( 777.4774526936600978, -202.2709662947835341, -304.7301800767028226 ) ) ;
#32485 = FACE_OUTER_BOUND ( 'NONE', #12888, .T. ) ;
#32486 = CARTESIAN_POINT ( 'NONE',  ( 774.6312213355099630, 0.6381246143067236254, -364.6798772138717482 ) ) ;
#32487 = CARTESIAN_POINT ( 'NONE',  ( 760.0363995740630116, -154.9181544815165523, 368.7758568127991907 ) ) ;
#32488 = CARTESIAN_POINT ( 'NONE',  ( 756.1443688327750579, -93.62377810805098477, -314.3581564841659315 ) ) ;
#32489 = CARTESIAN_POINT ( 'NONE',  ( 763.2262854647970016, -128.6346026584201354, 309.2812353651462445 ) ) ;
#32490 = CARTESIAN_POINT ( 'NONE',  ( 808.3070685750230950, -330.9982390220558273, -361.1904061080339261 ) ) ;
#32491 = DIRECTION ( 'NONE',  ( 0.000000000000000000, 0.3826834323650836200, 0.9238795325112892920 ) ) ;
#32492 = DIRECTION ( 'NONE',  ( 1.000000000000000000, 0.000000000000000000, -0.000000000000000000 ) ) ;
#32493 = CARTESIAN_POINT ( 'NONE',  ( 785.3687786644884454, -227.3618753856925707, 315.3201227861279676 ) ) ;
#32494 = CARTESIAN_POINT ( 'NONE',  ( 796.1575198192839480, -6.009063572426154742, 359.4546378042384163 ) ) ;
#32495 = CARTESIAN_POINT ( 'NONE',  ( 800.1688906516307043, -418.1692326535044799, -369.0717654672308186 ) ) ;
#32496 = CARTESIAN_POINT ( 'NONE',  ( 787.4397851343537695, -405.7255117493283478, -374.2001403089903988 ) ) ;
#32497 = LINE ( 'NONE', #1308, #43163 ) ;
#32498 = CARTESIAN_POINT ( 'NONE',  ( 778.7502325331095108, -48.35105083532386061, 304.6391490659818828 ) ) ;
#32499 = ORIENTED_EDGE ( 'NONE', *, *, #22985, .F. ) ;
#32500 = EDGE_CURVE ( 'NONE', #20516, #2099, #30211, .T. ) ;
#32501 = CARTESIAN_POINT ( 'NONE',  ( 773.3843516231979720, -181.4419599262325278, -364.4086373105754433 ) ) ;
#32502 = CARTESIAN_POINT ( 'NONE',  ( 794.9819416627830151, -12.99823902205686821, 319.9864689768909898 ) ) ;
#32503 = CARTESIAN_POINT ( 'NONE',  ( 761.9338519418445230, -206.5328690171415360, -370.4231160770881957 ) ) ;
#32504 = SURFACE_SIDE_STYLE ('',( #11034 ) ) ;
#32505 = CARTESIAN_POINT ( 'NONE',  ( 803.8556311672234642, -345.6237781080501463, 365.6418435158340117 ) ) ;
#32506 = CARTESIAN_POINT ( 'NONE',  ( 771.1735550268780344, -153.1800572038746111, 316.3353852180828198 ) ) ;
#32507 = ORIENTED_EDGE ( 'NONE', *, *, #6355, .F. ) ;
#32508 = CARTESIAN_POINT ( 'NONE',  ( 804.6798772138708955, -135.7255117493291152, -334.6312213355107019 ) ) ;
#32509 = CARTESIAN_POINT ( 'NONE',  ( 758.0580252608178853, -342.4527844766013231, 328.0187753319985404 ) ) ;
#32510 = CARTESIAN_POINT ( 'NONE',  ( 772.4837098697144029, -47.36187538569312494, -374.5518280994205611 ) ) ;
#32511 = VERTEX_POINT ( 'NONE', #1792 ) ;
#32512 = CARTESIAN_POINT ( 'NONE',  ( 799.9636004259356241, -454.9181544815156713, -311.2241431872006956 ) ) ;
#32513 = ORIENTED_EDGE ( 'NONE', *, *, #9984, .T. ) ;
#32514 = CARTESIAN_POINT ( 'NONE',  ( 802.5472867521000353, -316.3726999360615082, -350.8726784830461156 ) ) ;
#32516 = CARTESIAN_POINT ( 'NONE',  ( 790.0220218866281812, -367.0999726633342561, 363.2186876482849129 ) ) ;
#32515 = CARTESIAN_POINT ( 'NONE',  ( 755.0636971347428243, -52.27096629478401724, 341.7834795799807353 ) ) ;
#32517 = CARTESIAN_POINT ( 'NONE',  ( 797.8594530101008786, -301.5436935675105588, -322.1405469898980982 ) ) ;
#32519 = CARTESIAN_POINT ( 'NONE',  ( 751.2241431872005251, -280.1692326535049347, 359.9636004259367610 ) ) ;
#32518 = CARTESIAN_POINT ( 'NONE',  ( 744.7301800767020268, -388.8164208402374129, 337.4774526936615189 ) ) ;
#32520 = CARTESIAN_POINT ( 'NONE',  ( 778.7502325331095108, -72.35105083532378956, 304.6391490659818828 ) ) ;
#32521 = CARTESIAN_POINT ( 'NONE',  ( 754.7162404726377645, -302.7363362996979959, -339.4709603349214717 ) ) ;
#32522 = CARTESIAN_POINT ( 'NONE',  ( 756.5762568750052424, -291.1800572038741848, -348.7366044899774238 ) ) ;
#32523 = FACE_OUTER_BOUND ( 'NONE', #10390, .T. ) ;
#32524 = CARTESIAN_POINT ( 'NONE',  ( 797.8594530101008786, -109.5436935675110988, -322.1405469898980982 ) ) ;
#32525 = EDGE_CURVE ( 'NONE', #21185, #12675, #5952, .T. ) ;
#32526 = LINE ( 'NONE', #25121, #25465 ) ;
#32527 = VERTEX_POINT ( 'NONE', #44072 ) ;
#32528 = CARTESIAN_POINT ( 'NONE',  ( 800.9747183278959710, -420.9982390220555999, 311.9810565676471583 ) ) ;
#32530 = DIRECTION ( 'NONE',  ( -0.000000000000000000, 1.000000000000000000, -0.000000000000000000 ) ) ;
#32529 = CARTESIAN_POINT ( 'NONE',  ( 759.9999999999992042, -462.9681489794448339, -309.9999999999998863 ) ) ;
#32531 = CARTESIAN_POINT ( 'NONE',  ( 766.4474001241216001, -67.09997266333506616, -307.3154664389482491 ) ) ;
#32532 = DIRECTION ( 'NONE',  ( -0.000000000000000000, 1.000000000000000000, -0.000000000000000000 ) ) ;
#32533 = DIRECTION ( 'NONE',  ( 0.7071067811857625340, 0.000000000000000000, -0.7071067811873326114 ) ) ;
#32534 = EDGE_CURVE ( 'NONE', #33435, #35726, #2032, .T. ) ;
#32535 = CARTESIAN_POINT ( 'NONE',  ( 804.8461984189677878, -266.1908817542435486, 336.9566956441385628 ) ) ;
#32536 = CARTESIAN_POINT ( 'NONE',  ( 757.8323909638827445, -146.6346026584200217, 352.1044303154654358 ) ) ;
#32537 = ORIENTED_EDGE ( 'NONE', *, *, #22626, .F. ) ;
#32538 = CARTESIAN_POINT ( 'NONE',  ( 767.7687537140311633, -95.90732993114751537, -372.7932403749916830 ) ) ;
#32539 = CARTESIAN_POINT ( 'NONE',  ( 799.4546378042377910, -321.0783235625956991, 356.1575198192848006 ) ) ;
#32540 = CYLINDRICAL_SURFACE ( 'NONE', #7182, 2.749999999999863665 ) ;
#32541 = CARTESIAN_POINT ( 'NONE',  ( 805.6418435158337843, -29.46360902697153250, 363.8556311672236916 ) ) ;
#32542 = CARTESIAN_POINT ( 'NONE',  ( 796.7737145352015204, -236.6346026584198228, -370.7187646348536987 ) ) ;
#32543 = CARTESIAN_POINT ( 'NONE',  ( 763.2262854647970016, -200.6346026584199365, 309.2812353651462445 ) ) ;
#32544 = CARTESIAN_POINT ( 'NONE',  ( 757.8323909638827445, -98.63460265842024910, 352.1044303154654358 ) ) ;
#32545 = DIRECTION ( 'NONE',  ( -0.000000000000000000, 1.000000000000000000, -0.000000000000000000 ) ) ;
#32546 = CARTESIAN_POINT ( 'NONE',  ( 808.7758568127978833, -316.1692326535048210, -320.0363995740631822 ) ) ;
#32547 = CARTESIAN_POINT ( 'NONE',  ( 809.0717654672305343, -436.9181544815157281, 360.1688906516309885 ) ) ;
#32548 = CARTESIAN_POINT ( 'NONE',  ( 759.0252816721024374, -312.9982390220559409, -368.0189434323527280 ) ) ;
#32549 = CARTESIAN_POINT ( 'NONE',  ( 999.9999999999992042, -600.0000000000001137, -359.0000000000000000 ) ) ;
#32550 = CARTESIAN_POINT ( 'NONE',  ( 754.8983024940795303, -402.8965053807773415, 336.9254006560228163 ) ) ;
#32551 = ORIENTED_EDGE ( 'NONE', *, *, #27506, .T. ) ;
#32552 = DIRECTION ( 'NONE',  ( 0.000000000000000000, 0.000000000000000000, 1.000000000000000000 ) ) ;
#32553 = CARTESIAN_POINT ( 'NONE',  ( 757.8323909638827445, -410.6346026584191122, -352.1044303154654358 ) ) ;
#32554 = CARTESIAN_POINT ( 'NONE',  ( 790.8726784830453198, -58.71468719896019905, 362.5472867521010585 ) ) ;
#32555 = CARTESIAN_POINT ( 'NONE',  ( 774.6312213355099630, -215.3618753856925423, -364.6798772138717482 ) ) ;
#32556 = CARTESIAN_POINT ( 'NONE',  ( 781.2497674668890113, -84.35105083532374692, -375.3608509340180603 ) ) ;
#32557 = DIRECTION ( 'NONE',  ( 0.000000000000000000, -0.3826834323650836756, -0.9238795325112892920 ) ) ;
#32558 = CARTESIAN_POINT ( 'NONE',  ( 744.9990715423526808, -210.3510508353233490, 341.2370466360926002 ) ) ;
#32559 = CARTESIAN_POINT ( 'NONE',  ( 759.7806653035535192, -54.99823902205672965, 324.8639956371181370 ) ) ;
#32560 = ORIENTED_EDGE ( 'NONE', *, *, #35350, .F. ) ;
#32561 = CARTESIAN_POINT ( 'NONE',  ( 757.2208543904082489, -232.7146871989596377, -350.9844846989624330 ) ) ;
#32562 = CARTESIAN_POINT ( 'NONE',  ( 764.8639956371174549, -248.0891481129651481, 319.7806653035542013 ) ) ;
#32563 = CARTESIAN_POINT ( 'NONE',  ( 814.8230680027162407, -53.80559628986930676, -333.7305795820267917 ) ) ;
#32564 = CARTESIAN_POINT ( 'NONE',  ( 804.9363028652555840, -352.2709662947830225, 338.2165204200192079 ) ) ;
#32565 = CARTESIAN_POINT ( 'NONE',  ( 989.9999999999992042, 249.9999999999998863, -209.9999999999999716 ) ) ;
#32566 = ORIENTED_EDGE ( 'NONE', *, *, #31216, .T. ) ;
#32567 = CARTESIAN_POINT ( 'NONE',  ( 748.6759233522253680, -352.3726999360614514, -324.3348316497537098 ) ) ;
#32568 = CARTESIAN_POINT ( 'NONE',  ( 782.5225473063383106, -286.2709662947833067, 375.2698199232970637 ) ) ;
#32569 = EDGE_CURVE ( 'NONE', #40061, #18319, #16681, .T. ) ;
#32570 = CARTESIAN_POINT ( 'NONE',  ( 771.2368401574024119, -13.44195992623305713, 374.2805881961240857 ) ) ;
#32571 = APPLICATION_CONTEXT ( 'automotive_design' ) ;
#32572 = CARTESIAN_POINT ( 'NONE',  ( 793.0897708529556667, -174.5545181178801784, -361.3366627262616362 ) ) ;
#32573 = CARTESIAN_POINT ( 'NONE',  ( 759.9864689768902508, -194.0891481129654039, -354.9819416627836404 ) ) ;
#32574 = VECTOR ( 'NONE', #21501, 1000.000000000000000 ) ;
#32575 = CARTESIAN_POINT ( 'NONE',  ( 759.7806653035535192, -390.9982390220556567, -324.8639956371181370 ) ) ;
#32576 = VERTEX_POINT ( 'NONE', #20271 ) ;
#32577 = CARTESIAN_POINT ( 'NONE',  ( 769.1273215169530886, 25.28531280103955226, -317.4527132478988847 ) ) ;
#32578 = VERTEX_POINT ( 'NONE', #12657 ) ;
#32579 = CARTESIAN_POINT ( 'NONE',  ( 772.5602148656447525, -273.7255117493288026, 305.7998596910095443 ) ) ;
#32580 = DIRECTION ( 'NONE',  ( 0.000000000000000000, -1.000000000000000000, 0.000000000000000000 ) ) ;
#32581 = CARTESIAN_POINT ( 'NONE',  ( 754.9735926884551418, -354.3510508353228943, 340.5236548041000333 ) ) ;
#32582 = CYLINDRICAL_SURFACE ( 'NONE', #41810, 2.749999999999863665 ) ;
#32583 = ADVANCED_FACE ( 'NONE', ( #40407 ), #44775, .F. ) ;
#32584 = CARTESIAN_POINT ( 'NONE',  ( 772.4468031744293057, -153.8272453906075157, 363.8651313633793620 ) ) ;
#32585 = CARTESIAN_POINT ( 'NONE',  ( 785.3687786644884454, -35.36187538569316047, 315.3201227861279676 ) ) ;
#32586 = ORIENTED_EDGE ( 'NONE', *, *, #28336, .F. ) ;
#32587 = CARTESIAN_POINT ( 'NONE',  ( 764.1737431748507561, -418.3726999360612808, -371.6461892240376415 ) ) ;
#32588 = CARTESIAN_POINT ( 'NONE',  ( 813.1304606946831655, 6.092670068852160448, -352.3570229623691716 ) ) ;
#32589 = CARTESIAN_POINT ( 'NONE',  ( 813.5763878283155464, -267.8272453906071746, 351.1614460488615350 ) ) ;
#32590 = CARTESIAN_POINT ( 'NONE',  ( 770.0799878456142551, -205.9874144716870035, 362.9823548866085616 ) ) ;
#32591 = CARTESIAN_POINT ( 'NONE',  ( 774.6858677611749044, -369.7255117493284615, -315.5713283507209894 ) ) ;
#32592 = LINE ( 'NONE', #18512, #32728 ) ;
#32593 = CARTESIAN_POINT ( 'NONE',  ( 755.5713283507202505, -5.361875385693257279, 334.6858677611754729 ) ) ;
#32594 = CARTESIAN_POINT ( 'NONE',  ( 914.9999999999992042, 74.99999999999984368, -360.0000000000000000 ) ) ;
#32595 = CARTESIAN_POINT ( 'NONE',  ( 760.7433823573367135, -252.0090635724254184, -355.9930595647440441 ) ) ;
#32596 = CARTESIAN_POINT ( 'NONE',  ( 792.3570229623688874, -45.18005720387493085, 373.1304606946836202 ) ) ;
#32597 = CARTESIAN_POINT ( 'NONE',  ( 777.4774526936600978, -106.2709662947838467, 304.7301800767027657 ) ) ;
#32598 = DIRECTION ( 'NONE',  ( 4.625929269271485914E-16, -1.000000000000000000, 0.000000000000000000 ) ) ;
#32599 = DIRECTION ( 'NONE',  ( 0.000000000000000000, -0.6594541114781790059, 0.7517448203044204691 ) ) ;
#32600 = EDGE_CURVE ( 'NONE', #16943, #9876, #18902, .T. ) ;
#32601 = CARTESIAN_POINT ( 'NONE',  ( 809.0717654672305343, -388.9181544815158986, 360.1688906516309885 ) ) ;
#32602 = ADVANCED_FACE ( 'NONE', ( #37376 ), #16354, .F. ) ;
#32603 = DIRECTION ( 'NONE',  ( 1.000000000000000000, 0.000000000000000000, 0.000000000000000000 ) ) ;
#32604 = CARTESIAN_POINT ( 'NONE',  ( 763.2262854647970016, -320.6346026584195670, 309.2812353651462445 ) ) ;
#32605 = CARTESIAN_POINT ( 'NONE',  ( 778.2165204200184689, -334.8164208402376403, -364.9363028652563230 ) ) ;
#32606 = CARTESIAN_POINT ( 'NONE',  ( 311.1634899080286232, 260.0000000000000000, -197.2499999999964473 ) ) ;
#32607 = CARTESIAN_POINT ( 'NONE',  ( 774.6312213355099630, -431.3618753856918033, 364.6798772138717482 ) ) ;
#32608 =( GEOMETRIC_REPRESENTATION_CONTEXT ( 3 ) GLOBAL_UNCERTAINTY_ASSIGNED_CONTEXT ( ( #37024 ) ) GLOBAL_UNIT_ASSIGNED_CONTEXT ( ( #32820, #15041, #35826 ) ) REPRESENTATION_CONTEXT ( 'NONE', 'WORKASPACE' ) );
#32609 = CARTESIAN_POINT ( 'NONE',  ( 758.4439275373578084, -204.5545181178800931, 353.2243759319684386 ) ) ;
#32610 = CARTESIAN_POINT ( 'NONE',  ( 786.2694204179717872, -69.28179084515321051, -305.1769319972829067 ) ) ;
#32611 = CARTESIAN_POINT ( 'NONE',  ( 773.3843516231979720, -109.4419599262327836, -364.4086373105754433 ) ) ;
#32612 = CARTESIAN_POINT ( 'NONE',  ( 759.8311093483677041, -118.1692326535054463, 310.9282345327691814 ) ) ;
#32613 = CARTESIAN_POINT ( 'NONE',  ( 781.8018195045267476, -430.2709662947827383, 365.1927285166407273 ) ) ;
#32614 = CARTESIAN_POINT ( 'NONE',  ( 764.8639956371174549, 15.91085188703394238, -319.7806653035542013 ) ) ;
#32616 = EDGE_LOOP ( 'NONE', ( #3978, #12962, #18610, #32274 ) ) ;
#32615 = CARTESIAN_POINT ( 'NONE',  ( 795.9930595647434757, -147.0783235625962959, -320.7433823573372820 ) ) ;
#32617 = CARTESIAN_POINT ( 'NONE',  ( 803.4237431249931660, -111.1800572038747532, -331.2633955100225194 ) ) ;
#32618 = CARTESIAN_POINT ( 'NONE',  ( 804.9511171171677688, -389.8055962898682765, -335.8780910478229202 ) ) ;
#32620 = CARTESIAN_POINT ( 'NONE',  ( 804.6798772138710092, -255.7255117493287742, 334.6312213355106451 ) ) ;
#32619 = CARTESIAN_POINT ( 'NONE',  ( 762.1405469898971887, -265.5436935675106156, 357.8594530101015607 ) ) ;
#32621 = DIRECTION ( 'NONE',  ( -1.000000000000000000, -0.000000000000000000, 0.000000000000000000 ) ) ;
#32622 = ORIENTED_EDGE ( 'NONE', *, *, #35975, .F. ) ;
#32623 = CARTESIAN_POINT ( 'NONE',  ( 755.3201227861273992, -435.7255117493282341, 345.3687786644892981 ) ) ;
#32624 = EDGE_CURVE ( 'NONE', #42970, #14331, #9656, .T. ) ;
#32625 = EDGE_LOOP ( 'NONE', ( #23284, #34928 ) ) ;
#32626 = CARTESIAN_POINT ( 'NONE',  ( 801.1904061080338124, -188.0891481129653755, 368.3070685750236066 ) ) ;
#32627 = EDGE_CURVE ( 'NONE', #35816, #22668, #9433, .T. ) ;
#32628 = CARTESIAN_POINT ( 'NONE',  ( 772.4468031744293057, -249.8272453906072315, 363.8651313633793620 ) ) ;
#32629 = CARTESIAN_POINT ( 'NONE',  ( 761.2382568024794409, -375.6237781080501463, 356.9571628226838129 ) ) ;
#32630 = EDGE_LOOP ( 'NONE', ( #25294, #34621, #32551, #34777 ) ) ;
#32631 = CARTESIAN_POINT ( 'NONE',  ( 779.4763451958990572, -80.73633629969864955, -365.0264073115438919 ) ) ;
#32632 = CARTESIAN_POINT ( 'NONE',  ( 746.0683387631852383, -211.4419599262324709, 331.3260364891676204 ) ) ;
#32633 = CARTESIAN_POINT ( 'NONE',  ( 805.1927285166399315, -256.8164208402379245, -341.8018195045277707 ) ) ;
#32634 = EDGE_LOOP ( 'NONE', ( #13829, #28923, #7892, #29662 ) ) ;
#32635 = CARTESIAN_POINT ( 'NONE',  ( 785.3141322388236176, -381.7255117493284615, -364.4286716492789537 ) ) ;
#32636 = CARTESIAN_POINT ( 'NONE',  ( 781.8018195045266339, -46.27096629478404566, -365.1927285166406705 ) ) ;
#32637 = CARTESIAN_POINT ( 'NONE',  ( 769.1273215169530886, -262.7146871989594956, 317.4527132478988847 ) ) ;
#32638 = EDGE_CURVE ( 'NONE', #19609, #3824, #30434, .T. ) ;
#32639 = LINE ( 'NONE', #4249, #14511 ) ;
#32640 = CARTESIAN_POINT ( 'NONE',  ( 115.7583438952258774, 430.0000000000002842, -244.9999999999999716 ) ) ;
#32641 = EDGE_CURVE ( 'NONE', #346, #35075, #37831, .T. ) ;
#32642 = CARTESIAN_POINT ( 'NONE',  ( 765.0180583372156207, -24.99823902205683268, -360.0135310231089534 ) ) ;
#32643 = CYLINDRICAL_SURFACE ( 'NONE', #31397, 2.749999999999863665 ) ;
#32644 = VERTEX_POINT ( 'NONE', #12216 ) ;
#32645 = CARTESIAN_POINT ( 'NONE',  ( 755.8990559732751535, -299.4636090269707438, -365.9055244015606831 ) ) ;
#32646 = AXIS2_PLACEMENT_3D ( 'NONE', #44686, #26216, #13044 ) ;
#32647 = CARTESIAN_POINT ( 'NONE',  ( 745.7194118038753459, -157.6454272087893287, 348.7631598425976449 ) ) ;
#32649 = CARTESIAN_POINT ( 'NONE',  ( 771.1735550268778070, -249.1800572038742416, -316.3353852180827630 ) ) ;
#32648 = DIRECTION ( 'NONE',  ( 0.000000000000000000, 0.000000000000000000, -1.000000000000000000 ) ) ;
#32650 = FACE_OUTER_BOUND ( 'NONE', #5915, .T. ) ;
#32651 = CARTESIAN_POINT ( 'NONE',  ( 755.1538015810308480, -158.1908817542438612, -343.0433043558613804 ) ) ;
#32652 = MANIFOLD_SOLID_BREP ( 'Boss-Extrude21', #7734 ) ;
#32653 = CARTESIAN_POINT ( 'NONE',  ( 763.2262854647970016, -8.634602658420517329, 309.2812353651462445 ) ) ;
#32654 = CARTESIAN_POINT ( 'NONE',  ( -338.8365100919713200, 260.0000000000001137, -202.7499999999916724 ) ) ;
#32655 = CARTESIAN_POINT ( 'NONE',  ( 744.9990715423526808, -18.35105083532395298, -341.2370466360926002 ) ) ;
#32656 = CARTESIAN_POINT ( 'NONE',  ( 759.0252816721024374, -360.9982390220557704, -368.0189434323527280 ) ) ;
#32657 = DIRECTION ( 'NONE',  ( -1.337618101958019798E-16, 1.000000000000000000, -1.672022627447524747E-16 ) ) ;
#32658 = CARTESIAN_POINT ( 'NONE',  ( 765.0180583372156207, -24.99823902205683268, 360.0135310231089534 ) ) ;
#32659 = CARTESIAN_POINT ( 'NONE',  ( 745.7194118038753459, -277.6454272087889308, 348.7631598425976449 ) ) ;
#32660 = CARTESIAN_POINT ( 'NONE',  ( 814.8230680027162407, -245.8055962898686460, -333.7305795820267917 ) ) ;
#32661 = CARTESIAN_POINT ( 'NONE',  ( 751.9810565676468741, -218.0891481129653187, 360.9747183278973921 ) ) ;
#32662 = CARTESIAN_POINT ( 'NONE',  ( 763.2262854647970016, 15.36539734157940629, -309.2812353651462445 ) ) ;
#32663 = FACE_BOUND ( 'NONE', #30386, .T. ) ;
#32664 = ORIENTED_EDGE ( 'NONE', *, *, #30520, .F. ) ;
#32665 = CARTESIAN_POINT ( 'NONE',  ( 804.9363028652555840, -328.2709662947831362, 338.2165204200192079 ) ) ;
#32666 = VECTOR ( 'NONE', #13844, 1000.000000000000227 ) ;
#32667 = CARTESIAN_POINT ( 'NONE',  ( 804.1105419155481968, -99.82724539060768620, 347.6308680596136469 ) ) ;
#32668 = CARTESIAN_POINT ( 'NONE',  ( 761.2382568024794409, 8.376221891948691933, -356.9571628226838129 ) ) ;
#32669 = CARTESIAN_POINT ( 'NONE',  ( 767.9999999999992042, 205.0000000000000568, 319.9999999999999432 ) ) ;
#32670 = CARTESIAN_POINT ( 'NONE',  ( 911.9999999999993179, 154.9999999999998863, -360.0000000000000000 ) ) ;
#32672 = CARTESIAN_POINT ( 'NONE',  ( 781.8018195045266339, -358.2709662947829088, 365.1927285166406705 ) ) ;
#32671 = CARTESIAN_POINT ( 'NONE',  ( 754.9735926884551418, -162.3510508353235196, 340.5236548041000333 ) ) ;
#32673 = ORIENTED_EDGE ( 'NONE', *, *, #43384, .T. ) ;
#32674 = CARTESIAN_POINT ( 'NONE',  ( 770.0799878456142551, -301.9874144716867477, -362.9823548866085616 ) ) ;
#32675 = CARTESIAN_POINT ( 'NONE',  ( 785.3141322388236176, -141.7255117493291721, 364.4286716492789537 ) ) ;
#32676 = CARTESIAN_POINT ( 'NONE',  ( 812.6845335610512393, -343.9874144716865771, -353.5525998758768651 ) ) ;
#32677 = DIRECTION ( 'NONE',  ( 0.000000000000000000, -1.000000000000000000, 0.000000000000000000 ) ) ;
#32678 = CARTESIAN_POINT ( 'NONE',  ( 767.6429770376289525, 14.81994279612486309, 306.8695393053162093 ) ) ;
#32679 = ORIENTED_EDGE ( 'NONE', *, *, #20172, .F. ) ;
#32680 = CARTESIAN_POINT ( 'NONE',  ( 771.2633955100217236, -335.9073299311468190, 363.4237431249939618 ) ) ;
#32681 = EDGE_CURVE ( 'NONE', #37595, #31020, #22822, .T. ) ;
#32682 = CARTESIAN_POINT ( 'NONE',  ( 803.2186876482843445, -79.98741447168740137, -350.0220218866286928 ) ) ;
#32683 = VERTEX_POINT ( 'NONE', #6865 ) ;
#32684 = CARTESIAN_POINT ( 'NONE',  ( 791.9812246680005501, -452.6346026584191691, 361.9419747391813189 ) ) ;
#32685 = CARTESIAN_POINT ( 'NONE',  ( 748.9653473494363425, -146.6346026584200217, -356.9462024416521331 ) ) ;
#32686 = ORIENTED_EDGE ( 'NONE', *, *, #20200, .T. ) ;
#32687 = CARTESIAN_POINT ( 'NONE',  ( 801.9419747391806368, -138.4527844766019200, -351.9812246680014027 ) ) ;
#32688 = VERTEX_POINT ( 'NONE', #24192 ) ;
#32689 = CARTESIAN_POINT ( 'NONE',  ( 766.0291762391763086, -418.9181544815157849, -360.7704444035551319 ) ) ;
#32690 = CARTESIAN_POINT ( 'NONE',  ( 800.2193346964447755, 5.001760977943074948, 355.1360043628815788 ) ) ;
#32691 = CARTESIAN_POINT ( 'NONE',  ( 810.7187646348534145, -234.4527844766016358, 356.7737145352016341 ) ) ;
#32692 = CARTESIAN_POINT ( 'NONE',  ( 793.2243759319678702, -146.5328690171417350, 318.4439275373583200 ) ) ;
#32694 = CARTESIAN_POINT ( 'NONE',  ( -190.7583438952258916, 294.6698570112193920, -224.9999999999999716 ) ) ;
#32693 = PLANE ( 'NONE',  #16654 ) ;
#32695 = ORIENTED_EDGE ( 'NONE', *, *, #23250, .F. ) ;
#32696 = CARTESIAN_POINT ( 'NONE',  ( 755.3028492785439312, -399.2817908451522726, -335.9200461376539693 ) ) ;
#32697 = CARTESIAN_POINT ( 'NONE',  ( -598.8365100919716042, 240.0000000000001705, -197.2499999999901092 ) ) ;
#32698 = CIRCLE ( 'NONE', #13505, 2.749999999999919176 ) ;
#32699 = CARTESIAN_POINT ( 'NONE',  ( 814.8207195650702488, -218.1908817542437191, -336.2433038121456548 ) ) ;
#32700 = CARTESIAN_POINT ( 'NONE',  ( 808.3070685750230950, -162.9982390220563673, 361.1904061080339261 ) ) ;
#32701 = CARTESIAN_POINT ( 'NONE',  ( 781.2370466360911223, -68.73633629969867798, 304.9990715423533629 ) ) ;
#32703 = CARTESIAN_POINT ( 'NONE',  ( -784.4999999999993179, -513.1383975375929367, -369.9999999999999432 ) ) ;
#32702 = DIRECTION ( 'NONE',  ( -0.000000000000000000, 1.000000000000000000, -0.000000000000000000 ) ) ;
#32704 = CARTESIAN_POINT ( 'NONE',  ( 775.9200461376533440, -311.8055962898685038, -315.3028492785443291 ) ) ;
#32705 = DIRECTION ( 'NONE',  ( 0.000000000000000000, 0.000000000000000000, 1.000000000000000000 ) ) ;
#32706 = CARTESIAN_POINT ( 'NONE',  ( 811.3240766477731540, -196.3726999360619061, -355.6651683502462902 ) ) ;
#32707 = DIRECTION ( 'NONE',  ( -0.000000000000000000, 0.9235249282889856914, -0.3835384033298670503 ) ) ;
#32708 = CARTESIAN_POINT ( 'NONE',  ( 187.1337867209877857, -428.4497686941065808, 352.6378164459125060 ) ) ;
#32709 = CARTESIAN_POINT ( 'NONE',  ( 779.4763451958990572, -392.7363362996977116, 365.0264073115438919 ) ) ;
#32710 = CARTESIAN_POINT ( 'NONE',  ( 759.0252816721024374, -240.9982390220561683, -368.0189434323527280 ) ) ;
#32711 = DIRECTION ( 'NONE',  ( 1.000000000000000000, -0.000000000000000000, 0.000000000000000000 ) ) ;
#32712 = CARTESIAN_POINT ( 'NONE',  ( 781.8018195045266339, -22.27096629478410250, -365.1927285166406705 ) ) ;
#32713 = PRESENTATION_LAYER_ASSIGNMENT (  '', '', ( #40809 ) ) ;
#32714 = CARTESIAN_POINT ( 'NONE',  ( 749.5768839229115201, -180.5545181178801499, 358.0661480581553064 ) ) ;
#32715 = CARTESIAN_POINT ( 'NONE',  ( 746.0683387631852383, -115.4419599262327409, -331.3260364891676204 ) ) ;
#32716 = CARTESIAN_POINT ( 'NONE',  ( 796.9462024416508257, -132.4527844766018916, 308.9653473494370246 ) ) ;
#32717 = CARTESIAN_POINT ( 'NONE',  ( 772.4837098697144029, -359.3618753856920875, -374.5518280994205611 ) ) ;
#32718 = LINE ( 'NONE', #8696, #12854 ) ;
#32719 = DIRECTION ( 'NONE',  ( 0.000000000000000000, 0.000000000000000000, 1.000000000000000000 ) ) ;
#32720 = CARTESIAN_POINT ( 'NONE',  ( 755.0636971347428243, -220.2709662947834772, 341.7834795799807353 ) ) ;
#32721 = CARTESIAN_POINT ( 'NONE',  ( 804.6971507214547046, -27.28179084515336328, 344.0799538623459739 ) ) ;
#32722 = CARTESIAN_POINT ( 'NONE',  ( 751.2241431872005251, -400.1692326535045936, -359.9636004259367610 ) ) ;
#32723 = CARTESIAN_POINT ( 'NONE',  ( 792.2312462859673587, -443.9073299311464780, -307.2067596250082602 ) ) ;
#32724 = CARTESIAN_POINT ( 'NONE',  ( 927.9999999999992042, 219.9999999999998863, -360.0000000000000000 ) ) ;
#32725 = CARTESIAN_POINT ( 'NONE',  ( 778.7502325331095108, -24.35105083532392811, 304.6391490659818828 ) ) ;
#32726 = EDGE_LOOP ( 'NONE', ( #9103, #13190, #8099, #5622 ) ) ;
#32727 = CARTESIAN_POINT ( 'NONE',  ( 805.1016975059191054, -198.8965053807779384, -343.0745993439771837 ) ) ;
#32728 = VECTOR ( 'NONE', #3095, 1000.000000000000000 ) ;
#32729 = CARTESIAN_POINT ( 'NONE',  ( 756.3353852180819104, -29.90732993114771787, 331.1735550268788302 ) ) ;
#32730 = CARTESIAN_POINT ( 'NONE',  ( 754.0944755984390895, -207.6237781080506295, -364.1009440267246760 ) ) ;
#32731 = CARTESIAN_POINT ( 'NONE',  ( 999.5857864376259840, 249.9999999999998863, 360.0000000000000000 ) ) ;
#32732 = CARTESIAN_POINT ( 'NONE',  ( 814.8230680027162407, -341.8055962898683333, 333.7305795820267917 ) ) ;
#32733 = CARTESIAN_POINT ( 'NONE',  ( 788.8264449731201466, -165.1800572038745543, 363.6646147819170665 ) ) ;
#32734 = AXIS2_PLACEMENT_3D ( 'NONE', #24217, #5975, #17070 ) ;
#32735 = ORIENTED_EDGE ( 'NONE', *, *, #5689, .F. ) ;
#32736 = CARTESIAN_POINT ( 'NONE',  ( 803.8556311672234642, -417.6237781080499190, 365.6418435158340117 ) ) ;
#32737 = CARTESIAN_POINT ( 'NONE',  ( 781.7834795799800531, -154.8164208402382371, -315.0636971347436202 ) ) ;
#32738 = CARTESIAN_POINT ( 'NONE',  ( 788.7366044899766848, -347.9073299311467053, 316.5762568750059813 ) ) ;
#32739 = CARTESIAN_POINT ( 'NONE',  ( 812.7932403749906598, -39.18005720387496638, -327.7687537140311633 ) ) ;
#32740 = ORIENTED_EDGE ( 'NONE', *, *, #17520, .F. ) ;
#32741 = CARTESIAN_POINT ( 'NONE',  ( 791.0478386215596629, -429.8272453906067199, -306.7653713866226326 ) ) ;
#32742 = ORIENTED_EDGE ( 'NONE', *, *, #18974, .F. ) ;
#32743 = CARTESIAN_POINT ( 'NONE',  ( 755.8894580844503253, -303.8272453906071178, -332.3691319403863531 ) ) ;
#32744 = CIRCLE ( 'NONE', #15781, 6.119000000000013095 ) ;
#32746 = CARTESIAN_POINT ( 'NONE',  ( 793.0897708529556667, -366.5545181178795815, 361.3366627262616362 ) ) ;
#32745 = CARTESIAN_POINT ( 'NONE',  ( 800.2193346964447755, -66.99823902205672255, 355.1360043628815788 ) ) ;
#32748 = CARTESIAN_POINT ( 'NONE',  ( 748.3538107759620743, -304.7146871989594388, 355.8262568251490165 ) ) ;
#32747 = CARTESIAN_POINT ( 'NONE',  ( 777.5031285880264704, -406.8164208402375266, 374.9108240113588408 ) ) ;
#32749 = CARTESIAN_POINT ( 'NONE',  ( 814.8230680027162407, -101.8055962898691718, 333.7305795820267917 ) ) ;
#32750 = CARTESIAN_POINT ( 'NONE',  ( 775.8780910478218402, -273.2817908451526137, -364.9511171171680530 ) ) ;
#32751 = CARTESIAN_POINT ( 'NONE',  ( 797.8594530101008786, -277.5436935675105019, -322.1405469898980982 ) ) ;
#32752 = CARTESIAN_POINT ( 'NONE',  ( -338.8365100919713200, 230.0000000000001137, -202.7499999999916724 ) ) ;
#32753 = CARTESIAN_POINT ( 'NONE',  ( 765.0180583372156207, -168.9982390220563673, -360.0135310231089534 ) ) ;
#32754 = FACE_OUTER_BOUND ( 'NONE', #35190, .T. ) ;
#32755 = EDGE_LOOP ( 'NONE', ( #30345, #29976, #34129, #30116, #26087, #14273 ) ) ;
#32756 = CARTESIAN_POINT ( 'NONE',  ( 767.6429770376289525, -417.1800572038736163, 306.8695393053162093 ) ) ;
#32758 = CARTESIAN_POINT ( 'NONE',  ( -728.8365100919714905, 256.5000000000001705, -199.9999999999890861 ) ) ;
#32757 = CARTESIAN_POINT ( 'NONE',  ( 999.9999999999992042, -599.0000000000001137, 359.0000000000000000 ) ) ;
#32759 = CARTESIAN_POINT ( 'NONE',  ( 814.4686193811664907, -99.28179084515313946, -346.2056067578752732 ) ) ;
#32760 = DIRECTION ( 'NONE',  ( -1.000000000000000000, 0.000000000000000000, 0.000000000000000000 ) ) ;
#32761 = DIRECTION ( 'NONE',  ( -1.000000000000000000, 0.000000000000000000, 0.000000000000000000 ) ) ;
#32762 = CARTESIAN_POINT ( 'NONE',  ( 772.4468031744293057, -297.8272453906070041, 363.8651313633793620 ) ) ;
#32763 = CARTESIAN_POINT ( 'NONE',  ( 797.8594530101008786, -157.5436935675108998, 322.1405469898980982 ) ) ;
#32764 = ORIENTED_EDGE ( 'NONE', *, *, #37597, .T. ) ;
#32765 = VECTOR ( 'NONE', #38675, 1000.000000000000000 ) ;
#32766 = CIRCLE ( 'NONE', #28323, 10.00000000000000888 ) ;
#32767 = CARTESIAN_POINT ( 'NONE',  ( 748.9653473494365699, -122.6346026584201496, -356.9462024416520762 ) ) ;
#32768 = CARTESIAN_POINT ( 'NONE',  ( 775.9200461376533440, -335.8055962898683902, 315.3028492785443291 ) ) ;
#32769 = LINE ( 'NONE', #19747, #28578 ) ;
#32770 = CARTESIAN_POINT ( 'NONE',  ( 764.1737431748507561, -82.37269993606227558, 371.6461892240376415 ) ) ;
#32771 = CARTESIAN_POINT ( 'NONE',  ( 796.7737145352015204, -284.6346026584196807, -370.7187646348536987 ) ) ;
#32772 = CARTESIAN_POINT ( 'NONE',  ( 759.7806653035534055, -102.9982390220565520, 324.8639956371180801 ) ) ;
#32773 = DIRECTION ( 'NONE',  ( 0.000000000000000000, 0.000000000000000000, 1.000000000000000000 ) ) ;
#32774 = CARTESIAN_POINT ( 'NONE',  ( 754.0944755984390895, -303.6237781080503169, -364.1009440267246760 ) ) ;
#32775 = AXIS2_PLACEMENT_3D ( 'NONE', #20954, #27435, #40159 ) ;
#32776 = CARTESIAN_POINT ( 'NONE',  ( 804.6971507214547046, -3.281790845153435221, 344.0799538623459739 ) ) ;
#32777 = CARTESIAN_POINT ( 'NONE',  ( 808.3070685750230950, -354.9982390220557704, -361.1904061080339261 ) ) ;
#32778 = FACE_OUTER_BOUND ( 'NONE', #41213, .T. ) ;
#32779 = CARTESIAN_POINT ( 'NONE',  ( 779.4709603349208464, -384.3510508353227806, 314.7162404726379918 ) ) ;
#32780 = ORIENTED_EDGE ( 'NONE', *, *, #36838, .T. ) ;
#32781 = CARTESIAN_POINT ( 'NONE',  ( 754.8072714833581358, -412.8164208402372992, -338.1981804954720587 ) ) ;
#32783 = ADVANCED_FACE ( 'NONE', ( #41993 ), #41776, .F. ) ;
#32782 = CARTESIAN_POINT ( 'NONE',  ( 805.9055244015594326, -99.62377810805098477, -315.8990559732753240 ) ) ;
#32784 = CARTESIAN_POINT ( 'NONE',  ( -468.8365100919714337, 240.0000000000001705, -199.9999999999908766 ) ) ;
#32785 = CARTESIAN_POINT ( 'NONE',  ( 756.1443688327750579, -237.6237781080505442, 314.3581564841659315 ) ) ;
#32786 = CARTESIAN_POINT ( 'NONE',  ( 768.0187753319979720, -56.63460265842036279, 318.0580252608186242 ) ) ;
#32787 = ORIENTED_EDGE ( 'NONE', *, *, #41538, .F. ) ;
#32788 = CARTESIAN_POINT ( 'NONE',  ( 800.7704444035546203, -220.1692326535051052, -326.0291762391768771 ) ) ;
#32789 = CARTESIAN_POINT ( 'NONE',  ( 803.4237431249931660, -231.1800572038743553, 331.2633955100225194 ) ) ;
#32790 = CARTESIAN_POINT ( 'NONE',  ( 795.6651683502461765, -58.71468719896019905, -371.3240766477733814 ) ) ;
#32791 =( GEOMETRIC_REPRESENTATION_CONTEXT ( 3 ) GLOBAL_UNCERTAINTY_ASSIGNED_CONTEXT ( ( #40298 ) ) GLOBAL_UNIT_ASSIGNED_CONTEXT ( ( #17635, #3305, #35173 ) ) REPRESENTATION_CONTEXT ( 'NONE', 'WORKASPACE' ) );
#32792 = CARTESIAN_POINT ( 'NONE',  ( 807.6521310549275086, -452.9681489794448339, -339.7933401739554711 ) ) ;
#32793 = CIRCLE ( 'NONE', #19483, 24.99999999999991118 ) ;
#32794 = EDGE_LOOP ( 'NONE', ( #2444, #23117, #34595, #9829 ) ) ;
#32795 = CARTESIAN_POINT ( 'NONE',  ( 815.3608509340175488, -338.7363362996978822, -341.2497674668889545 ) ) ;
#32796 = CARTESIAN_POINT ( 'NONE',  ( 772.4837098697145166, -287.3618753856923718, 374.5518280994205611 ) ) ;
#32797 = CARTESIAN_POINT ( 'NONE',  ( 749.8865473780648472, -20.53286901714212931, 322.1177392798429082 ) ) ;
#32798 = CARTESIAN_POINT ( 'NONE',  ( 755.8894580844503253, -183.8272453906074020, -332.3691319403863531 ) ) ;
#32799 = CARTESIAN_POINT ( 'NONE',  ( 801.9419747391806368, -186.4527844766017779, -351.9812246680014027 ) ) ;
#32800 = CARTESIAN_POINT ( 'NONE',  ( 762.1405469898973024, -385.5436935675102745, -357.8594530101016176 ) ) ;
#32801 = ORIENTED_EDGE ( 'NONE', *, *, #7988, .T. ) ;
#32802 = ORIENTED_EDGE ( 'NONE', *, *, #28955, .T. ) ;
#32803 = CARTESIAN_POINT ( 'NONE',  ( 796.7737145352015204, -308.6346026584195670, 370.7187646348536987 ) ) ;
#32804 = AXIS2_PLACEMENT_3D ( 'NONE', #35270, #16822, #24188 ) ;
#32805 = LINE ( 'NONE', #11104, #29966 ) ;
#32806 = CARTESIAN_POINT ( 'NONE',  ( 800.9840315886518738, -220.9181544815164102, 354.1144889064786412 ) ) ;
#32807 = LINE ( 'NONE', #25864, #33437 ) ;
#32808 = AXIS2_PLACEMENT_3D ( 'NONE', #8852, #30092, #8401 ) ;
#32809 = CARTESIAN_POINT ( 'NONE',  ( 804.1105419155481968, -195.8272453906074304, 347.6308680596136469 ) ) ;
#32810 = CARTESIAN_POINT ( 'NONE',  ( 797.8594530101008786, -61.54369356751124087, 322.1405469898980982 ) ) ;
#32811 = EDGE_CURVE ( 'NONE', #23400, #29488, #17740, .T. ) ;
#32812 = VERTEX_POINT ( 'NONE', #42209 ) ;
#32813 = CARTESIAN_POINT ( 'NONE',  ( 752.7379699480933368, -420.0090635724249069, -361.9858362298580232 ) ) ;
#32814 = CARTESIAN_POINT ( 'NONE',  ( 796.9462024416508257, -12.45278447660232324, -308.9653473494370246 ) ) ;
#32815 = CARTESIAN_POINT ( 'NONE',  ( 781.2370466360911223, -260.7363362996981095, 304.9990715423533629 ) ) ;
#32816 = CARTESIAN_POINT ( 'NONE',  ( 786.6156483768007774, -217.4419599262324141, 315.5913626894246136 ) ) ;
#32817 = CARTESIAN_POINT ( 'NONE',  ( 774.6312213355099630, -407.3618753856920307, -364.6798772138717482 ) ) ;
#32818 = CARTESIAN_POINT ( 'NONE',  ( 791.9812246680005501, 3.365397341579444479, -361.9419747391813189 ) ) ;
#32819 = CARTESIAN_POINT ( 'NONE',  ( 784.1219089521767955, -453.2817908451519315, 315.0488828828318333 ) ) ;
#32820 =( LENGTH_UNIT ( ) NAMED_UNIT ( * ) SI_UNIT ( .MILLI., .METRE. ) );
#32821 = CARTESIAN_POINT ( 'NONE',  ( 766.0291762391763086, -250.9181544815163534, -360.7704444035551319 ) ) ;
#32822 = CLOSED_SHELL ( 'NONE', ( #39335, #38204, #21922, #33943 ) ) ;
#32823 = CARTESIAN_POINT ( 'NONE',  ( 758.8095938919642549, -32.08914811296588709, 311.6929314249763365 ) ) ;
#32824 = CARTESIAN_POINT ( 'NONE',  ( 745.7998596910086917, -101.3618753856929544, 332.5602148656461168 ) ) ;
#32825 = CARTESIAN_POINT ( 'NONE',  ( -775.4999999999993179, -563.3203001761230553, -342.3463313526983143 ) ) ;
#32826 = AXIS2_PLACEMENT_3D ( 'NONE', #8578, #37179, #5099 ) ;
#32827 =( NAMED_UNIT ( * ) SI_UNIT ( $, .STERADIAN. ) SOLID_ANGLE_UNIT ( ) );
#32828 = AXIS2_PLACEMENT_3D ( 'NONE', #7907, #3961, #11589 ) ;
#32829 = CARTESIAN_POINT ( 'NONE',  ( 748.6759233522253680, -376.3726999360614514, 324.3348316497537098 ) ) ;
#32830 = DIRECTION ( 'NONE',  ( 1.000000000000000000, -0.000000000000000000, -0.000000000000000000 ) ) ;
#32831 = CARTESIAN_POINT ( 'NONE',  ( 808.3070685750230950, -378.9982390220555999, 361.1904061080339261 ) ) ;
#32832 = CARTESIAN_POINT ( 'NONE',  ( 802.1676090361156639, -326.6346026584193396, -327.8955696845344505 ) ) ;
#32833 = EDGE_CURVE ( 'NONE', #8307, #33095, #10559, .T. ) ;
#32834 = CARTESIAN_POINT ( 'NONE',  ( 775.9200461376533440, 0.1944037101305369775, 315.3028492785443291 ) ) ;
#32835 = CARTESIAN_POINT ( 'NONE',  ( 757.0176451133909268, -181.0999726633347109, 349.9200121543848354 ) ) ;
#32836 = CARTESIAN_POINT ( 'NONE',  ( 773.7305795820266212, -81.28179084515319630, -374.8230680027170365 ) ) ;
#32837 = CARTESIAN_POINT ( 'NONE',  ( 756.1348686366196716, -137.2601417444144829, -347.5531968255698416 ) ) ;
#32838 = CARTESIAN_POINT ( 'NONE',  ( 788.7631598425961101, -121.4419599262327267, 305.7194118038759143 ) ) ;
#32839 = CARTESIAN_POINT ( 'NONE',  ( 762.3223304703356007, -439.5436935675101040, 322.3223304703362828 ) ) ;
#32840 = VECTOR ( 'NONE', #17448, 1000.000000000000000 ) ;
#32841 = CARTESIAN_POINT ( 'NONE',  ( 800.0135310231082713, -14.08914811296595460, -325.0180583372163028 ) ) ;
#32842 = CARTESIAN_POINT ( 'NONE',  ( 769.1273215169530886, -118.7146871989600072, -317.4527132478988847 ) ) ;
#32843 = CARTESIAN_POINT ( 'NONE',  ( 762.3223304703356007, -127.5436935675110561, -322.3223304703362828 ) ) ;
#32844 = EDGE_CURVE ( 'NONE', #20464, #34629, #18184, .T. ) ;
#32845 = VECTOR ( 'NONE', #38934, 1000.000000000000000 ) ;
#32846 = AXIS2_PLACEMENT_3D ( 'NONE', #33828, #3037, #30352 ) ;
#32847 = CARTESIAN_POINT ( 'NONE',  ( 789.9200121543843807, -433.9874144716862361, -317.0176451133914384 ) ) ;
#32849 = CARTESIAN_POINT ( 'NONE',  ( 803.4237431249931660, -255.1800572038742700, 331.2633955100225194 ) ) ;
#32848 = CARTESIAN_POINT ( 'NONE',  ( 797.6776695296629214, -259.5436935675106156, 357.6776695296636603 ) ) ;
#32850 = DIRECTION ( 'NONE',  ( -1.000000000000000000, -0.000000000000000000, 0.000000000000000000 ) ) ;
#32851 = VERTEX_POINT ( 'NONE', #38299 ) ;
#32852 = CARTESIAN_POINT ( 'NONE',  ( 761.2382568024794409, 8.376221891948691933, 356.9571628226838129 ) ) ;
#32853 = ORIENTED_EDGE ( 'NONE', *, *, #23281, .T. ) ;
#32854 = CARTESIAN_POINT ( 'NONE',  ( 804.7487373415286811, -187.5436935675108430, 364.7487373415288516 ) ) ;
#32855 = CARTESIAN_POINT ( 'NONE',  ( 798.5707757039680246, -269.4636090269708006, 356.7845633553585003 ) ) ;
#32856 = ORIENTED_EDGE ( 'NONE', *, *, #16211, .F. ) ;
#32857 = CARTESIAN_POINT ( 'NONE',  ( 763.0428371773158460, -83.46360902697136908, -358.7617431975195359 ) ) ;
#32858 = CARTESIAN_POINT ( 'NONE',  ( 783.7566961878529810, -216.8965053807778816, 305.1792804349288417 ) ) ;
#32859 = CARTESIAN_POINT ( 'NONE',  ( 767.8955696845334842, -264.4527844766016074, -362.1676090361161755 ) ) ;
#32860 = VECTOR ( 'NONE', #38129, 1000.000000000000000 ) ;
#32861 = ORIENTED_EDGE ( 'NONE', *, *, #665, .F. ) ;
#32862 = EDGE_CURVE ( 'NONE', #29646, #40310, #30476, .T. ) ;
#32863 = CARTESIAN_POINT ( 'NONE',  ( 804.6798772138708955, -399.7255117493283478, -334.6312213355107019 ) ) ;
#32864 = CARTESIAN_POINT ( 'NONE',  ( 805.1927285166397041, -64.81642084023852135, -341.8018195045277707 ) ) ;
#32865 = AXIS2_PLACEMENT_3D ( 'NONE', #23990, #30721, #45502 ) ;
#32866 = EDGE_CURVE ( 'NONE', #4510, #27542, #2458, .T. ) ;
#32867 = CARTESIAN_POINT ( 'NONE',  ( 783.0433043558608688, -264.8965053807776826, 315.1538015810313027 ) ) ;
#32868 = DIRECTION ( 'NONE',  ( 0.000000000000000000, -1.000000000000000000, 0.000000000000000000 ) ) ;
#32869 = CARTESIAN_POINT ( 'NONE',  ( -28.63011601220122415, -365.3551492539851893, -8.132432514707076621 ) ) ;
#32870 = CARTESIAN_POINT ( 'NONE',  ( 814.8207195650702488, -26.19088175424427334, -336.2433038121456548 ) ) ;
#32871 = FACE_OUTER_BOUND ( 'NONE', #31420, .T. ) ;
#32872 = EDGE_CURVE ( 'NONE', #18154, #32812, #36393, .T. ) ;
#32873 = ORIENTED_EDGE ( 'NONE', *, *, #20771, .F. ) ;
#32874 = CARTESIAN_POINT ( 'NONE',  ( 793.5525998758768083, -319.0999726633342561, -372.6845335610516941 ) ) ;
#32875 = CARTESIAN_POINT ( 'NONE',  ( 811.3240766477731540, -172.3726999360619914, 355.6651683502462902 ) ) ;
#32876 = AXIS2_PLACEMENT_3D ( 'NONE', #8089, #36467, #29334 ) ;
#32878 = CARTESIAN_POINT ( 'NONE',  ( 791.9812246680005501, -260.6346026584197375, -361.9419747391813189 ) ) ;
#32877 = CARTESIAN_POINT ( 'NONE',  ( 759.9999999999992042, 205.0000000000000568, -339.9999999999999432 ) ) ;
#32879 = DIRECTION ( 'NONE',  ( -1.000000000000000000, -0.000000000000000000, -0.000000000000000000 ) ) ;
#32880 = CARTESIAN_POINT ( 'NONE',  ( 755.5913626894240451, -157.6454272087893287, -346.6156483768012890 ) ) ;
#32881 = AXIS2_PLACEMENT_3D ( 'NONE', #31963, #14895, #39618 ) ;
#32882 = CARTESIAN_POINT ( 'NONE',  ( 796.9462024416508257, -12.45278447660232146, 308.9653473494370246 ) ) ;
#32883 = AXIS2_PLACEMENT_3D ( 'NONE', #16811, #44517, #41513 ) ;
#32884 = CARTESIAN_POINT ( 'NONE',  ( 799.9999999999993179, -365.3551492539851893, -18.13243251470705886 ) ) ;
#32885 = CARTESIAN_POINT ( 'NONE',  ( 748.9653473494365699, -362.6346026584193964, -356.9462024416520762 ) ) ;
#32886 = FACE_OUTER_BOUND ( 'NONE', #19840, .T. ) ;
#32887 = CARTESIAN_POINT ( 'NONE',  ( 755.5713283507202505, -53.36187538569310362, 334.6858677611754729 ) ) ;
#32888 = ADVANCED_FACE ( 'NONE', ( #17511 ), #41765, .F. ) ;
#32889 = CARTESIAN_POINT ( 'NONE',  ( 793.5525998758768083, -295.0999726633343698, 372.6845335610516941 ) ) ;
#32890 = CARTESIAN_POINT ( 'NONE',  ( 749.8865473780648472, -236.5328690171414792, -322.1177392798429082 ) ) ;
#32891 = CARTESIAN_POINT ( 'NONE',  ( 746.8695393053150156, -245.9073299311469896, 327.6429770376306010 ) ) ;
#32892 = CARTESIAN_POINT ( 'NONE',  ( 793.9861285913068514, -442.9180389616178672, -372.1637643035757606 ) ) ;
#32893 = DIRECTION ( 'NONE',  ( 0.000000000000000000, 0.000000000000000000, -1.000000000000000000 ) ) ;
#32894 = ADVANCED_FACE ( 'NONE', ( #34813 ), #3870, .F. ) ;
#32895 = ORIENTED_EDGE ( 'NONE', *, *, #4622, .F. ) ;
#32896 = CARTESIAN_POINT ( 'NONE',  ( 767.8955696845333705, -336.4527844766012095, 362.1676090361162323 ) ) ;
#32897 = VECTOR ( 'NONE', #35407, 999.9999999999998863 ) ;
#32898 = CARTESIAN_POINT ( 'NONE',  ( 804.6971507214547046, -99.28179084515313946, 344.0799538623459739 ) ) ;
#32899 = CARTESIAN_POINT ( 'NONE',  ( 800.7704444035546203, -4.169232653505813069, -326.0291762391768771 ) ) ;
#32900 = CIRCLE ( 'NONE', #43952, 10.00000000000000888 ) ;
#32901 = PLANE ( 'NONE',  #37276 ) ;
#32902 = LINE ( 'NONE', #1248, #7097 ) ;
#32903 = CARTESIAN_POINT ( 'NONE',  ( 803.8556311672234642, -129.6237781080508853, 365.6418435158340117 ) ) ;
#32905 = CARTESIAN_POINT ( 'NONE',  ( 762.1405469898971887, -385.5436935675102745, 357.8594530101015607 ) ) ;
#32904 = CARTESIAN_POINT ( 'NONE',  ( 759.2295555964440155, -160.1692326535053326, 353.9708237608231229 ) ) ;
#32906 = EDGE_LOOP ( 'NONE', ( #18376, #16490 ) ) ;
#32907 = EDGE_CURVE ( 'NONE', #10930, #25389, #37770, .T. ) ;
#32908 = ADVANCED_FACE ( 'NONE', ( #17264, #38513, #20945 ), #35042, .T. ) ;
#32909 = CARTESIAN_POINT ( 'NONE',  ( 770.0799878456142551, -325.9874144716865771, -362.9823548866085616 ) ) ;
#32910 = CARTESIAN_POINT ( 'NONE',  ( 755.0636971347428243, -148.2709662947837330, 341.7834795799807353 ) ) ;
#32911 = UNCERTAINTY_MEASURE_WITH_UNIT (LENGTH_MEASURE( 1.000000000000000082E-05 ), #37939, 'distance_accuracy_value', 'NONE');
#32912 = CARTESIAN_POINT ( 'NONE',  ( 788.7631598425961101, -313.4419599262320730, -305.7194118038759143 ) ) ;
#32913 = CARTESIAN_POINT ( 'NONE',  ( 799.9999999999993179, 166.4563064324884465, -319.9999999999999432 ) ) ;
#32914 = CARTESIAN_POINT ( 'NONE',  ( 793.4146539503750546, -433.9874144716862361, 307.6481478633938877 ) ) ;
#32915 = ORIENTED_EDGE ( 'NONE', *, *, #1846, .T. ) ;
#32916 = CARTESIAN_POINT ( 'NONE',  ( 803.4237431249931660, -375.1800572038739574, 331.2633955100225194 ) ) ;
#32917 = CARTESIAN_POINT ( 'NONE',  ( 755.8398074228967971, -67.44195992623289726, -333.4516893846970333 ) ) ;
#32918 = EDGE_LOOP ( 'NONE', ( #24818, #2376 ) ) ;
#32919 = DIRECTION ( 'NONE',  ( -1.000000000000000000, -0.000000000000000000, -0.000000000000000000 ) ) ;
#32920 = VECTOR ( 'NONE', #20404, 1000.000000000000000 ) ;
#32921 = CARTESIAN_POINT ( 'NONE',  ( 796.9462024416508257, -180.4527844766017211, -308.9653473494370246 ) ) ;
#32922 = ORIENTED_EDGE ( 'NONE', *, *, #36821, .T. ) ;
#32923 = CARTESIAN_POINT ( 'NONE',  ( 762.1405469898973024, -169.5436935675108998, -357.8594530101016176 ) ) ;
#32924 = EDGE_LOOP ( 'NONE', ( #14956, #35277 ) ) ;
#32925 = CARTESIAN_POINT ( 'NONE',  ( 804.4086373105744769, -433.6454272087884760, -333.3843516231986541 ) ) ;
#32926 = EDGE_CURVE ( 'NONE', #44486, #42944, #39825, .T. ) ;
#32927 = CARTESIAN_POINT ( 'NONE',  ( 754.8072714833581358, -4.816420840238714085, 338.1981804954720587 ) ) ;
#32928 = CARTESIAN_POINT ( 'NONE',  ( 763.0537975583475827, -216.4527844766016926, 371.0346526505627480 ) ) ;
#32929 = CARTESIAN_POINT ( 'NONE',  ( 783.0433043558608688, -144.8965053807781089, 315.1538015810313027 ) ) ;
#32931 = DIRECTION ( 'NONE',  ( 4.625929269271485914E-16, -1.000000000000000000, -0.000000000000000000 ) ) ;
#32930 = CARTESIAN_POINT ( 'NONE',  ( -78.83651009197140525, 260.0000000000000568, -199.9999999999936051 ) ) ;
#32932 = ORIENTED_EDGE ( 'NONE', *, *, #44199, .F. ) ;
#32933 = CARTESIAN_POINT ( 'NONE',  ( 757.0176451133909268, -445.0999726633338582, -349.9200121543848354 ) ) ;
#32934 = LINE ( 'NONE', #15379, #38811 ) ;
#32935 = CARTESIAN_POINT ( 'NONE',  ( 812.3518521366052028, -217.0999726633345972, -326.5853460496235243 ) ) ;
#32936 = CARTESIAN_POINT ( 'NONE',  ( 783.7953271457878373, -56.19088175424417386, 375.1787889125761239 ) ) ;
#32938 = FACE_OUTER_BOUND ( 'NONE', #32755, .T. ) ;
#32937 = DIRECTION ( 'NONE',  ( 0.000000000000000000, 0.000000000000000000, -1.000000000000000000 ) ) ;
#32939 = CARTESIAN_POINT ( 'NONE',  ( 776.9566956441375396, -324.8965053807775121, -364.8461984189686405 ) ) ;
#32940 = CARTESIAN_POINT ( 'NONE',  ( 180.7583438952258916, 294.6698570112193920, -244.9999999999999716 ) ) ;
#32941 = CARTESIAN_POINT ( 'NONE',  ( 747.6481478633932056, -181.0999726633347109, -353.4146539503763620 ) ) ;
#32942 = CARTESIAN_POINT ( 'NONE',  ( 927.9999999999992042, 154.9999999999998863, -350.0000000000000000 ) ) ;
#32943 = DIRECTION ( 'NONE',  ( 0.000000000000000000, 0.000000000000000000, 1.000000000000000000 ) ) ;
#32944 = CIRCLE ( 'NONE', #30718, 10.00000000000006395 ) ;
#32945 = CARTESIAN_POINT ( 'NONE',  ( 790.9844846989617508, -406.3726999360612808, 317.2208543904092721 ) ) ;
#32946 = CARTESIAN_POINT ( 'NONE',  ( 814.2001403089898304, -257.3618753856924286, -347.4397851343538264 ) ) ;
#32947 = CYLINDRICAL_SURFACE ( 'NONE', #5433, 2.749999999999863665 ) ;
#32948 = CARTESIAN_POINT ( 'NONE',  ( 795.1360043628807261, -20.08914811296592973, -360.2193346964456282 ) ) ;
#32949 = ADVANCED_FACE ( 'NONE', ( #29492 ), #32969, .F. ) ;
#32950 = CARTESIAN_POINT ( 'NONE',  ( 811.3240766477731540, -172.3726999360619914, 355.6651683502462902 ) ) ;
#32951 = CARTESIAN_POINT ( 'NONE',  ( 766.5853460496234675, -133.9874144716872024, -372.3518521366060554 ) ) ;
#32952 = CARTESIAN_POINT ( 'NONE',  ( 810.7187646348534145, -138.4527844766019200, 356.7737145352016341 ) ) ;
#32953 = CARTESIAN_POINT ( 'NONE',  ( 787.4397851343537695, -381.7255117493284615, -374.2001403089903988 ) ) ;
#32954 = CIRCLE ( 'NONE', #21136, 2.749999999999919176 ) ;
#32955 = DIRECTION ( 'NONE',  ( -0.000000000000000000, 1.000000000000000000, -0.000000000000000000 ) ) ;
#32957 = EDGE_CURVE ( 'NONE', #45720, #4703, #15752, .T. ) ;
#32956 = DIRECTION ( 'NONE',  ( 1.000000000000000000, 0.000000000000000000, 0.000000000000000000 ) ) ;
#32958 = CARTESIAN_POINT ( 'NONE',  ( 791.9812246680005501, -236.6346026584198228, 361.9419747391813189 ) ) ;
#32959 = CARTESIAN_POINT ( 'NONE',  ( 755.5913626894240451, -37.64542720878968396, 346.6156483768012890 ) ) ;
#32960 = CARTESIAN_POINT ( 'NONE',  ( 797.8594530101008786, -397.5436935675100472, -322.1405469898980982 ) ) ;
#32961 = CARTESIAN_POINT ( 'NONE',  ( 813.1304606946830518, -449.9073299311463643, -352.3570229623690580 ) ) ;
#32962 = CARTESIAN_POINT ( 'NONE',  ( 799.9999999999993179, -512.9681489794448908, -370.0000000000000000 ) ) ;
#32963 = CARTESIAN_POINT ( 'NONE',  ( 773.7943932421234194, -23.80559628986938847, 305.5313806188329409 ) ) ;
#32964 = ORIENTED_EDGE ( 'NONE', *, *, #29445, .T. ) ;
#32965 = MANIFOLD_SOLID_BREP ( 'Cut-Extrude9', #10692 ) ;
#32966 = CARTESIAN_POINT ( 'NONE',  ( 804.9511171171677688, -173.8055962898689302, -335.8780910478229202 ) ) ;
#32967 = CARTESIAN_POINT ( 'NONE',  ( 756.5762568750052424, -27.18005720387500901, 348.7366044899774238 ) ) ;
#32968 = CARTESIAN_POINT ( 'NONE',  ( 766.5853460496234675, -229.9874144716869466, -372.3518521366060554 ) ) ;
#32969 = CYLINDRICAL_SURFACE ( 'NONE', #26780, 2.749999999999863665 ) ;
#32970 = CARTESIAN_POINT ( 'NONE',  ( 778.7502325331095108, -360.3510508353228374, 304.6391490659818828 ) ) ;
#32971 = CARTESIAN_POINT ( 'NONE',  ( 803.4237431249931660, -87.18005720387481006, -331.2633955100225194 ) ) ;
#32972 = ORIENTED_EDGE ( 'NONE', *, *, #32364, .T. ) ;
#32973 = CARTESIAN_POINT ( 'NONE',  ( 758.0141637701419768, -423.0783235625953580, 367.2620300519063790 ) ) ;
#32974 = CARTESIAN_POINT ( 'NONE',  ( 797.6776695296629214, -139.5436935675110135, -357.6776695296636603 ) ) ;
#32975 = CARTESIAN_POINT ( 'NONE',  ( 797.6776695296629214, -355.5436935675103882, 357.6776695296636603 ) ) ;
#32976 = AXIS2_PLACEMENT_3D ( 'NONE', #42466, #35301, #6894 ) ;
#32977 = CARTESIAN_POINT ( 'NONE',  ( 745.7998596910086917, -77.36187538569302546, -332.5602148656461168 ) ) ;
#32978 = AXIS2_PLACEMENT_3D ( 'NONE', #5819, #14067, #10589 ) ;
#32979 = VECTOR ( 'NONE', #40083, 1000.000000000000000 ) ;
#32980 = EDGE_LOOP ( 'NONE', ( #31412, #38361, #39898, #44030, #1645, #34421 ) ) ;
#32981 = CARTESIAN_POINT ( 'NONE',  ( 796.9571628226829034, -23.46360902697155026, -321.2382568024804641 ) ) ;
#32982 = AXIS2_PLACEMENT_3D ( 'NONE', #42282, #14592, #39286 ) ;
#32983 = VERTEX_POINT ( 'NONE', #11933 ) ;
#32984 = CARTESIAN_POINT ( 'NONE',  ( 755.5913626894240451, -325.6454272087888739, -346.6156483768012890 ) ) ;
#32986 = CARTESIAN_POINT ( 'NONE',  ( 763.0428371773158460, -371.4636090269705164, 358.7617431975195359 ) ) ;
#32985 = CARTESIAN_POINT ( 'NONE',  ( 756.5762568750052424, -75.18005720387485269, 348.7366044899774238 ) ) ;
#32987 = CARTESIAN_POINT ( 'NONE',  ( 759.7806653035534055, -318.9982390220557704, -324.8639956371180801 ) ) ;
#32988 = VECTOR ( 'NONE', #6668, 1000.000000000000000 ) ;
#32990 = CARTESIAN_POINT ( 'NONE',  ( 783.7566961878529810, -336.8965053807774552, 305.1792804349288417 ) ) ;
#32989 = CARTESIAN_POINT ( 'NONE',  ( 747.2067596250078623, -411.1800572038738437, 352.2312462859687230 ) ) ;
#32991 = CARTESIAN_POINT ( 'NONE',  ( 744.8212110874229666, -90.89650538077827946, 336.2046728542121627 ) ) ;
#32992 = CARTESIAN_POINT ( 'NONE',  ( 759.0159684113467620, -304.9181544815161828, -325.8855110935213020 ) ) ;
#32993 = CARTESIAN_POINT ( 'NONE',  ( 785.3687786644884454, -299.3618753856922581, -315.3201227861279676 ) ) ;
#32994 = LINE ( 'NONE', #16489, #24307 ) ;
#32995 = CARTESIAN_POINT ( 'NONE',  ( 757.8323909638827445, -146.6346026584200217, -352.1044303154654358 ) ) ;
#32996 = DIRECTION ( 'NONE',  ( 1.000000000000000000, -0.000000000000000000, -0.000000000000000000 ) ) ;
#32997 = CARTESIAN_POINT ( 'NONE',  ( 758.8095938919642549, -416.0891481129645513, 311.6929314249763365 ) ) ;
#32999 = FACE_OUTER_BOUND ( 'NONE', #7173, .T. ) ;
#32998 = DIRECTION ( 'NONE',  ( -4.440892098500622217E-15, 1.000000000000000000, 0.000000000000000000 ) ) ;
#33000 = CARTESIAN_POINT ( 'NONE',  ( 802.2119215644370342, -78.00906357242591582, -367.5423716828165084 ) ) ;
#33001 = CARTESIAN_POINT ( 'NONE',  ( 767.9999999999992042, 178.9475563372491251, -320.0000000000000000 ) ) ;
#33002 = DIRECTION ( 'NONE',  ( 0.000000000000000000, 0.3826834323650836756, 0.9238795325112892920 ) ) ;
#33003 = CARTESIAN_POINT ( 'NONE',  ( 793.0897708529556667, -294.5545181178797520, 361.3366627262616362 ) ) ;
#33004 = CARTESIAN_POINT ( 'NONE',  ( 771.1735550268778070, -153.1800572038746395, 316.3353852180827630 ) ) ;
#33005 = ORIENTED_EDGE ( 'NONE', *, *, #7197, .T. ) ;
#33006 = CARTESIAN_POINT ( 'NONE',  ( 800.9747183278959710, -132.9982390220564810, -311.9810565676471583 ) ) ;
#33007 = CARTESIAN_POINT ( 'NONE',  ( 802.7791456095903868, -340.7146871989592114, 329.0155153010375102 ) ) ;
#33008 = AXIS2_PLACEMENT_3D ( 'NONE', #2648, #29076, #39723 ) ;
#33009 = DIRECTION ( 'NONE',  ( 0.000000000000000000, 0.000000000000000000, -1.000000000000000000 ) ) ;
#33010 = CARTESIAN_POINT ( 'NONE',  ( 801.3366627262608972, -416.5328690171409107, -353.0897708529566899 ) ) ;
#33011 = CARTESIAN_POINT ( 'NONE',  ( 745.5313806188320314, -63.28179084515324604, 333.7943932421247268 ) ) ;
#33012 = CARTESIAN_POINT ( 'NONE',  ( 814.9108240113580450, -280.2709662947833067, -337.5031285880265273 ) ) ;
#33013 = CARTESIAN_POINT ( 'NONE',  ( 801.1904061080336987, -212.0891481129652902, 368.3070685750235498 ) ) ;
#33014 = CARTESIAN_POINT ( 'NONE',  ( 756.3353852180819104, -125.9073299311474159, 331.1735550268788302 ) ) ;
#33015 = EDGE_LOOP ( 'NONE', ( #22107, #6481, #10563, #25830 ) ) ;
#33016 = CARTESIAN_POINT ( 'NONE',  ( 805.9055244015594326, -315.6237781080503169, -315.8990559732753240 ) ) ;
#33017 = AXIS2_PLACEMENT_3D ( 'NONE', #37951, #17395, #21083 ) ;
#33018 = CARTESIAN_POINT ( 'NONE',  ( 757.4527132478984868, -16.37269993606248519, 329.1273215169538844 ) ) ;
#33019 = CARTESIAN_POINT ( 'NONE',  ( 744.7301800767019131, -364.8164208402374697, -337.4774526936615757 ) ) ;
#33020 = DIRECTION ( 'NONE',  ( 0.000000000000000000, -1.000000000000000000, 0.000000000000000000 ) ) ;
#33021 = CARTESIAN_POINT ( 'NONE',  ( 756.7813123517142913, -403.9874144716863498, 329.9779781133712504 ) ) ;
#33022 = VERTEX_POINT ( 'NONE', #11492 ) ;
#33023 = CARTESIAN_POINT ( 'NONE',  ( 787.6308680596127942, -83.26014174441466764, 364.1105419155492768 ) ) ;
#33024 = CARTESIAN_POINT ( 'NONE',  ( 795.1360043628807261, -428.0891481129644944, -360.2193346964456282 ) ) ;
#33025 = CARTESIAN_POINT ( 'NONE',  ( 759.7806653035534055, -222.9982390220561399, -324.8639956371180801 ) ) ;
#33026 = CARTESIAN_POINT ( 'NONE',  ( 746.7653713866222915, -137.2601417444144829, -351.0478386215610271 ) ) ;
#33027 = CARTESIAN_POINT ( 'NONE',  ( 989.9999999999992042, 62.85347435602256638, -357.4246812887967053 ) ) ;
#33028 = CARTESIAN_POINT ( 'NONE',  ( 768.8385539511368734, -239.2601417444141987, 306.4236121716840557 ) ) ;
#33029 = CARTESIAN_POINT ( 'NONE',  ( 755.0636971347428243, -52.27096629478401724, 341.7834795799807353 ) ) ;
#33030 = CARTESIAN_POINT ( 'NONE',  ( 760.5453621957607311, -237.0783235625960117, -323.8424801807151425 ) ) ;
#33031 = CARTESIAN_POINT ( 'NONE',  ( 778.1981804954714335, -250.2709662947832783, 314.8072714833589885 ) ) ;
#33032 = CARTESIAN_POINT ( 'NONE',  ( 815.0009284576459549, -54.35105083532383219, -338.7629533639073429 ) ) ;
#33033 = CARTESIAN_POINT ( 'NONE',  ( 989.9999999999992042, 56.73212367640085318, -362.5753187112032379 ) ) ;
#33034 = ORIENTED_EDGE ( 'NONE', *, *, #17079, .F. ) ;
#33035 = ORIENTED_EDGE ( 'NONE', *, *, #18199, .F. ) ;
#33036 = CARTESIAN_POINT ( 'NONE',  ( 815.3608509340175488, -362.7363362996977116, -341.2497674668889545 ) ) ;
#33037 = AXIS2_PLACEMENT_3D ( 'NONE', #22802, #41503, #33881 ) ;
#33038 = CARTESIAN_POINT ( 'NONE',  ( 777.4774526936600978, -274.2709662947832499, 304.7301800767028226 ) ) ;
#33039 = MANIFOLD_SOLID_BREP ( 'Move Face1', #36504 ) ;
#33040 = CARTESIAN_POINT ( 'NONE',  ( 766.5853460496234675, -37.98741447168752927, 372.3518521366060554 ) ) ;
#33041 = CARTESIAN_POINT ( 'NONE',  ( 783.0745993439762742, -200.1908817542436907, -365.1016975059196739 ) ) ;
#33042 = CARTESIAN_POINT ( 'NONE',  ( 757.8323909638827445, -194.6346026584198796, -352.1044303154654358 ) ) ;
#33043 = CARTESIAN_POINT ( 'NONE',  ( 768.0187753319979720, -368.6346026584193964, -318.0580252608186242 ) ) ;
#33044 = ORIENTED_EDGE ( 'NONE', *, *, #771, .T. ) ;
#33045 = CARTESIAN_POINT ( 'NONE',  ( 805.1016975059191054, 17.10349461922139369, -343.0745993439771837 ) ) ;
#33046 = EDGE_LOOP ( 'NONE', ( #37130, #43304, #24433, #9144 ) ) ;
#33047 = VECTOR ( 'NONE', #25899, 1000.000000000000000 ) ;
#33048 = CARTESIAN_POINT ( 'NONE',  ( 748.9653473494363425, -314.6346026584194533, 356.9462024416521331 ) ) ;
#33049 = DIRECTION ( 'NONE',  ( -0.000000000000000000, 1.000000000000000000, -0.000000000000000000 ) ) ;
#33050 = DIRECTION ( 'NONE',  ( 1.000000000000000000, -0.000000000000000000, -0.000000000000000000 ) ) ;
#33051 = CARTESIAN_POINT ( 'NONE',  ( 763.0428371773158460, -203.4636090269709996, 358.7617431975195359 ) ) ;
#33052 = CARTESIAN_POINT ( 'NONE',  ( 794.9819416627830151, -60.99823902205671544, 319.9864689768909898 ) ) ;
#33053 = ORIENTED_EDGE ( 'NONE', *, *, #17095, .F. ) ;
#33054 = CARTESIAN_POINT ( 'NONE',  ( 793.5525998758768083, -415.0999726633340288, -372.6845335610516941 ) ) ;
#33055 = CARTESIAN_POINT ( 'NONE',  ( 759.0252816721024374, -24.99823902205683268, -368.0189434323527280 ) ) ;
#33056 = CARTESIAN_POINT ( 'NONE',  ( 765.8855110935204493, -238.1692326535050768, 319.0159684113471599 ) ) ;
#33057 = CARTESIAN_POINT ( 'NONE',  ( 788.7366044899766848, -395.9073299311465348, -316.5762568750059813 ) ) ;
#33058 = CARTESIAN_POINT ( 'NONE',  ( 759.9864689768902508, -2.089148112965993231, -354.9819416627836404 ) ) ;
#33059 = CARTESIAN_POINT ( 'NONE',  ( 814.5518280994195948, -447.7255117493280636, 332.4837098697145734 ) ) ;
#33060 = CARTESIAN_POINT ( 'NONE',  ( -598.8365100919716042, 260.0000000000001705, -199.9999999999899671 ) ) ;
#33061 = CARTESIAN_POINT ( 'NONE',  ( 802.9823548866075953, -241.0999726633345119, -330.0799878456151077 ) ) ;
#33062 = CARTESIAN_POINT ( 'NONE',  ( 782.4968714119720516, -154.8164208402382371, -305.0891759886411023 ) ) ;
#33063 = CARTESIAN_POINT ( 'NONE',  ( 787.5162901302840055, -35.36187538569316047, 305.4481719005792684 ) ) ;
#33064 = CARTESIAN_POINT ( 'NONE',  ( 759.0252816721024374, -120.9982390220565378, 368.0189434323527280 ) ) ;
#33065 = DIRECTION ( 'NONE',  ( 1.000000000000000000, 0.000000000000000000, -0.000000000000000000 ) ) ;
#33066 = CARTESIAN_POINT ( 'NONE',  ( 760.0363995740630116, -394.9181544815158418, 368.7758568127991907 ) ) ;
#33067 = DIRECTION ( 'NONE',  ( 0.000000000000000000, 0.000000000000000000, -1.000000000000000000 ) ) ;
#33068 = CARTESIAN_POINT ( 'NONE',  ( 808.0189434323515343, -350.0891481129648923, 319.0252816721025511 ) ) ;
#33069 = CARTESIAN_POINT ( 'NONE',  ( 804.9363028652555840, -304.2709662947832499, -338.2165204200192079 ) ) ;
#33070 = CARTESIAN_POINT ( 'NONE',  ( 803.6646147819161570, -449.9073299311463643, 348.8264449731210561 ) ) ;
#33071 = CARTESIAN_POINT ( 'NONE',  ( 811.3240766477731540, -100.3726999360622187, -355.6651683502462902 ) ) ;
#33072 = CARTESIAN_POINT ( 'NONE',  ( 783.0433043558608688, -120.8965053807781800, -315.1538015810313027 ) ) ;
#33073 = CARTESIAN_POINT ( 'NONE',  ( 749.8865473780648472, -140.5328690171417634, 322.1177392798429082 ) ) ;
#33074 = CARTESIAN_POINT ( 'NONE',  ( 791.9812246680005501, -452.6346026584191691, 361.9419747391813189 ) ) ;
#33075 = CIRCLE ( 'NONE', #2090, 10.00000000000000888 ) ;
#33076 = CARTESIAN_POINT ( 'NONE',  ( 746.0683387631852383, -163.4419599262325846, 331.3260364891676204 ) ) ;
#33077 = CARTESIAN_POINT ( 'NONE',  ( 794.9819416627830151, -36.99823902205679360, -319.9864689768909898 ) ) ;
#33078 = CARTESIAN_POINT ( 'NONE',  ( 789.9200121543843807, -121.9874144716872593, -317.0176451133914384 ) ) ;
#33079 = CARTESIAN_POINT ( 'NONE',  ( 759.9864689768902508, -122.0891481129656171, -354.9819416627836404 ) ) ;
#33080 = CARTESIAN_POINT ( 'NONE',  ( 754.8072714833581358, -124.8164208402383508, 338.1981804954720587 ) ) ;
#33081 = CARTESIAN_POINT ( 'NONE',  ( 756.7813123517142913, -427.9874144716862929, -329.9779781133712504 ) ) ;
#33082 = EDGE_CURVE ( 'NONE', #23353, #20535, #38604, .T. ) ;
#33084 = CARTESIAN_POINT ( 'NONE',  ( 758.0580252608178853, -270.4527844766014937, 328.0187753319985404 ) ) ;
#33083 = CARTESIAN_POINT ( 'NONE',  ( 805.1927285166397041, -256.8164208402379245, 341.8018195045277707 ) ) ;
#33085 = DIRECTION ( 'NONE',  ( -0.000000000000000000, 1.000000000000000000, -0.000000000000000000 ) ) ;
#33086 = ORIENTED_EDGE ( 'NONE', *, *, #24162, .F. ) ;
#33087 = CARTESIAN_POINT ( 'NONE',  ( 766.7756240680305382, 9.467130982857780097, 361.5560724626415663 ) ) ;
#33088 = EDGE_LOOP ( 'NONE', ( #29668, #39911, #35241, #21826, #11935, #38660, #17641, #13847 ) ) ;
#33089 = CARTESIAN_POINT ( 'NONE',  ( 747.2067596250078623, -171.1800572038745543, 352.2312462859687230 ) ) ;
#33090 = CARTESIAN_POINT ( 'NONE',  ( 787.5531968255692163, -309.8272453906070041, 316.1348686366205811 ) ) ;
#33091 = CARTESIAN_POINT ( 'NONE',  ( 804.9511171171677688, -389.8055962898682765, 335.8780910478229202 ) ) ;
#33092 = ORIENTED_EDGE ( 'NONE', *, *, #6544, .F. ) ;
#33093 = CARTESIAN_POINT ( 'NONE',  ( 761.4292242960306112, -89.46360902697134065, -323.2154366446414429 ) ) ;
#33094 = CARTESIAN_POINT ( 'NONE',  ( 774.6312213355098493, -287.3618753856923718, -364.6798772138717482 ) ) ;
#33095 = VERTEX_POINT ( 'NONE', #7803 ) ;
#33096 = CARTESIAN_POINT ( 'NONE',  ( 768.0187753319979720, -392.6346026584193396, -318.0580252608186242 ) ) ;
#33097 = CARTESIAN_POINT ( 'NONE',  ( 781.7834795799800531, -34.81642084023861372, -315.0636971347436202 ) ) ;
#33098 = CARTESIAN_POINT ( 'NONE',  ( 758.6633372737375112, -260.5328690171413086, 326.9102291470432533 ) ) ;
#33099 = CARTESIAN_POINT ( 'NONE',  ( 759.9999999999992042, -462.9681489794448339, 317.6393202250019954 ) ) ;
#33100 = CARTESIAN_POINT ( 'NONE',  ( 200.7583438952258916, 294.6698570112193920, -274.9999999999999432 ) ) ;
#33101 = CARTESIAN_POINT ( 'NONE',  ( 788.6739635108323228, -31.64542720878970883, -373.9316612368139090 ) ) ;
#33102 = CARTESIAN_POINT ( 'NONE',  ( -779.9999999999993179, -513.1383975375929367, -367.9999999999999432 ) ) ;
#33103 = ORIENTED_EDGE ( 'NONE', *, *, #36003, .T. ) ;
#33104 = CARTESIAN_POINT ( 'NONE',  ( 747.6481478633932056, -301.0999726633342561, -353.4146539503763620 ) ) ;
#33105 = CARTESIAN_POINT ( 'NONE',  ( 786.2694204179717872, -165.2817908451529547, 305.1769319972829067 ) ) ;
#33106 = VECTOR ( 'NONE', #27759, 1000.000000000000000 ) ;
#33108 = CARTESIAN_POINT ( 'NONE',  ( 801.9419747391806368, -282.4527844766014937, -351.9812246680014027 ) ) ;
#33107 = CARTESIAN_POINT ( 'NONE',  ( 786.4999999999993179, -365.3551492539851893, -18.13243251470705886 ) ) ;
#33109 = CARTESIAN_POINT ( 'NONE',  ( 761.4292242960306112, -161.4636090269711133, -323.2154366446414429 ) ) ;
#33110 = EDGE_CURVE ( 'NONE', #7841, #42952, #18424, .T. ) ;
#33111 = CARTESIAN_POINT ( 'NONE',  ( -728.8365100919714905, 230.0000000000001705, -199.9999999999890861 ) ) ;
#33112 = CARTESIAN_POINT ( 'NONE',  ( 771.2368401574024119, -13.44195992623305713, -374.2805881961240857 ) ) ;
#33113 = CARTESIAN_POINT ( 'NONE',  ( 810.7187646348534145, -354.4527844766012095, -356.7737145352016341 ) ) ;
#33114 = ADVANCED_FACE ( 'NONE', ( #404 ), #14507, .F. ) ;
#33115 = CARTESIAN_POINT ( 'NONE',  ( -784.4999999999993179, 22.32581219114657856, 895.6886905569881492 ) ) ;
#33116 = CARTESIAN_POINT ( 'NONE',  ( 767.8955696845333705, -48.45278447660219712, 362.1676090361162323 ) ) ;
#33117 = CARTESIAN_POINT ( 'NONE',  ( 809.0717654672305343, -268.9181544815162397, 360.1688906516309885 ) ) ;
#33118 = CARTESIAN_POINT ( 'NONE',  ( 805.9055244015594326, -243.6237781080504590, -315.8990559732753240 ) ) ;
#33119 = CARTESIAN_POINT ( 'NONE',  ( 744.7301800767019131, -268.8164208402378108, 337.4774526936615757 ) ) ;
#33120 = CARTESIAN_POINT ( 'NONE',  ( 801.9858362298568863, -435.0783235625953580, -312.7379699480935642 ) ) ;
#33121 = DIRECTION ( 'NONE',  ( 0.000000000000000000, 0.000000000000000000, -1.000000000000000000 ) ) ;
#33122 = CARTESIAN_POINT ( 'NONE',  ( 772.4999999999993179, -512.9681489794448908, 309.9999999999998863 ) ) ;
#33123 = CARTESIAN_POINT ( 'NONE',  ( 762.1405469898971887, -361.5436935675103882, 357.8594530101015607 ) ) ;
#33124 = CARTESIAN_POINT ( 'NONE',  ( 783.0745993439762742, -128.1908817542439465, 365.1016975059196739 ) ) ;
#33125 = CARTESIAN_POINT ( 'NONE',  ( 779.4709603349208464, -24.35105083532392811, -314.7162404726379918 ) ) ;
#33126 = DIRECTION ( 'NONE',  ( 1.000000000000000000, 0.000000000000000000, -0.000000000000000000 ) ) ;
#33127 = DIRECTION ( 'NONE',  ( 0.000000000000000000, 0.7071067811865474617, 0.7071067811865474617 ) ) ;
#33128 = CARTESIAN_POINT ( 'NONE',  ( 767.8955696845333705, -408.4527844766009252, 362.1676090361162323 ) ) ;
#33129 = ORIENTED_EDGE ( 'NONE', *, *, #9748, .T. ) ;
#33130 = CARTESIAN_POINT ( 'NONE',  ( 799.4546378042377910, -321.0783235625956991, -356.1575198192848006 ) ) ;
#33131 = CARTESIAN_POINT ( 'NONE',  ( 800.0135310231082713, -158.0891481129655176, 325.0180583372163028 ) ) ;
#33132 = CARTESIAN_POINT ( 'NONE',  ( 791.1614460488616487, -323.2601417444138860, -373.5763878283158874 ) ) ;
#33133 = FACE_OUTER_BOUND ( 'NONE', #40016, .T. ) ;
#33134 = ORIENTED_EDGE ( 'NONE', *, *, #28866, .T. ) ;
#33135 = CARTESIAN_POINT ( 'NONE',  ( 764.8639956371174549, -344.0891481129647786, 319.7806653035542013 ) ) ;
#33136 = VECTOR ( 'NONE', #23321, 1000.000000000000000 ) ;
#33137 = CARTESIAN_POINT ( 'NONE',  ( 769.1273215169530886, -70.71468719896014932, -317.4527132478988847 ) ) ;
#33138 = ORIENTED_EDGE ( 'NONE', *, *, #2980, .F. ) ;
#33139 = CARTESIAN_POINT ( 'NONE',  ( 571.1634899080285095, 229.9999999999999432, -199.9999999999981526 ) ) ;
#33140 = CARTESIAN_POINT ( 'NONE',  ( 745.0891759886404770, -172.2709662947836478, -342.4968714119734159 ) ) ;
#33141 = CARTESIAN_POINT ( 'NONE',  ( 759.0252816721024374, -96.99823902205660886, 368.0189434323527280 ) ) ;
#33142 = ORIENTED_EDGE ( 'NONE', *, *, #11632, .T. ) ;
#33143 = CARTESIAN_POINT ( 'NONE',  ( 797.6776695296629214, -163.5436935675109567, -357.6776695296636603 ) ) ;
#33144 = ORIENTED_EDGE ( 'NONE', *, *, #12906, .T. ) ;
#33145 = CARTESIAN_POINT ( 'NONE',  ( 796.1575198192839480, -438.0090635724247932, -359.4546378042384163 ) ) ;
#33146 = CARTESIAN_POINT ( 'NONE',  ( 788.8264449731200330, 2.819942796124898177, 363.6646147819171233 ) ) ;
#33147 = CARTESIAN_POINT ( 'NONE',  ( 769.1273215169530886, -166.7146871989598367, 317.4527132478988847 ) ) ;
#33149 = DIRECTION ( 'NONE',  ( 0.000000000000000000, -1.000000000000000000, 1.586032892321651891E-15 ) ) ;
#33148 = CARTESIAN_POINT ( 'NONE',  ( 772.4999999999993179, -512.9681489794448908, 350.0000000000000000 ) ) ;
#33150 = EDGE_CURVE ( 'NONE', #15014, #1382, #23447, .T. ) ;
#33151 = ORIENTED_EDGE ( 'NONE', *, *, #25839, .F. ) ;
#33152 = CARTESIAN_POINT ( 'NONE',  ( 804.6971507214547046, -435.2817908451521021, -344.0799538623459739 ) ) ;
#33153 = LINE ( 'NONE', #12125, #22592 ) ;
#33154 = CARTESIAN_POINT ( 'NONE',  ( 810.4231160770870019, -192.5545181178801215, -321.9338519418446936 ) ) ;
#33155 = CARTESIAN_POINT ( 'NONE',  ( 747.6481478633932056, -85.09997266333499510, 353.4146539503763620 ) ) ;
#33157 = CARTESIAN_POINT ( 'NONE',  ( 778.2165204200184689, -190.8164208402381234, -364.9363028652563230 ) ) ;
#33156 = CARTESIAN_POINT ( 'NONE',  ( 759.9999999999992042, -462.9681489794448339, 309.9999999999998863 ) ) ;
#33158 = CARTESIAN_POINT ( 'NONE',  ( 795.9930595647434757, -339.0783235625956422, -320.7433823573372820 ) ) ;
#33159 = FACE_OUTER_BOUND ( 'NONE', #35410, .T. ) ;
#33160 = CARTESIAN_POINT ( 'NONE',  ( 810.4231160770870019, -216.5545181178800931, -321.9338519418446936 ) ) ;
#33161 = CARTESIAN_POINT ( 'NONE',  ( 879.9999999999990905, 50.81038600091414281, -210.0000000000000000 ) ) ;
#33162 = FACE_BOUND ( 'NONE', #44155, .T. ) ;
#33163 = CARTESIAN_POINT ( 'NONE',  ( 766.9102291470427417, -42.55451811788057626, -318.6633372737382501 ) ) ;
#33164 = ADVANCED_FACE ( 'NONE', ( #30161, #41250 ), #9606, .F. ) ;
#33165 = CARTESIAN_POINT ( 'NONE',  ( 804.1105419155481968, -411.8272453906067199, 347.6308680596136469 ) ) ;
#33166 = CARTESIAN_POINT ( 'NONE',  ( 801.1904061080338124, -236.0891481129652334, -368.3070685750236066 ) ) ;
#33167 = CARTESIAN_POINT ( 'NONE',  ( 761.4292242960306112, -233.4636090269708575, 323.2154366446414429 ) ) ;
#33168 = CARTESIAN_POINT ( 'NONE',  ( -879.9999999999992042, 240.0000000000002274, -224.9999999999999716 ) ) ;
#33169 = CARTESIAN_POINT ( 'NONE',  ( 756.5762568750052424, -27.18005720387500901, -348.7366044899774238 ) ) ;
#33170 = AXIS2_PLACEMENT_3D ( 'NONE', #14170, #42585, #17649 ) ;
#33171 = CARTESIAN_POINT ( 'NONE',  ( 744.6391490659812007, -182.7363362996983369, 338.7502325331110455 ) ) ;
#33172 = CARTESIAN_POINT ( 'NONE',  ( 805.9055244015594326, -147.6237781080508285, -315.8990559732753240 ) ) ;
#33173 = CARTESIAN_POINT ( 'NONE',  ( 767.7687537140311633, -143.9073299311473590, 372.7932403749916830 ) ) ;
#33174 = CARTESIAN_POINT ( 'NONE',  ( 746.8695393053150156, -365.9073299311465917, -327.6429770376306010 ) ) ;
#33175 = CARTESIAN_POINT ( 'NONE',  ( 454.7528517110262101, 229.9999999999999432, -122.7905160835442615 ) ) ;
#33176 = CARTESIAN_POINT ( 'NONE',  ( -773.4999999999993179, -512.9681489794448908, -339.9999999999999432 ) ) ;
#33177 = CARTESIAN_POINT ( 'NONE',  ( 767.8955696845333705, -264.4527844766016074, 362.1676090361162323 ) ) ;
#33178 = CARTESIAN_POINT ( 'NONE',  ( 793.9708237608222134, -22.91815448151701062, 319.2295555964448681 ) ) ;
#33179 = EDGE_CURVE ( 'NONE', #42944, #26579, #43782, .T. ) ;
#33180 = CARTESIAN_POINT ( 'NONE',  ( 804.4286716492782716, -401.3618753856920307, -345.3141322388244703 ) ) ;
#33181 = CARTESIAN_POINT ( 'NONE',  ( 758.8095938919642549, -440.0891481129644944, -311.6929314249763365 ) ) ;
#33183 = EDGE_CURVE ( 'NONE', #21203, #28948, #16536, .T. ) ;
#33182 = CARTESIAN_POINT ( 'NONE',  ( 571.1634899080285095, 229.9999999999999432, -199.9999999999981526 ) ) ;
#33184 = CARTESIAN_POINT ( 'NONE',  ( 746.7653713866222915, -41.26014174441479554, 351.0478386215610271 ) ) ;
#33185 = VERTEX_POINT ( 'NONE', #26471 ) ;
#33186 = CARTESIAN_POINT ( 'NONE',  ( 761.2382568024794409, -207.6237781080506295, -356.9571628226838129 ) ) ;
#33187 = CARTESIAN_POINT ( 'NONE',  ( 804.9363028652555840, -16.27096629478413092, 338.2165204200192079 ) ) ;
#33188 = CARTESIAN_POINT ( 'NONE',  ( 773.7943932421234194, -215.8055962898687881, -305.5313806188329409 ) ) ;
#33189 = CARTESIAN_POINT ( 'NONE',  ( 837.2824899080285377, 256.4999999999998863, -199.9999999999999432 ) ) ;
#33190 = CARTESIAN_POINT ( 'NONE',  ( 745.1769319972822814, -329.8055962898683902, 346.2694204179732083 ) ) ;
#33191 = ORIENTED_EDGE ( 'NONE', *, *, #16139, .T. ) ;
#33192 = CARTESIAN_POINT ( 'NONE',  ( 759.7806653035534055, -150.9982390220563957, -324.8639956371180801 ) ) ;
#33193 = CARTESIAN_POINT ( 'NONE',  ( 794.9819416627830151, -324.9982390220559409, 319.9864689768909898 ) ) ;
#33194 = CARTESIAN_POINT ( 'NONE',  ( 755.2512626584698410, -79.54369356751119824, -315.2512626584710915 ) ) ;
#33195 = CARTESIAN_POINT ( 'NONE',  ( 792.1044303154646968, -60.45278447660216159, -317.8323909638837677 ) ) ;
#33196 = VERTEX_POINT ( 'NONE', #19770 ) ;
#33197 = CARTESIAN_POINT ( 'NONE',  ( 786.5483106153019435, -7.645427208789786100, -364.1601925771022366 ) ) ;
#33198 = ORIENTED_EDGE ( 'NONE', *, *, #25832, .F. ) ;
#33199 = CARTESIAN_POINT ( 'NONE',  ( 763.8424801807145741, -306.0090635724252479, -320.5453621957614700 ) ) ;
#33200 = EDGE_CURVE ( 'NONE', #16297, #14962, #40785, .T. ) ;
#33202 = CARTESIAN_POINT ( 'NONE',  ( 776.9254006560222479, -356.1908817542432075, 314.8983024940802125 ) ) ;
#33201 = CARTESIAN_POINT ( 'NONE',  ( 788.8264449731200330, -69.18005720387488111, 363.6646147819171233 ) ) ;
#33205 = CARTESIAN_POINT ( 'NONE',  ( 761.9338519418445230, -326.5328690171411381, 370.4231160770881957 ) ) ;
#33204 = CARTESIAN_POINT ( 'NONE',  ( -829.9999999999992042, 290.0000000000001705, -319.9999999999996021 ) ) ;
#33203 = CARTESIAN_POINT ( 'NONE',  ( 805.0032342141413437, -421.5436935675101040, 314.9967657858572352 ) ) ;
#33206 = EDGE_CURVE ( 'NONE', #42149, #19960, #23667, .T. ) ;
#33207 = CARTESIAN_POINT ( 'NONE',  ( 745.1769319972822814, -89.80559628986918597, 346.2694204179732083 ) ) ;
#33208 = CARTESIAN_POINT ( 'NONE',  ( 784.1219089521767955, -309.2817908451525568, -315.0488828828318333 ) ) ;
#33209 = CARTESIAN_POINT ( 'NONE',  ( 802.1676090361156639, -302.6346026584196238, -327.8955696845344505 ) ) ;
#33210 = CARTESIAN_POINT ( 'NONE',  ( 801.9419747391806368, -138.4527844766019200, -351.9812246680014027 ) ) ;
#33211 = CARTESIAN_POINT ( 'NONE',  ( 772.5602148656447525, -417.7255117493283478, 305.7998596910095443 ) ) ;
#33213 = CYLINDRICAL_SURFACE ( 'NONE', #29285, 10.00000000000000888 ) ;
#33212 = PLANE ( 'NONE',  #34415 ) ;
#33214 = CARTESIAN_POINT ( 'NONE',  ( 802.2119215644370342, -102.0090635724258448, -367.5423716828165084 ) ) ;
#33215 = PLANE ( 'NONE',  #16743 ) ;
#33217 = EDGE_CURVE ( 'NONE', #10766, #11542, #2210, .T. ) ;
#33216 = DIRECTION ( 'NONE',  ( 1.000000000000000000, 4.625929269271485914E-16, 0.000000000000000000 ) ) ;
#33218 = CARTESIAN_POINT ( 'NONE',  ( 755.1538015810308480, -302.1908817542433781, 343.0433043558613804 ) ) ;
#33219 = VERTEX_POINT ( 'NONE', #29936 ) ;
#33220 = CARTESIAN_POINT ( 'NONE',  ( 796.7737145352015204, -140.6346026584201070, -370.7187646348536987 ) ) ;
#33221 = CARTESIAN_POINT ( 'NONE',  ( 879.9999999999990905, 479.9999999999998863, -199.9999999999999716 ) ) ;
#33222 = CARTESIAN_POINT ( 'NONE',  ( 746.4236121716829757, -87.82724539060770041, 328.8385539511384650 ) ) ;
#33223 = CARTESIAN_POINT ( 'NONE',  ( 787.4397851343537695, -285.7255117493286889, -374.2001403089903988 ) ) ;
#33224 = CARTESIAN_POINT ( 'NONE',  ( 767.6429770376291799, -441.1800572038736163, -306.8695393053162093 ) ) ;
#33225 = CARTESIAN_POINT ( 'NONE',  ( 803.4237431249931660, -111.1800572038747532, 331.2633955100225194 ) ) ;
#33226 = CARTESIAN_POINT ( 'NONE',  ( 798.0661480581538854, -338.5328690171411381, -309.5768839229118043 ) ) ;
#33227 = CARTESIAN_POINT ( 'NONE',  ( 759.0252816721024374, -72.99823902205667991, -368.0189434323527280 ) ) ;
#33228 = CARTESIAN_POINT ( 'NONE',  ( 772.4468031744293057, -9.827245390607961539, 363.8651313633793620 ) ) ;
#33229 = CARTESIAN_POINT ( 'NONE',  ( 745.0891759886404770, -364.2709662947830793, -342.4968714119734159 ) ) ;
#33230 = CARTESIAN_POINT ( 'NONE',  ( 1238.921997096861332, 430.0000000000002842, -320.0000000000000568 ) ) ;
#33231 = CARTESIAN_POINT ( 'NONE',  ( 766.7756240680305382, -398.5328690171409107, 361.5560724626415663 ) ) ;
#33232 = ORIENTED_EDGE ( 'NONE', *, *, #21631, .F. ) ;
#33233 = CARTESIAN_POINT ( 'NONE',  ( 801.9858362298568863, -123.0783235625963385, -312.7379699480935642 ) ) ;
#33234 = LINE ( 'NONE', #38627, #12263 ) ;
#33235 = CARTESIAN_POINT ( 'NONE',  ( 812.6845335610512393, -247.9874144716867761, 353.5525998758768651 ) ) ;
#33236 = CARTESIAN_POINT ( 'NONE',  ( 755.3201227861273992, -51.72551174932947049, 345.3687786644892981 ) ) ;
#33237 = EDGE_LOOP ( 'NONE', ( #9224, #18326, #38767, #25900 ) ) ;
#33238 = CARTESIAN_POINT ( 'NONE',  ( 801.3366627262608972, -248.5328690171414223, -353.0897708529566899 ) ) ;
#33239 = CARTESIAN_POINT ( 'NONE',  ( 757.8323909638827445, -218.6346026584197944, 352.1044303154654358 ) ) ;
#33240 = CARTESIAN_POINT ( 'NONE',  ( 808.0189434323515343, 9.910851887033969021, -319.0252816721025511 ) ) ;
#33241 = CARTESIAN_POINT ( 'NONE',  ( 745.1769319972822814, -65.80559628986925702, -346.2694204179732083 ) ) ;
#33242 = ORIENTED_EDGE ( 'NONE', *, *, #14716, .T. ) ;
#33243 = ORIENTED_EDGE ( 'NONE', *, *, #22728, .F. ) ;
#33244 = CARTESIAN_POINT ( 'NONE',  ( 797.8822607201568644, -390.5545181178794678, -370.1134526219340160 ) ) ;
#33245 = CARTESIAN_POINT ( 'NONE',  ( 812.7932403749906598, -327.1800572038741279, 327.7687537140311633 ) ) ;
#33246 = CARTESIAN_POINT ( 'NONE',  ( 795.6651683502461765, -34.71468719896025590, 371.3240766477733814 ) ) ;
#33247 = CARTESIAN_POINT ( 'NONE',  ( 759.0159684113467620, -208.9181544815164102, -325.8855110935213020 ) ) ;
#33248 = CARTESIAN_POINT ( 'NONE',  ( 765.0180583372156207, -168.9982390220563673, -360.0135310231089534 ) ) ;
#33249 = CARTESIAN_POINT ( 'NONE',  ( 800.0135310231082713, -374.0891481129647786, -325.0180583372163028 ) ) ;
#33250 = ORIENTED_EDGE ( 'NONE', *, *, #4320, .F. ) ;
#33251 = CARTESIAN_POINT ( 'NONE',  ( 785.3687786644884454, -227.3618753856925707, 315.3201227861279676 ) ) ;
#33252 = CARTESIAN_POINT ( 'NONE',  ( 795.1360043628807261, -116.0891481129656029, -360.2193346964456282 ) ) ;
#33253 = ORIENTED_EDGE ( 'NONE', *, *, #6120, .F. ) ;
#33254 = CARTESIAN_POINT ( 'NONE',  ( 763.0537975583475827, -336.4527844766012095, 371.0346526505627480 ) ) ;
#33255 = DIRECTION ( 'NONE',  ( 1.644774851296528363E-16, -1.000000000000000000, 0.000000000000000000 ) ) ;
#33256 = CARTESIAN_POINT ( 'NONE',  ( 803.8651313633788504, -365.2601417444137155, 332.4468031744301015 ) ) ;
#33257 = CARTESIAN_POINT ( 'NONE',  ( 571.1634899080285095, 258.0939999999999372, -199.9999999999981526 ) ) ;
#33258 = CARTESIAN_POINT ( 'NONE',  ( 181.1634899080285948, 240.0000000000000284, -197.2499999999955662 ) ) ;
#33259 = CARTESIAN_POINT ( 'NONE',  ( 759.0159684113467620, -208.9181544815164102, 325.8855110935213020 ) ) ;
#33260 = CARTESIAN_POINT ( 'NONE',  ( 791.9812246680005501, -68.63460265842033436, 361.9419747391813189 ) ) ;
#33261 = VERTEX_POINT ( 'NONE', #44019 ) ;
#33262 = CARTESIAN_POINT ( 'NONE',  ( 771.3260364891663130, -403.6454272087884760, -306.0683387631859773 ) ) ;
#33263 = CARTESIAN_POINT ( 'NONE',  ( 804.7487373415286811, -19.54369356751139364, -364.7487373415288516 ) ) ;
#33264 = CARTESIAN_POINT ( 'NONE',  ( 773.3843516231979720, -229.4419599262323572, 364.4086373105754433 ) ) ;
#33265 = CARTESIAN_POINT ( 'NONE',  ( 805.1927285166397041, -400.8164208402373561, -341.8018195045277707 ) ) ;
#33266 = CARTESIAN_POINT ( 'NONE',  ( 797.6776695296629214, -19.54369356751139364, -357.6776695296636603 ) ) ;
#33267 = CARTESIAN_POINT ( 'NONE',  ( 813.1304606946830518, -425.9073299311463074, 352.3570229623690580 ) ) ;
#33268 = DIRECTION ( 'NONE',  ( -0.000000000000000000, 1.000000000000000000, -0.000000000000000000 ) ) ;
#33269 = CARTESIAN_POINT ( 'NONE',  ( 805.2837595273609850, -266.7363362996981095, -340.5290396650784714 ) ) ;
#33270 = CARTESIAN_POINT ( 'NONE',  ( 744.7301800767019131, -148.8164208402382656, -337.4774526936615757 ) ) ;
#33271 = CARTESIAN_POINT ( 'NONE',  ( 796.7737145352015204, -44.63460265842040542, 370.7187646348536987 ) ) ;
#33272 = CARTESIAN_POINT ( 'NONE',  ( 755.2512626584698410, -127.5436935675110561, 315.2512626584710915 ) ) ;
#33273 = CARTESIAN_POINT ( 'NONE',  ( 795.1616405723528942, 16.45630643248848912, -314.3282859078202591 ) ) ;
#33274 = CARTESIAN_POINT ( 'NONE',  ( 1238.921997096861332, 430.0000000000002842, -320.0000000000000568 ) ) ;
#33275 = DIRECTION ( 'NONE',  ( -0.3826814224632280603, -1.110223024625159854E-14, 0.9238803650373355048 ) ) ;
#33276 = CARTESIAN_POINT ( 'NONE',  ( 782.4968714119720516, -370.8164208402375834, 305.0891759886411023 ) ) ;
#33277 = CARTESIAN_POINT ( 'NONE',  ( 781.7834795799800531, -322.8164208402377540, -315.0636971347436202 ) ) ;
#33278 = CARTESIAN_POINT ( 'NONE',  ( 766.7756240680305382, 9.467130982857780097, 361.5560724626415663 ) ) ;
#33279 = CARTESIAN_POINT ( 'NONE',  ( 755.8894580844503253, -207.8272453906073451, 332.3691319403863531 ) ) ;
#33280 = CARTESIAN_POINT ( 'NONE',  ( 773.7305795820266212, -105.2817908451530968, -374.8230680027170365 ) ) ;
#33281 = CARTESIAN_POINT ( 'NONE',  ( 801.3366627262608972, -128.5328690171417634, -353.0897708529566899 ) ) ;
#33282 = CARTESIAN_POINT ( 'NONE',  ( 778.7502325331095108, -144.3510508353235764, 304.6391490659818828 ) ) ;
#33283 = CARTESIAN_POINT ( 'NONE',  ( 758.0580252608178853, -438.4527844766009821, 328.0187753319985404 ) ) ;
#33284 = CARTESIAN_POINT ( 'NONE',  ( 797.8594530101008786, -37.54369356751132614, -322.1405469898980982 ) ) ;
#33285 = CARTESIAN_POINT ( 'NONE',  ( 789.9200121543843807, -145.9874144716871740, -317.0176451133914384 ) ) ;
#33286 = CARTESIAN_POINT ( 'NONE',  ( 768.0187753319979720, -128.6346026584201354, -318.0580252608186242 ) ) ;
#33287 = CARTESIAN_POINT ( 'NONE',  ( 785.3687786644884454, -131.3618753856928834, 315.3201227861279676 ) ) ;
#33288 = CARTESIAN_POINT ( 'NONE',  ( 756.1443688327750579, 26.37622189194863509, -314.3581564841659315 ) ) ;
#33290 = CARTESIAN_POINT ( 'NONE',  ( 785.3141322388236176, -261.7255117493288026, 364.4286716492789537 ) ) ;
#33289 = CARTESIAN_POINT ( 'NONE',  ( 759.7806653035534055, -270.9982390220561115, 324.8639956371180801 ) ) ;
#33291 = LINE ( 'NONE', #1636, #9422 ) ;
#33292 = VERTEX_POINT ( 'NONE', #1741 ) ;
#33293 = CARTESIAN_POINT ( 'NONE',  ( 790.8726784830453198, 13.28531280103958423, 362.5472867521010585 ) ) ;
#33294 = CARTESIAN_POINT ( 'NONE',  ( 760.0363995740630116, -274.9181544815161828, -368.7758568127991907 ) ) ;
#33295 = VERTEX_POINT ( 'NONE', #44252 ) ;
#33296 = DIRECTION ( 'NONE',  ( 0.000000000000000000, 0.000000000000000000, 1.000000000000000000 ) ) ;
#33297 = CARTESIAN_POINT ( 'NONE',  ( 796.9462024416508257, -180.4527844766017495, 308.9653473494370246 ) ) ;
#33298 = CARTESIAN_POINT ( 'NONE',  ( 790.9844846989617508, -286.3726999360617356, 317.2208543904092721 ) ) ;
#33299 = CARTESIAN_POINT ( 'NONE',  ( 800.7704444035546203, -388.1692326535045936, 326.0291762391768771 ) ) ;
#33300 = ORIENTED_EDGE ( 'NONE', *, *, #14016, .T. ) ;
#33301 = CARTESIAN_POINT ( 'NONE',  ( 804.4086373105744769, -97.64542720878949922, -333.3843516231986541 ) ) ;
#33302 = CARTESIAN_POINT ( 'NONE',  ( 762.3223304703356007, -295.5436935675105588, -322.3223304703362828 ) ) ;
#33303 = EDGE_LOOP ( 'NONE', ( #27221, #26861, #44711, #10008 ) ) ;
#33304 = CARTESIAN_POINT ( 'NONE',  ( 765.0180583372156207, -408.9982390220556567, -360.0135310231089534 ) ) ;
#33305 = CARTESIAN_POINT ( 'NONE',  ( 788.8264449731200330, -93.18005720387481006, -363.6646147819171233 ) ) ;
#33306 = CARTESIAN_POINT ( 'NONE',  ( 770.0799878456142551, -277.9874144716867477, 362.9823548866085616 ) ) ;
#33307 = CARTESIAN_POINT ( 'NONE',  ( 794.9999999999993179, 205.0000000000000568, -255.0000000000000000 ) ) ;
#33308 = DIRECTION ( 'NONE',  ( -0.000000000000000000, 0.000000000000000000, -1.000000000000000000 ) ) ;
#33309 = CARTESIAN_POINT ( 'NONE',  ( 813.5763878283155464, -3.827245390607979303, -351.1614460488615350 ) ) ;
#33310 = LINE ( 'NONE', #8619, #10657 ) ;
#33311 = EDGE_LOOP ( 'NONE', ( #14042, #40732, #1884, #15477 ) ) ;
#33312 = CARTESIAN_POINT ( 'NONE',  ( 768.9521613784389729, -297.8272453906070041, -373.2346286133773106 ) ) ;
#33314 = CARTESIAN_POINT ( 'NONE',  ( 802.1676090361156639, -278.6346026584196807, -327.8955696845344505 ) ) ;
#33313 = DIRECTION ( 'NONE',  ( 0.000000000000000000, 1.000000000000000000, 3.700743415417198493E-16 ) ) ;
#33315 = FILL_AREA_STYLE ('',( #2341 ) ) ;
#33316 = CARTESIAN_POINT ( 'NONE',  ( 780.5236548040995785, -140.7363362996984506, -314.9735926884559944 ) ) ;
#33317 = CARTESIAN_POINT ( 'NONE',  ( 804.7487373415286811, -19.54369356751139364, 364.7487373415288516 ) ) ;
#33318 = PRESENTATION_LAYER_ASSIGNMENT (  '', '', ( #25201 ) ) ;
#33319 = CARTESIAN_POINT ( 'NONE',  ( 786.4999999999993179, -544.8427095258973623, -350.0000000000000000 ) ) ;
#33320 = CARTESIAN_POINT ( 'NONE',  ( 763.0537975583476964, -360.4527844766011526, -371.0346526505628617 ) ) ;
#33321 =( NAMED_UNIT ( * ) PLANE_ANGLE_UNIT ( ) SI_UNIT ( $, .RADIAN. ) );
#33322 = CARTESIAN_POINT ( 'NONE',  ( 762.3223304703356007, -31.54369356751135456, 322.3223304703362828 ) ) ;
#33323 = CARTESIAN_POINT ( 'NONE',  ( 805.6418435158337843, -269.4636090269708006, 363.8556311672236916 ) ) ;
#33324 = CARTESIAN_POINT ( 'NONE',  ( 763.0537975583475827, -264.4527844766016074, 371.0346526505627480 ) ) ;
#33325 = CARTESIAN_POINT ( 'NONE',  ( 782.5225473063381969, 1.729033705215812011, -375.2698199232970637 ) ) ;
#33326 = LINE ( 'NONE', #29424, #26888 ) ;
#33327 = LINE ( 'NONE', #44872, #8493 ) ;
#33328 = CARTESIAN_POINT ( 'NONE',  ( 804.4286716492782716, -353.3618753856922012, 345.3141322388244703 ) ) ;
#33329 = CARTESIAN_POINT ( 'NONE',  ( 757.0176451133909268, -109.0999726633349241, 349.9200121543848354 ) ) ;
#33330 = CARTESIAN_POINT ( 'NONE',  ( 789.9200121543843807, -25.98741447168755769, -317.0176451133914384 ) ) ;
#33331 = PLANE ( 'NONE',  #12921 ) ;
#33332 = PLANE ( 'NONE',  #25517 ) ;
#33333 = CARTESIAN_POINT ( 'NONE',  ( 814.8230680027162407, -125.8055962898690581, 333.7305795820267917 ) ) ;
#33334 = CARTESIAN_POINT ( 'NONE',  ( 791.9812246680005501, -380.6346026584192828, 361.9419747391813189 ) ) ;
#33335 = ORIENTED_EDGE ( 'NONE', *, *, #31752, .F. ) ;
#33336 = CARTESIAN_POINT ( 'NONE',  ( 754.9735926884551418, -330.3510508353229511, -340.5236548041000333 ) ) ;
#33337 = CARTESIAN_POINT ( 'NONE',  ( 759.7806653035534055, -150.9982390220563957, 324.8639956371180801 ) ) ;
#33338 = UNCERTAINTY_MEASURE_WITH_UNIT (LENGTH_MEASURE( 1.000000000000000082E-05 ), #12966, 'distance_accuracy_value', 'NONE');
#33339 = CARTESIAN_POINT ( 'NONE',  ( 752.4576283171824116, -333.0783235625956991, -317.7880784355627952 ) ) ;
#33340 = DIRECTION ( 'NONE',  ( 1.000000000000000000, -0.000000000000000000, -0.000000000000000000 ) ) ;
#33341 = ORIENTED_EDGE ( 'NONE', *, *, #26355, .F. ) ;
#33342 = CARTESIAN_POINT ( 'NONE',  ( 791.9812246680005501, -356.6346026584193964, 361.9419747391813189 ) ) ;
#33343 = ORIENTED_EDGE ( 'NONE', *, *, #39725, .F. ) ;
#33344 = CARTESIAN_POINT ( 'NONE',  ( 939.9999999999992042, 74.99999999999984368, -350.0000000000000000 ) ) ;
#33345 = EDGE_CURVE ( 'NONE', #20722, #6854, #16301, .T. ) ;
#33346 = CARTESIAN_POINT ( 'NONE',  ( 772.4837098697144029, -191.3618753856925991, -374.5518280994205611 ) ) ;
#33347 = CARTESIAN_POINT ( 'NONE',  ( 745.7998596910086917, -77.36187538569302546, 332.5602148656461168 ) ) ;
#33348 = ORIENTED_EDGE ( 'NONE', *, *, #33200, .T. ) ;
#33349 = CIRCLE ( 'NONE', #13448, 8.025000000000003908 ) ;
#33350 = CARTESIAN_POINT ( 'NONE',  ( 778.2165204200184689, -190.8164208402381234, -364.9363028652563230 ) ) ;
#33351 = ORIENTED_EDGE ( 'NONE', *, *, #25533, .F. ) ;
#33352 = CARTESIAN_POINT ( 'NONE',  ( 793.0897708529556667, -414.5545181178795247, -361.3366627262616362 ) ) ;
#33353 = CARTESIAN_POINT ( 'NONE',  ( 767.7687537140311633, -263.9073299311469327, 372.7932403749916830 ) ) ;
#33354 = CARTESIAN_POINT ( 'NONE',  ( 783.0433043558608688, -168.8965053807780237, 315.1538015810313027 ) ) ;
#33356 = CARTESIAN_POINT ( 'NONE',  ( 879.9999999999990905, 479.9999999999998863, -199.9999999999999716 ) ) ;
#33355 = DIRECTION ( 'NONE',  ( -0.000000000000000000, -1.110223024625155554E-15, -1.000000000000000000 ) ) ;
#33357 = ORIENTED_EDGE ( 'NONE', *, *, #37373, .F. ) ;
#33358 = CARTESIAN_POINT ( 'NONE',  ( 798.5707757039680246, -413.4636090269704027, -356.7845633553585003 ) ) ;
#33359 = CARTESIAN_POINT ( 'NONE',  ( 200.7583438952259485, 394.6698570112193920, -224.9999999999999716 ) ) ;
#33360 = CARTESIAN_POINT ( 'NONE',  ( 813.5763878283155464, -195.8272453906074304, -351.1614460488615350 ) ) ;
#33361 = CARTESIAN_POINT ( 'NONE',  ( 805.6418435158337843, -53.46360902697146855, 363.8556311672236916 ) ) ;
#33363 = CARTESIAN_POINT ( 'NONE',  ( 762.1405469898971887, -193.5436935675108714, -357.8594530101015607 ) ) ;
#33362 = DIRECTION ( 'NONE',  ( 0.000000000000000000, -1.000000000000000000, 0.000000000000000000 ) ) ;
#33364 = CARTESIAN_POINT ( 'NONE',  ( 755.0488828828309806, -377.8055962898682765, -344.1219089521771934 ) ) ;
#33365 = DIRECTION ( 'NONE',  ( -0.000000000000000000, -0.000000000000000000, 1.000000000000000000 ) ) ;
#33366 = CARTESIAN_POINT ( 'NONE',  ( 799.9636004259356241, -214.9181544815164386, -311.2241431872006956 ) ) ;
#33367 = CYLINDRICAL_SURFACE ( 'NONE', #29660, 30.00000000000008171 ) ;
#33368 = FACE_OUTER_BOUND ( 'NONE', #5280, .T. ) ;
#33369 = CARTESIAN_POINT ( 'NONE',  ( 793.0897708529556667, -54.55451811788054783, -361.3366627262616362 ) ) ;
#33370 = CARTESIAN_POINT ( 'NONE',  ( 775.8780910478218402, -417.2817908451522158, 364.9511171171680530 ) ) ;
#33371 = VECTOR ( 'NONE', #12866, 1000.000000000000000 ) ;
#33372 = CARTESIAN_POINT ( 'NONE',  ( 805.0032342141413437, -253.5436935675105588, -314.9967657858572352 ) ) ;
#33373 = CARTESIAN_POINT ( 'NONE',  ( 799.9999999999993179, 205.0000000000000568, 360.0000000000000000 ) ) ;
#33374 = LINE ( 'NONE', #1719, #29776 ) ;
#33375 = CARTESIAN_POINT ( 'NONE',  ( 805.1927285166397041, -64.81642084023852135, -341.8018195045277707 ) ) ;
#33376 = CARTESIAN_POINT ( 'NONE',  ( 813.5763878283155464, -195.8272453906074304, 351.1614460488615350 ) ) ;
#33377 = CARTESIAN_POINT ( 'NONE',  ( 813.2346286133761168, -125.2601417444145255, -328.9521613784389160 ) ) ;
#33378 = CARTESIAN_POINT ( 'NONE',  ( 758.8095938919642549, -152.0891481129655460, 311.6929314249763365 ) ) ;
#33379 = CARTESIAN_POINT ( 'NONE',  ( 745.7998596910086917, -365.3618753856920875, -332.5602148656461168 ) ) ;
#33380 = DIRECTION ( 'NONE',  ( -1.880165489482579047E-16, -1.000000000000000000, -0.000000000000000000 ) ) ;
#33381 = CARTESIAN_POINT ( 'NONE',  ( 754.8072714833581358, -244.8164208402378961, 338.1981804954720587 ) ) ;
#33382 = CIRCLE ( 'NONE', #31892, 9.999999999999982236 ) ;
#33383 = CARTESIAN_POINT ( 'NONE',  ( 796.9571628226829034, -23.46360902697155026, 321.2382568024804641 ) ) ;
#33384 = CARTESIAN_POINT ( 'NONE',  ( 762.1405469898971887, -385.5436935675102745, -357.8594530101015607 ) ) ;
#33385 = DIRECTION ( 'NONE',  ( -0.000000000000000000, 1.000000000000000000, -0.000000000000000000 ) ) ;
#33386 = CARTESIAN_POINT ( 'NONE',  ( 767.6429770376289525, -441.1800572038735027, -306.8695393053162093 ) ) ;
#33387 = DIRECTION ( 'NONE',  ( -1.000000000000000000, -0.000000000000000000, -0.000000000000000000 ) ) ;
#33388 = CARTESIAN_POINT ( 'NONE',  ( 803.2186876482843445, -79.98741447168740137, 350.0220218866286928 ) ) ;
#33389 = ORIENTED_EDGE ( 'NONE', *, *, #12822, .T. ) ;
#33390 = ADVANCED_FACE ( 'NONE', ( #5221 ), #8709, .F. ) ;
#33391 = MANIFOLD_SOLID_BREP ( 'Boss-Extrude22', #7004 ) ;
#33392 = CARTESIAN_POINT ( 'NONE',  ( 793.2243759319678702, -218.5328690171414792, -318.4439275373583200 ) ) ;
#33393 = CARTESIAN_POINT ( 'NONE',  ( 803.4237431249931660, -63.18005720387488822, 331.2633955100225194 ) ) ;
#33394 = CARTESIAN_POINT ( 'NONE',  ( 800.1688906516307043, -226.1692326535051052, -369.0717654672308186 ) ) ;
#33395 = CARTESIAN_POINT ( 'NONE',  ( 999.9999999999992042, -590.0000000000001137, -350.0000000000000000 ) ) ;
#33396 = CARTESIAN_POINT ( 'NONE',  ( 746.7653713866222915, -353.2601417444137724, 351.0478386215610271 ) ) ;
#33397 = VERTEX_POINT ( 'NONE', #5906 ) ;
#33398 = CARTESIAN_POINT ( 'NONE',  ( 774.6312213355099630, -143.3618753856927697, -364.6798772138717482 ) ) ;
#33399 = CARTESIAN_POINT ( 'NONE',  ( 767.8955696845333705, -336.4527844766012095, 362.1676090361162323 ) ) ;
#33400 = EDGE_CURVE ( 'NONE', #45689, #911, #15844, .T. ) ;
#33401 = CARTESIAN_POINT ( 'NONE',  ( 814.9108240113580450, -88.27096629478390355, -337.5031285880265273 ) ) ;
#33402 = VECTOR ( 'NONE', #41448, 1000.000000000000000 ) ;
#33403 = CARTESIAN_POINT ( 'NONE',  ( 759.9864689768902508, -74.08914811296577341, -354.9819416627836404 ) ) ;
#33404 = ORIENTED_EDGE ( 'NONE', *, *, #22731, .T. ) ;
#33405 = CARTESIAN_POINT ( 'NONE',  ( 761.4292242960306112, 6.536390973028352924, -323.2154366446414429 ) ) ;
#33406 = PRODUCT_DEFINITION_FORMATION_WITH_SPECIFIED_SOURCE ( 'ANY', '', #38824, .NOT_KNOWN. ) ;
#33407 = CARTESIAN_POINT ( 'NONE',  ( 787.5531968255692163, -333.8272453906070041, -316.1348686366205811 ) ) ;
#33409 = CARTESIAN_POINT ( 'NONE',  ( 769.0155153010367712, -370.3726999360613377, 362.7791456095907279 ) ) ;
#33408 = CARTESIAN_POINT ( 'NONE',  ( 797.8594530101008786, -109.5436935675110988, 322.1405469898980982 ) ) ;
#33412 = CARTESIAN_POINT ( 'NONE',  ( 793.4146539503750546, -313.9874144716866908, 307.6481478633938877 ) ) ;
#33411 = DIRECTION ( 'NONE',  ( 1.000000000000000000, 0.000000000000000000, 0.000000000000000000 ) ) ;
#33410 = CARTESIAN_POINT ( 'NONE',  ( 751.9810565676468741, -434.0891481129646081, 360.9747183278973921 ) ) ;
#33413 = CARTESIAN_POINT ( 'NONE',  ( 771.2368401574024119, -109.4419599262327836, 374.2805881961240857 ) ) ;
#33414 = CARTESIAN_POINT ( 'NONE',  ( 799.2566176426618085, -336.0090635724251911, -324.0069404352559559 ) ) ;
#33415 = CARTESIAN_POINT ( 'NONE',  ( 771.2633955100217236, -311.9073299311468759, -363.4237431249939618 ) ) ;
#33416 = CARTESIAN_POINT ( 'NONE',  ( 758.0580252608178853, -150.4527844766018916, -328.0187753319985404 ) ) ;
#33417 = EDGE_CURVE ( 'NONE', #22578, #23899, #11343, .T. ) ;
#33418 = CARTESIAN_POINT ( 'NONE',  ( 813.1304606946830518, -425.9073299311463074, 352.3570229623690580 ) ) ;
#33420 = LINE ( 'NONE', #9167, #10848 ) ;
#33419 = CARTESIAN_POINT ( 'NONE',  ( 571.1634899080285095, 256.4999999999999432, -199.9999999999981526 ) ) ;
#33421 = EDGE_CURVE ( 'NONE', #22668, #518, #41710, .T. ) ;
#33422 = CARTESIAN_POINT ( 'NONE',  ( 773.7305795820266212, -129.2817908451530400, -374.8230680027170365 ) ) ;
#33423 = DIRECTION ( 'NONE',  ( 1.000000000000000000, 0.000000000000000000, 0.000000000000000000 ) ) ;
#33424 = DIRECTION ( 'NONE',  ( 0.000000000000000000, 0.000000000000000000, -1.000000000000000000 ) ) ;
#33425 = CARTESIAN_POINT ( 'NONE',  ( 804.4086373105744769, -289.6454272087889308, 333.3843516231986541 ) ) ;
#33426 = CARTESIAN_POINT ( 'NONE',  ( 755.0636971347428243, -172.2709662947836478, 341.7834795799807353 ) ) ;
#33427 = ORIENTED_EDGE ( 'NONE', *, *, #9097, .T. ) ;
#33428 = CARTESIAN_POINT ( 'NONE',  ( 763.0537975583476964, -144.4527844766018632, -371.0346526505628617 ) ) ;
#33429 = DIRECTION ( 'NONE',  ( 0.000000000000000000, 0.000000000000000000, -1.000000000000000000 ) ) ;
#33430 = CARTESIAN_POINT ( 'NONE',  ( 815.3608509340175488, -74.73633629969866377, 341.2497674668889545 ) ) ;
#33431 = CARTESIAN_POINT ( 'NONE',  ( 748.9653473494363425, -266.6346026584197375, -356.9462024416521331 ) ) ;
#33432 = CARTESIAN_POINT ( 'NONE',  ( 796.7737145352015204, -452.6346026584191691, -370.7187646348536987 ) ) ;
#33433 = CARTESIAN_POINT ( 'NONE',  ( 762.1405469898971887, -145.5436935675109851, 357.8594530101015607 ) ) ;
#33434 = VECTOR ( 'NONE', #37814, 1000.000000000000000 ) ;
#33435 = VERTEX_POINT ( 'NONE', #13988 ) ;
#33436 = CARTESIAN_POINT ( 'NONE',  ( 768.8385539511368734, -335.2601417444137724, -306.4236121716840557 ) ) ;
#33437 = VECTOR ( 'NONE', #36490, 1000.000000000000000 ) ;
#33438 = CARTESIAN_POINT ( 'NONE',  ( 777.4774526936600978, -82.27096629478388934, -304.7301800767027657 ) ) ;
#33439 = EDGE_CURVE ( 'NONE', #20663, #24719, #118, .T. ) ;
#33440 = CARTESIAN_POINT ( 'NONE',  ( 775.8780910478218402, -9.281790845153418346, 364.9511171171680530 ) ) ;
#33441 = CARTESIAN_POINT ( 'NONE',  ( 772.4837098697144029, -335.3618753856920307, -374.5518280994205611 ) ) ;
#33442 = DIRECTION ( 'NONE',  ( 0.000000000000000000, 0.000000000000000000, 1.000000000000000000 ) ) ;
#33443 = CARTESIAN_POINT ( 'NONE',  ( 798.7617431975189675, -387.6237781080499758, 323.0428371773161871 ) ) ;
#33444 = ORIENTED_EDGE ( 'NONE', *, *, #13291, .F. ) ;
#33445 = ADVANCED_FACE ( 'NONE', ( #42377, #6813, #38245 ), #10745, .F. ) ;
#33446 = CARTESIAN_POINT ( 'NONE',  ( 768.0187753319979720, -224.6346026584198228, -318.0580252608186242 ) ) ;
#33447 = CARTESIAN_POINT ( 'NONE',  ( 803.8556311672234642, -105.6237781080509421, -365.6418435158340117 ) ) ;
#33448 = DIRECTION ( 'NONE',  ( 1.000000000000000000, -1.880165489482579047E-16, 0.000000000000000000 ) ) ;
#33449 = CARTESIAN_POINT ( 'NONE',  ( 764.3348316497523456, -238.7146871989596661, 308.6759233522265617 ) ) ;
#33450 = CARTESIAN_POINT ( 'NONE',  ( 758.0580252608178853, -102.4527844766020337, 328.0187753319985404 ) ) ;
#33451 = ORIENTED_EDGE ( 'NONE', *, *, #2313, .F. ) ;
#33452 = AXIS2_PLACEMENT_3D ( 'NONE', #12162, #37548, #41021 ) ;
#33453 = CARTESIAN_POINT ( 'NONE',  ( 774.6858677611749044, -249.7255117493288594, 315.5713283507209894 ) ) ;
#33454 = EDGE_CURVE ( 'NONE', #27157, #36537, #7056, .T. ) ;
#33455 = CARTESIAN_POINT ( 'NONE',  ( 811.0346526505616112, 9.365397341579420498, -323.0537975583477532 ) ) ;
#33456 = CARTESIAN_POINT ( 'NONE',  ( 190.7583438952259485, 394.6698570112193920, -244.9999999999999716 ) ) ;
#33457 = ORIENTED_EDGE ( 'NONE', *, *, #23239, .T. ) ;
#33458 = VERTEX_POINT ( 'NONE', #20454 ) ;
#33459 = CARTESIAN_POINT ( 'NONE',  ( 812.3518521366052028, -385.0999726633340856, -326.5853460496235243 ) ) ;
#33460 = CARTESIAN_POINT ( 'NONE',  ( 795.1360043628807261, -236.0891481129651766, -360.2193346964456282 ) ) ;
#33461 = CARTESIAN_POINT ( 'NONE',  ( 796.9462024416508257, -324.4527844766013231, 308.9653473494370246 ) ) ;
#33462 = CARTESIAN_POINT ( 'NONE',  ( 756.1443688327750579, -45.62377810805114109, 314.3581564841659315 ) ) ;
#33463 = CARTESIAN_POINT ( 'NONE',  ( 804.8461984189677878, -218.1908817542437191, -336.9566956441385628 ) ) ;
#33464 = CARTESIAN_POINT ( 'NONE',  ( 758.0580252608178853, -222.4527844766016642, -328.0187753319985404 ) ) ;
#33465 = AXIS2_PLACEMENT_3D ( 'NONE', #40089, #33837, #1959 ) ;
#33466 = CARTESIAN_POINT ( 'NONE',  ( 792.1044303154646968, -396.4527844766010958, -317.8323909638837677 ) ) ;
#33467 = AXIS2_PLACEMENT_3D ( 'NONE', #28504, #42602, #10963 ) ;
#33468 = EDGE_LOOP ( 'NONE', ( #25708, #24376, #38640, #12012 ) ) ;
#33469 = CARTESIAN_POINT ( 'NONE',  ( 795.1360043628807261, -212.0891481129652902, 360.2193346964456282 ) ) ;
#33470 = CARTESIAN_POINT ( 'NONE',  ( 755.5713283507202505, -101.3618753856929544, -334.6858677611754729 ) ) ;
#33471 = ORIENTED_EDGE ( 'NONE', *, *, #32318, .F. ) ;
#33472 = CARTESIAN_POINT ( 'NONE',  ( 814.9108240113580450, -328.2709662947831362, 337.5031285880265273 ) ) ;
#33473 = DIRECTION ( 'NONE',  ( -1.000000000000000000, 0.000000000000000000, 0.000000000000000000 ) ) ;
#33474 = EDGE_CURVE ( 'NONE', #6928, #38375, #34542, .T. ) ;
#33475 = DIRECTION ( 'NONE',  ( 1.000000000000000000, 0.000000000000000000, 0.000000000000000000 ) ) ;
#33476 = CARTESIAN_POINT ( 'NONE',  ( 879.9999999999992042, 99.99999999999984368, 360.0000000000000000 ) ) ;
#33477 = CARTESIAN_POINT ( 'NONE',  ( 783.0745993439762742, -176.1908817542438328, 365.1016975059196739 ) ) ;
#33478 = CARTESIAN_POINT ( 'NONE',  ( 785.3687786644884454, -83.36187538569296862, 315.3201227861279676 ) ) ;
#33479 = VERTEX_POINT ( 'NONE', #27379 ) ;
#33480 = CARTESIAN_POINT ( 'NONE',  ( 786.2694204179717872, -453.2817908451519315, -305.1769319972829067 ) ) ;
#33481 = CARTESIAN_POINT ( 'NONE',  ( 815.2698199232962679, -40.81642084023859951, -342.5225473063383674 ) ) ;
#33482 = CARTESIAN_POINT ( 'NONE',  ( 790.8726784830453198, -250.7146871989595809, 362.5472867521010585 ) ) ;
#33483 = CARTESIAN_POINT ( 'NONE',  ( 758.0580252608178853, -390.4527844766011526, -328.0187753319985404 ) ) ;
#33484 = CARTESIAN_POINT ( 'NONE',  ( 755.5713283507202505, -5.361875385693257279, -334.6858677611754729 ) ) ;
#33485 = AXIS2_PLACEMENT_3D ( 'NONE', #24098, #31503, #45608 ) ;
#33486 = CARTESIAN_POINT ( 'NONE',  ( 792.2312462859673587, -419.9073299311465348, 307.2067596250082602 ) ) ;
#33487 = DIRECTION ( 'NONE',  ( -1.880165489482579047E-16, -1.000000000000000000, -0.000000000000000000 ) ) ;
#33488 = CARTESIAN_POINT ( 'NONE',  ( 783.0745993439762742, -296.1908817542434917, -365.1016975059196739 ) ) ;
#33489 = CARTESIAN_POINT ( 'NONE',  ( 812.7932403749906598, -159.1800572038746111, -327.7687537140311633 ) ) ;
#33490 = CARTESIAN_POINT ( 'NONE',  ( 805.0032342141412300, -61.54369356751124087, 314.9967657858571783 ) ) ;
#33491 = CARTESIAN_POINT ( 'NONE',  ( 772.4837098697144029, -143.3618753856927697, 374.5518280994205611 ) ) ;
#33492 = CARTESIAN_POINT ( 'NONE',  ( 779.9999999999992042, -462.9681489794448339, -339.9999999999999432 ) ) ;
#33493 = CARTESIAN_POINT ( 'NONE',  ( -37.63011601220122770, -544.8427095258973623, -369.9999999999999432 ) ) ;
#33494 = EDGE_CURVE ( 'NONE', #26364, #27491, #17456, .T. ) ;
#33495 = DIRECTION ( 'NONE',  ( 0.000000000000000000, 1.000000000000000000, 0.000000000000000000 ) ) ;
#33496 = CARTESIAN_POINT ( 'NONE',  ( 812.7932403749906598, -375.1800572038739574, 327.7687537140311633 ) ) ;
#33497 = CARTESIAN_POINT ( 'NONE',  ( 756.5762568750052424, -363.1800572038739006, -348.7366044899774238 ) ) ;
#33498 = EDGE_CURVE ( 'NONE', #41469, #11754, #41938, .T. ) ;
#33499 = CARTESIAN_POINT ( 'NONE',  ( 755.0488828828309806, 6.194403710130517382, 344.1219089521771934 ) ) ;
#33500 = AXIS2_PLACEMENT_3D ( 'NONE', #14908, #4506, #1030 ) ;
#33501 = CIRCLE ( 'NONE', #23159, 24.99999999999991118 ) ;
#33502 = CARTESIAN_POINT ( 'NONE',  ( 745.1792804349281596, -86.19088175424408860, -343.7566961878542884 ) ) ;
#33503 = CARTESIAN_POINT ( 'NONE',  ( 756.1348686366196716, -113.2601417444145682, -347.5531968255698416 ) ) ;
#33504 = CARTESIAN_POINT ( 'NONE',  ( 783.7566961878529810, -144.8965053807781089, 305.1792804349288417 ) ) ;
#33505 = CARTESIAN_POINT ( 'NONE',  ( 800.2193346964446619, -450.9982390220554294, 355.1360043628816925 ) ) ;
#33506 = CARTESIAN_POINT ( 'NONE',  ( 783.7566961878529810, -168.8965053807780237, 305.1792804349288417 ) ) ;
#33507 = CARTESIAN_POINT ( 'NONE',  ( 771.1735550268778070, -33.18005720387498769, -316.3353852180827630 ) ) ;
#33508 = CARTESIAN_POINT ( 'NONE',  ( 793.2243759319678702, -122.5328690171417918, -318.4439275373583200 ) ) ;
#33509 = CARTESIAN_POINT ( 'NONE',  ( 778.2165204200184689, -118.8164208402383508, -364.9363028652563230 ) ) ;
#33510 = ADVANCED_FACE ( 'NONE', ( #30851 ), #20891, .T. ) ;
#33511 = CARTESIAN_POINT ( 'NONE',  ( 781.8018195045266339, -142.2709662947837330, 365.1927285166406705 ) ) ;
#33512 = CARTESIAN_POINT ( 'NONE',  ( 763.2154366446407039, -429.6237781080499190, -321.4292242960311228 ) ) ;
#33513 = CARTESIAN_POINT ( 'NONE',  ( 755.0636971347428243, -268.2709662947833067, 341.7834795799807353 ) ) ;
#33514 = CYLINDRICAL_SURFACE ( 'NONE', #36007, 2.749999999999863665 ) ;
#33515 = VERTEX_POINT ( 'NONE', #9827 ) ;
#33516 = CARTESIAN_POINT ( 'NONE',  ( 765.8855110935204493, 25.83076734649409545, 319.0159684113471599 ) ) ;
#33517 = CARTESIAN_POINT ( 'NONE',  ( 791.0478386215596629, -285.8272453906071178, -306.7653713866226326 ) ) ;
#33518 = CIRCLE ( 'NONE', #44569, 9.999999999999982236 ) ;
#33519 = ORIENTED_EDGE ( 'NONE', *, *, #19907, .T. ) ;
#33520 = AXIS2_PLACEMENT_3D ( 'NONE', #45388, #24122, #41007 ) ;
#33521 = CARTESIAN_POINT ( 'NONE',  ( 810.7187646348534145, -234.4527844766016358, 356.7737145352016341 ) ) ;
#33522 = CARTESIAN_POINT ( 'NONE',  ( 784.1219089521767955, -309.2817908451525568, 315.0488828828318333 ) ) ;
#33523 = CARTESIAN_POINT ( 'NONE',  ( 779.4709603349208464, -408.3510508353227806, 314.7162404726379918 ) ) ;
#33524 = VERTEX_POINT ( 'NONE', #13767 ) ;
#33525 = CARTESIAN_POINT ( 'NONE',  ( 799.2566176426618085, -120.0090635724258021, -324.0069404352559559 ) ) ;
#33526 = CARTESIAN_POINT ( 'NONE',  ( 756.5762568750052424, -99.18005720387478164, -348.7366044899774238 ) ) ;
#33527 = CARTESIAN_POINT ( 'NONE',  ( 781.7834795799800531, -274.8164208402378108, -315.0636971347436202 ) ) ;
#33528 = ORIENTED_EDGE ( 'NONE', *, *, #17569, .F. ) ;
#33529 = CARTESIAN_POINT ( 'NONE',  ( 767.8955696845333705, -432.4527844766008684, -362.1676090361162323 ) ) ;
#33530 = CARTESIAN_POINT ( 'NONE',  ( 778.2165204200184689, -70.81642084023850714, -364.9363028652563230 ) ) ;
#33531 = CARTESIAN_POINT ( 'NONE',  ( 789.9200121543843807, -289.9874144716866908, 317.0176451133914384 ) ) ;
#33532 = DIRECTION ( 'NONE',  ( -1.000000000000000000, -0.000000000000000000, -0.000000000000000000 ) ) ;
#33533 = CARTESIAN_POINT ( 'NONE',  ( -66.63011601220125613, -365.3551492539851893, -18.13243251470705886 ) ) ;
#33534 = CIRCLE ( 'NONE', #16600, 8.025000000000003908 ) ;
#33535 = CARTESIAN_POINT ( 'NONE',  ( 791.9812246680005501, 3.365397341579444479, 361.9419747391813189 ) ) ;
#33536 = EDGE_LOOP ( 'NONE', ( #5626, #6437, #28477, #42777 ) ) ;
#33537 = CARTESIAN_POINT ( 'NONE',  ( 795.8262568251477660, -358.3726999360613945, -308.3538107759623585 ) ) ;
#33538 = VECTOR ( 'NONE', #41346, 1000.000000000000000 ) ;
#33539 = CARTESIAN_POINT ( 'NONE',  ( 807.2620300519052989, -216.0090635724255037, 318.0141637701419768 ) ) ;
#33541 = CARTESIAN_POINT ( 'NONE',  ( 803.4237431249931660, -303.1800572038740711, -331.2633955100225194 ) ) ;
#33540 = LINE ( 'NONE', #30079, #7685 ) ;
#33542 = CARTESIAN_POINT ( 'NONE',  ( 784.4999999999993179, -563.3203001761230553, -342.3463313526983143 ) ) ;
#33543 = CARTESIAN_POINT ( 'NONE',  ( 800.9840315886518738, -148.9181544815166092, -354.1144889064786412 ) ) ;
#33544 = CARTESIAN_POINT ( 'NONE',  ( 763.2262854647970016, -32.63460265842044095, 309.2812353651462445 ) ) ;
#33545 = LINE ( 'NONE', #12084, #22560 ) ;
#33546 = CARTESIAN_POINT ( 'NONE',  ( 805.0032342141413437, -397.5436935675101040, -314.9967657858572352 ) ) ;
#33547 = DIRECTION ( 'NONE',  ( 0.000000000000000000, 0.000000000000000000, -1.000000000000000000 ) ) ;
#33548 = CARTESIAN_POINT ( 'NONE',  ( 759.7806653035534055, -54.99823902205672255, 324.8639956371180801 ) ) ;
#33549 = CARTESIAN_POINT ( 'NONE',  ( 748.6759233522253680, -304.3726999360615082, 324.3348316497537098 ) ) ;
#33550 = CARTESIAN_POINT ( 'NONE',  ( 748.9653473494363425, -242.6346026584197659, 356.9462024416521331 ) ) ;
#33551 = CARTESIAN_POINT ( 'NONE',  ( 782.5225473063381969, -22.27096629478410250, -375.2698199232970637 ) ) ;
#33552 = DIRECTION ( 'NONE',  ( 0.000000000000000000, 0.000000000000000000, 1.000000000000000000 ) ) ;
#33553 = AXIS2_PLACEMENT_3D ( 'NONE', #40044, #33552, #26170 ) ;
#33554 = CARTESIAN_POINT ( 'NONE',  ( -338.8365100919713200, 260.0000000000001137, -199.9999999999917861 ) ) ;
#33555 = VECTOR ( 'NONE', #33365, 1000.000000000000000 ) ;
#33556 = CARTESIAN_POINT ( 'NONE',  ( 794.9819416627830151, -348.9982390220558273, 319.9864689768909898 ) ) ;
#33557 = CARTESIAN_POINT ( 'NONE',  ( 790.9844846989617508, -118.3726999360621619, 317.2208543904092721 ) ) ;
#33558 = CARTESIAN_POINT ( 'NONE',  ( 795.9930595647434757, -3.078323562596726681, -320.7433823573372820 ) ) ;
#33559 = DIRECTION ( 'NONE',  ( -0.3826814224632300032, 0.000000000000000000, 0.9238803650373347276 ) ) ;
#33560 = CARTESIAN_POINT ( 'NONE',  ( -598.8365100919716042, 240.0000000000001705, -197.2499999999901092 ) ) ;
#33561 = CARTESIAN_POINT ( 'NONE',  ( 762.1405469898971887, -409.5436935675101040, 357.8594530101015607 ) ) ;
#33562 = ORIENTED_EDGE ( 'NONE', *, *, #31441, .T. ) ;
#33563 = CARTESIAN_POINT ( 'NONE',  ( 804.9363028652555840, -40.27096629478405987, -338.2165204200192079 ) ) ;
#33564 = CIRCLE ( 'NONE', #2570, 2.749999999999891642 ) ;
#33565 = CARTESIAN_POINT ( 'NONE',  ( 790.8726784830453198, -322.7146871989593819, -362.5472867521010585 ) ) ;
#33567 = CARTESIAN_POINT ( 'NONE',  ( 755.5713283507202505, -173.3618753856927128, 334.6858677611754729 ) ) ;
#33566 = CARTESIAN_POINT ( 'NONE',  ( 755.3201227861273992, -171.7255117493291152, 345.3687786644892981 ) ) ;
#33568 = CARTESIAN_POINT ( 'NONE',  ( 811.6461892240364477, -340.7146871989592114, -324.1737431748509835 ) ) ;
#33569 = DIRECTION ( 'NONE',  ( -1.000000000000000000, 0.000000000000000000, 0.000000000000000000 ) ) ;
#33570 = VERTEX_POINT ( 'NONE', #41475 ) ;
#33571 = CARTESIAN_POINT ( 'NONE',  ( 756.3353852180819104, -365.9073299311465917, 331.1735550268788302 ) ) ;
#33572 = VECTOR ( 'NONE', #39550, 1000.000000000000000 ) ;
#33573 = ORIENTED_EDGE ( 'NONE', *, *, #19601, .T. ) ;
#33574 = CARTESIAN_POINT ( 'NONE',  ( -454.7528517110260964, 200.0000000000001137, 339.9999999999999432 ) ) ;
#33575 = CARTESIAN_POINT ( 'NONE',  ( 777.5031285880264704, -190.8164208402381234, -374.9108240113588408 ) ) ;
#33576 = CARTESIAN_POINT ( 'NONE',  ( 745.7998596910086917, -125.3618753856928834, 332.5602148656461168 ) ) ;
#33577 = ORIENTED_EDGE ( 'NONE', *, *, #23732, .T. ) ;
#33578 = CIRCLE ( 'NONE', #13676, 9.999999999999982236 ) ;
#33579 = CARTESIAN_POINT ( 'NONE',  ( 800.2193346964446619, -162.9982390220563673, -355.1360043628816925 ) ) ;
#33580 = ORIENTED_EDGE ( 'NONE', *, *, #31202, .T. ) ;
#33581 = CARTESIAN_POINT ( 'NONE',  ( 804.6798772138708955, 8.274488250670337663, -334.6312213355107019 ) ) ;
#33582 = AXIS2_PLACEMENT_3D ( 'NONE', #35491, #4328, #43346 ) ;
#33583 = CARTESIAN_POINT ( 'NONE',  ( 746.8695393053150156, -245.9073299311469896, 327.6429770376306010 ) ) ;
#33584 = CARTESIAN_POINT ( 'NONE',  ( 803.8651313633788504, -173.2601417444143692, 332.4468031744301015 ) ) ;
#33586 = CARTESIAN_POINT ( 'NONE',  ( 989.9999999999992042, 47.45399382421947365, 201.9999999999999432 ) ) ;
#33585 = LINE ( 'NONE', #19266, #37316 ) ;
#33587 = VECTOR ( 'NONE', #44878, 1000.000000000000000 ) ;
#33588 = EDGE_LOOP ( 'NONE', ( #25800, #26241, #29150, #36044 ) ) ;
#33589 = CARTESIAN_POINT ( 'NONE',  ( 786.5483106153019435, -415.6454272087885897, -364.1601925771022366 ) ) ;
#33590 = DIRECTION ( 'NONE',  ( 5.551115123125783688E-16, 1.000000000000000000, -0.000000000000000000 ) ) ;
#33591 = ORIENTED_EDGE ( 'NONE', *, *, #43788, .F. ) ;
#33592 = CARTESIAN_POINT ( 'NONE',  ( 799.9636004259356241, -238.9181544815163534, -311.2241431872006956 ) ) ;
#33593 = CARTESIAN_POINT ( 'NONE',  ( 748.6759233522253680, -88.37269993606226137, 324.3348316497537098 ) ) ;
#33595 = CARTESIAN_POINT ( 'NONE',  ( 762.3223304703356007, -199.5436935675108430, -322.3223304703362828 ) ) ;
#33594 = CARTESIAN_POINT ( 'NONE',  ( 51.16348990802859475, 256.5000000000000568, -197.2499999999946283 ) ) ;
#33596 = CARTESIAN_POINT ( 'NONE',  ( 804.9511171171677688, -365.8055962898682765, -335.8780910478229202 ) ) ;
#33597 = FACE_OUTER_BOUND ( 'NONE', #25584, .T. ) ;
#33598 = CARTESIAN_POINT ( 'NONE',  ( 760.0363995740630116, -226.9181544815163534, -368.7758568127991907 ) ) ;
#33599 = CARTESIAN_POINT ( 'NONE',  ( 831.1634899080286232, 256.4999999999998863, -199.9999999999999432 ) ) ;
#33600 = DIRECTION ( 'NONE',  ( 0.000000000000000000, 0.000000000000000000, 1.000000000000000000 ) ) ;
#33601 = CARTESIAN_POINT ( 'NONE',  ( 755.3028492785439312, -63.28179084515324604, -335.9200461376539693 ) ) ;
#33602 = CARTESIAN_POINT ( 'NONE',  ( 780.5236548040995785, -428.7363362996975980, 314.9735926884559944 ) ) ;
#33603 = CIRCLE ( 'NONE', #13702, 2.749999999999919176 ) ;
#33604 = CARTESIAN_POINT ( 'NONE',  ( 745.0891759886404770, -244.2709662947834204, -342.4968714119734159 ) ) ;
#33605 = CARTESIAN_POINT ( 'NONE',  ( 796.1575198192839480, -246.0090635724253900, 359.4546378042384163 ) ) ;
#33606 = DIRECTION ( 'NONE',  ( 1.000000000000000000, 0.000000000000000000, 0.000000000000000000 ) ) ;
#33607 = LINE ( 'NONE', #12374, #9138 ) ;
#33608 = CARTESIAN_POINT ( 'NONE',  ( 759.7806653035534055, -54.99823902205672255, -324.8639956371180801 ) ) ;
#33609 = AXIS2_PLACEMENT_3D ( 'NONE', #30177, #36886, #5700 ) ;
#33610 = CARTESIAN_POINT ( 'NONE',  ( 810.4231160770870019, -168.5545181178802352, 321.9338519418446936 ) ) ;
#33611 = CARTESIAN_POINT ( 'NONE',  ( 778.7502325331095108, -144.3510508353235764, -304.6391490659818828 ) ) ;
#33612 = CARTESIAN_POINT ( 'NONE',  ( 747.2067596250078623, -147.1800572038746395, 352.2312462859687230 ) ) ;
#33613 = CARTESIAN_POINT ( 'NONE',  ( 811.0346526505616112, -374.6346026584192828, -323.0537975583477532 ) ) ;
#33614 = AXIS2_PLACEMENT_3D ( 'NONE', #145, #24606, #13554 ) ;
#33615 = CARTESIAN_POINT ( 'NONE',  ( 762.3223304703356007, 16.45630643248849267, 322.3223304703362828 ) ) ;
#33616 = CARTESIAN_POINT ( 'NONE',  ( 778.1981804954714335, -250.2709662947832783, 314.8072714833589885 ) ) ;
#33617 = CARTESIAN_POINT ( 'NONE',  ( 754.7162404726377645, -38.73633629969877035, 339.4709603349214717 ) ) ;
#33618 = CARTESIAN_POINT ( 'NONE',  ( 800.0135310231082713, -398.0891481129647218, -325.0180583372163028 ) ) ;
#33619 = VECTOR ( 'NONE', #12762, 1000.000000000000114 ) ;
#33620 = CARTESIAN_POINT ( 'NONE',  ( 311.1634899080286232, 260.0000000000000000, -202.7499999999961915 ) ) ;
#33621 = CARTESIAN_POINT ( 'NONE',  ( 755.2512626584698410, -439.5436935675101040, -315.2512626584710915 ) ) ;
#33622 = DIRECTION ( 'NONE',  ( 0.000000000000000000, 0.000000000000000000, 1.000000000000000000 ) ) ;
#33623 = CARTESIAN_POINT ( 'NONE',  ( 765.8855110935204493, -94.16923265350555994, 319.0159684113471599 ) ) ;
#33624 = ORIENTED_EDGE ( 'NONE', *, *, #5239, .T. ) ;
#33625 = CARTESIAN_POINT ( 'NONE',  ( 755.8398074228967971, -211.4419599262324709, -333.4516893846970333 ) ) ;
#33626 = CARTESIAN_POINT ( 'NONE',  ( 755.5713283507202505, -125.3618753856928834, -334.6858677611754729 ) ) ;
#33627 = CARTESIAN_POINT ( 'NONE',  ( 755.5713283507202505, -53.36187538569310362, 334.6858677611754729 ) ) ;
#33628 = CARTESIAN_POINT ( 'NONE',  ( 746.0683387631852383, -235.4419599262323857, -331.3260364891676204 ) ) ;
#33629 =( NAMED_UNIT ( * ) SI_UNIT ( $, .STERADIAN. ) SOLID_ANGLE_UNIT ( ) );
#33630 = CARTESIAN_POINT ( 'NONE',  ( 744.8212110874229666, -378.8965053807772847, 336.2046728542121627 ) ) ;
#33631 = ORIENTED_EDGE ( 'NONE', *, *, #16139, .F. ) ;
#33632 = CARTESIAN_POINT ( 'NONE',  ( 803.4237431249931660, -183.1800572038744974, -331.2633955100225194 ) ) ;
#33633 = CARTESIAN_POINT ( 'NONE',  ( 781.8018195045266339, -358.2709662947829088, 365.1927285166406705 ) ) ;
#33634 = CARTESIAN_POINT ( 'NONE',  ( 792.3570229623688874, -69.18005720387488111, -373.1304606946836202 ) ) ;
#33635 = CARTESIAN_POINT ( 'NONE',  ( 768.0187753319979720, -80.63460265842029173, -318.0580252608186242 ) ) ;
#33636 = ORIENTED_EDGE ( 'NONE', *, *, #24136, .T. ) ;
#33637 = CARTESIAN_POINT ( 'NONE',  ( 769.9779781133707957, -19.09997266333520116, -316.7813123517150871 ) ) ;
#33638 = CIRCLE ( 'NONE', #41769, 20.00000000000001776 ) ;
#33639 = ORIENTED_EDGE ( 'NONE', *, *, #11876, .T. ) ;
#33640 = CARTESIAN_POINT ( 'NONE',  ( 755.3028492785439312, -351.2817908451523294, -335.9200461376539693 ) ) ;
#33642 = CARTESIAN_POINT ( 'NONE',  ( 790.0220218866281812, -391.0999726633340288, 363.2186876482849129 ) ) ;
#33641 = CARTESIAN_POINT ( 'NONE',  ( 762.1405469898971887, -97.54369356751112718, 357.8594530101015607 ) ) ;
#33643 = AXIS2_PLACEMENT_3D ( 'NONE', #25541, #39654, #8006 ) ;
#33646 = CARTESIAN_POINT ( 'NONE',  ( 788.7631598425961101, -337.4419599262319593, 305.7194118038759143 ) ) ;
#33645 = CARTESIAN_POINT ( 'NONE',  ( 784.4999999999993179, -544.8427095258973623, -350.0000000000000000 ) ) ;
#33644 = CARTESIAN_POINT ( 'NONE',  ( 758.8095938919644823, -440.0891481129645513, 311.6929314249762797 ) ) ;
#33647 = CARTESIAN_POINT ( 'NONE',  ( 748.3538107759620743, -112.7146871989600356, 355.8262568251490165 ) ) ;
#33648 = CARTESIAN_POINT ( 'NONE',  ( 793.9708237608222134, -334.9181544815160692, -319.2295555964448681 ) ) ;
#33649 = CARTESIAN_POINT ( 'NONE',  ( 758.0580252608178853, -318.4527844766014368, -328.0187753319985404 ) ) ;
#33650 = CARTESIAN_POINT ( 'NONE',  ( 791.9812246680005501, -164.6346026584200217, -361.9419747391813189 ) ) ;
#33651 = CARTESIAN_POINT ( 'NONE',  ( 745.1792804349281596, -14.19088175424431242, 343.7566961878542884 ) ) ;
#33652 = VECTOR ( 'NONE', #38874, 1000.000000000000114 ) ;
#33654 = DIRECTION ( 'NONE',  ( 0.000000000000000000, 0.000000000000000000, -1.000000000000000000 ) ) ;
#33653 = CARTESIAN_POINT ( 'NONE',  ( -208.8365100919714052, 260.0000000000001137, -199.9999999999926956 ) ) ;
#33655 = CARTESIAN_POINT ( 'NONE',  ( 754.8983024940795303, -258.8965053807777963, -336.9254006560228163 ) ) ;
#33656 = CARTESIAN_POINT ( 'NONE',  ( 764.1737431748507561, -106.3726999360621903, -371.6461892240376415 ) ) ;
#33657 = DIRECTION ( 'NONE',  ( -0.000000000000000000, 1.000000000000000000, -0.000000000000000000 ) ) ;
#33658 = DIRECTION ( 'NONE',  ( 0.000000000000000000, 0.000000000000000000, 1.000000000000000000 ) ) ;
#33659 = VECTOR ( 'NONE', #16377, 1000.000000000000000 ) ;
#33660 = EDGE_CURVE ( 'NONE', #45642, #41202, #31248, .T. ) ;
#33661 = CARTESIAN_POINT ( 'NONE',  ( 773.4516893846965786, -283.6454272087889308, 315.8398074228977066 ) ) ;
#33662 = CARTESIAN_POINT ( 'NONE',  ( 758.0580252608178853, -174.4527844766018063, 328.0187753319985404 ) ) ;
#33663 = ORIENTED_EDGE ( 'NONE', *, *, #37065, .F. ) ;
#33664 = CARTESIAN_POINT ( 'NONE',  ( 766.4474001241216001, -283.0999726633344267, 307.3154664389482491 ) ) ;
#33665 = CARTESIAN_POINT ( 'NONE',  ( 782.4968714119720516, -154.8164208402382371, -305.0891759886411023 ) ) ;
#33666 = FACE_OUTER_BOUND ( 'NONE', #10995, .T. ) ;
#33667 = CARTESIAN_POINT ( 'NONE',  ( 768.9521613784389729, -81.82724539060772884, 373.2346286133773106 ) ) ;
#33668 = CARTESIAN_POINT ( 'NONE',  ( 796.9462024416508257, -252.4527844766015789, -308.9653473494370246 ) ) ;
#33669 = EDGE_CURVE ( 'NONE', #34711, #28297, #45538, .T. ) ;
#33670 = DIRECTION ( 'NONE',  ( 0.000000000000000000, 0.000000000000000000, 1.000000000000000000 ) ) ;
#33671 = CARTESIAN_POINT ( 'NONE',  ( 788.8264449731200330, -141.1800572038746395, 363.6646147819171233 ) ) ;
#33672 = CARTESIAN_POINT ( 'NONE',  ( 771.2368401574024119, -325.4419599262320162, -374.2805881961240857 ) ) ;
#33673 = CIRCLE ( 'NONE', #31466, 2.749999999999842792 ) ;
#33674 = CARTESIAN_POINT ( 'NONE',  ( 745.0891759886404770, -100.2709662947838609, -342.4968714119734159 ) ) ;
#33675 = CARTESIAN_POINT ( 'NONE',  ( 786.5483106153019435, -7.645427208789786100, 364.1601925771022366 ) ) ;
#33676 = CARTESIAN_POINT ( 'NONE',  ( 758.8095938919642549, -368.0891481129647786, -311.6929314249763365 ) ) ;
#33677 = CARTESIAN_POINT ( 'NONE',  ( 779.9999999999992042, 126.4563064324884465, 339.9999999999999432 ) ) ;
#33678 = CARTESIAN_POINT ( 'NONE',  ( 766.7756240680305382, -422.5328690171408539, 361.5560724626415663 ) ) ;
#33679 = ORIENTED_EDGE ( 'NONE', *, *, #20069, .F. ) ;
#33680 = CIRCLE ( 'NONE', #1953, 6.118999999999985562 ) ;
#33681 = CARTESIAN_POINT ( 'NONE',  ( 807.5423716828161105, -105.0783235625964096, -362.2119215644372048 ) ) ;
#33682 = DIRECTION ( 'NONE',  ( -0.000000000000000000, 1.000000000000000000, -0.000000000000000000 ) ) ;
#33683 = CARTESIAN_POINT ( 'NONE',  ( 812.6845335610512393, -223.9874144716869182, 353.5525998758768651 ) ) ;
#33684 = CARTESIAN_POINT ( 'NONE',  ( 781.8018195045267476, -94.27096629478387513, 365.1927285166407273 ) ) ;
#33685 = ORIENTED_EDGE ( 'NONE', *, *, #41968, .F. ) ;
#33686 = AXIS2_PLACEMENT_3D ( 'NONE', #17865, #28485, #7946 ) ;
#33687 = EDGE_CURVE ( 'NONE', #28026, #33818, #34303, .T. ) ;
#33688 = CARTESIAN_POINT ( 'NONE',  ( 764.0069404352550464, -15.07832356259669560, -359.2566176426627180 ) ) ;
#33689 = CARTESIAN_POINT ( 'NONE',  ( 788.7366044899766848, -251.9073299311470748, 316.5762568750059813 ) ) ;
#33690 = VECTOR ( 'NONE', #6892, 1000.000000000000000 ) ;
#33691 = CARTESIAN_POINT ( 'NONE',  ( 768.8385539511368734, -431.2601417444136018, -306.4236121716840557 ) ) ;
#33692 = DIRECTION ( 'NONE',  ( -1.000000000000000000, 4.147566128926370535E-16, 0.000000000000000000 ) ) ;
#33693 = ORIENTED_EDGE ( 'NONE', *, *, #42741, .F. ) ;
#33694 = VERTEX_POINT ( 'NONE', #35223 ) ;
#33695 = CARTESIAN_POINT ( 'NONE',  ( 788.6739635108323228, -367.6454272087886466, -373.9316612368139090 ) ) ;
#33697 = CARTESIAN_POINT ( 'NONE',  ( 786.2056067578752163, -227.8055962898687596, 374.4686193811670023 ) ) ;
#33696 = CARTESIAN_POINT ( 'NONE',  ( 751.9810565676468741, -338.0891481129649492, 360.9747183278973921 ) ) ;
#33698 = CARTESIAN_POINT ( 'NONE',  ( 803.8556311672234642, -33.62377810805116951, 365.6418435158340117 ) ) ;
#33699 = CARTESIAN_POINT ( 'NONE',  ( 804.6971507214547046, -219.2817908451527558, -344.0799538623459739 ) ) ;
#33700 = CARTESIAN_POINT ( 'NONE',  ( 792.1044303154645831, -204.4527844766016926, -317.8323909638837677 ) ) ;
#33701 = CARTESIAN_POINT ( 'NONE',  ( 771.1735550268780344, -417.1800572038736732, -316.3353852180828198 ) ) ;
#33702 = VERTEX_POINT ( 'NONE', #2675 ) ;
#33703 = CARTESIAN_POINT ( 'NONE',  ( 804.6798772138708955, -207.7255117493289447, 334.6312213355107019 ) ) ;
#33704 = CARTESIAN_POINT ( 'NONE',  ( 795.1360043628807261, -92.08914811296568814, -360.2193346964456282 ) ) ;
#33705 = ORIENTED_EDGE ( 'NONE', *, *, #20446, .T. ) ;
#33706 = AXIS2_PLACEMENT_3D ( 'NONE', #4252, #32423, #773 ) ;
#33707 = CARTESIAN_POINT ( 'NONE',  ( 796.7737145352015204, -332.6346026584195101, 370.7187646348536987 ) ) ;
#33708 = ADVANCED_FACE ( 'NONE', ( #38461 ), #31747, .F. ) ;
#33709 = CARTESIAN_POINT ( 'NONE',  ( 787.0645410984409409, 17.59807796021646098, -310.5263297651933954 ) ) ;
#33710 = FACE_BOUND ( 'NONE', #43301, .T. ) ;
#33711 = CARTESIAN_POINT ( 'NONE',  ( -37.63011601220122770, -365.3551492539851893, -28.13243251470704109 ) ) ;
#33712 = EDGE_CURVE ( 'NONE', #1685, #10345, #13091, .T. ) ;
#33713 = CARTESIAN_POINT ( 'NONE',  ( 760.7433823573367135, -204.0090635724255606, 355.9930595647440441 ) ) ;
#33714 = CARTESIAN_POINT ( 'NONE',  ( 788.8264449731200330, -69.18005720387488111, 363.6646147819171233 ) ) ;
#33715 = VERTEX_POINT ( 'NONE', #45169 ) ;
#33716 = CARTESIAN_POINT ( 'NONE',  ( 771.3260364891663130, -451.6454272087884192, -306.0683387631859773 ) ) ;
#33717 = CARTESIAN_POINT ( 'NONE',  ( 751.6929314249750860, -30.99823902205680781, -318.8095938919659034 ) ) ;
#33718 = CARTESIAN_POINT ( 'NONE',  ( 760.5453621957607311, -261.0783235625959264, 323.8424801807151425 ) ) ;
#33719 = CARTESIAN_POINT ( 'NONE',  ( 803.4237431249931660, -399.1800572038738437, -331.2633955100225194 ) ) ;
#33720 = CARTESIAN_POINT ( 'NONE',  ( 803.4237431249931660, -15.18005720387504631, -331.2633955100225194 ) ) ;
#33721 = CARTESIAN_POINT ( 'NONE',  ( 777.4774526936600978, -418.2709662947827383, 304.7301800767027657 ) ) ;
#33722 = CARTESIAN_POINT ( 'NONE',  ( -78.83651009197140525, 240.0000000000000568, -197.2499999999937756 ) ) ;
#33723 = CARTESIAN_POINT ( 'NONE',  ( 754.7162404726377645, -278.7363362996980527, -339.4709603349214717 ) ) ;
#33724 = CARTESIAN_POINT ( 'NONE',  ( 814.2001403089898304, -161.3618753856927697, -347.4397851343538264 ) ) ;
#33725 = VECTOR ( 'NONE', #30349, 1000.000000000000000 ) ;
#33726 = ADVANCED_FACE ( 'NONE', ( #13529 ), #6460, .F. ) ;
#33727 = CARTESIAN_POINT ( 'NONE',  ( 801.1904061080336987, -92.08914811296568814, 368.3070685750235498 ) ) ;
#33728 = CARTESIAN_POINT ( 'NONE',  ( 763.2262854647970016, -128.6346026584201354, 309.2812353651462445 ) ) ;
#33729 = CARTESIAN_POINT ( 'NONE',  ( 793.9408588713487234, 16.45630643248830438, -314.6714885282663090 ) ) ;
#33730 = SURFACE_SIDE_STYLE ('',( #16169 ) ) ;
#33731 = CARTESIAN_POINT ( 'NONE',  ( 701.1634899080286232, 258.0939999999999372, -193.8809999999990623 ) ) ;
#33732 = CARTESIAN_POINT ( 'NONE',  ( 745.7998596910086917, -389.3618753856919739, 332.5602148656461168 ) ) ;
#33733 = CARTESIAN_POINT ( 'NONE',  ( 808.0189434323515343, -14.08914811296595460, 319.0252816721025511 ) ) ;
#33734 = CARTESIAN_POINT ( 'NONE',  ( 755.3201227861273992, -339.7255117493285184, -345.3687786644892981 ) ) ;
#33735 = CARTESIAN_POINT ( 'NONE',  ( 801.3366627262608972, 15.46713098285775878, 353.0897708529566899 ) ) ;
#33736 = CARTESIAN_POINT ( 'NONE',  ( 745.7194118038753459, -109.6454272087894566, -348.7631598425976449 ) ) ;
#33737 = CARTESIAN_POINT ( 'NONE',  ( 794.1144889064781864, -154.1692326535053894, -360.9840315886528401 ) ) ;
#33738 = ADVANCED_FACE ( 'NONE', ( #3121 ), #17210, .F. ) ;
#33739 = CARTESIAN_POINT ( 'NONE',  ( 814.8230680027162407, -125.8055962898690581, 333.7305795820267917 ) ) ;
#33740 = DIRECTION ( 'NONE',  ( -1.000000000000000000, -0.000000000000000000, 0.000000000000000000 ) ) ;
#33741 = EDGE_CURVE ( 'NONE', #15749, #37618, #16046, .T. ) ;
#33742 = CARTESIAN_POINT ( 'NONE',  ( 797.6776695296629214, -43.54369356751131903, -357.6776695296636603 ) ) ;
#33743 = CARTESIAN_POINT ( 'NONE',  ( 754.9735926884551418, -162.3510508353235196, -340.5236548041000333 ) ) ;
#33744 = VECTOR ( 'NONE', #35472, 1000.000000000000000 ) ;
#33745 = CARTESIAN_POINT ( 'NONE',  ( 759.9864689768902508, -146.0891481129655176, 354.9819416627836404 ) ) ;
#33746 = CARTESIAN_POINT ( 'NONE',  ( 805.0264073115434940, -438.3510508353226669, -339.4763451958999099 ) ) ;
#33747 = CARTESIAN_POINT ( 'NONE',  ( 788.8264449731201466, -285.1800572038741279, 363.6646147819170665 ) ) ;
#33748 = CARTESIAN_POINT ( 'NONE',  ( 767.9999999999992042, 205.0000000000000568, -319.9999999999999432 ) ) ;
#33749 = ORIENTED_EDGE ( 'NONE', *, *, #37930, .F. ) ;
#33750 = CARTESIAN_POINT ( 'NONE',  ( 805.0264073115434940, 17.64894916467593688, 339.4763451958999099 ) ) ;
#33751 = CARTESIAN_POINT ( 'NONE',  ( 754.3581564841646241, -281.4636090269706870, -316.1443688327762516 ) ) ;
#33752 = AXIS2_PLACEMENT_3D ( 'NONE', #8597, #19423, #22663 ) ;
#33753 = ORIENTED_EDGE ( 'NONE', *, *, #4642, .F. ) ;
#33754 = CARTESIAN_POINT ( 'NONE',  ( 767.6429770376291799, -225.1800572038743553, 306.8695393053162093 ) ) ;
#33755 = CARTESIAN_POINT ( 'NONE',  ( 800.9840315886518738, -316.9181544815160692, 354.1144889064786412 ) ) ;
#33756 = CARTESIAN_POINT ( 'NONE',  ( 775.9200461376533440, -407.8055962898681628, 315.3028492785443291 ) ) ;
#33757 = VERTEX_POINT ( 'NONE', #38943 ) ;
#33758 = CARTESIAN_POINT ( 'NONE',  ( 787.5531968255692163, -117.8272453906076151, -316.1348686366205811 ) ) ;
#33759 = CARTESIAN_POINT ( 'NONE',  ( 785.3141322388236176, -117.7255117493292715, -364.4286716492789537 ) ) ;
#33760 = CARTESIAN_POINT ( 'NONE',  ( 778.2165204200184689, -286.8164208402378677, -364.9363028652563230 ) ) ;
#33761 = ADVANCED_FACE ( 'NONE', ( #25275 ), #36139, .T. ) ;
#33762 = ORIENTED_EDGE ( 'NONE', *, *, #26079, .T. ) ;
#33763 = CARTESIAN_POINT ( 'NONE',  ( 800.2193346964447755, -426.9982390220554862, -355.1360043628815788 ) ) ;
#33764 = CARTESIAN_POINT ( 'NONE',  ( 756.3353852180819104, -77.90732993114757221, -331.1735550268788302 ) ) ;
#33765 = EDGE_CURVE ( 'NONE', #31920, #17901, #7739, .T. ) ;
#33766 = CARTESIAN_POINT ( 'NONE',  ( 763.2154366446407039, -309.6237781080502600, 321.4292242960311228 ) ) ;
#33767 = CARTESIAN_POINT ( 'NONE',  ( 779.9999999999992042, 16.45630643248849267, -339.9999999999999432 ) ) ;
#33768 = DIRECTION ( 'NONE',  ( 0.000000000000000000, 0.000000000000000000, 1.000000000000000000 ) ) ;
#33769 = EDGE_CURVE ( 'NONE', #5289, #20839, #8678, .T. ) ;
#33770 = DIRECTION ( 'NONE',  ( 1.000000000000000000, 0.000000000000000000, 0.000000000000000000 ) ) ;
#33771 = ORIENTED_EDGE ( 'NONE', *, *, #27181, .T. ) ;
#33772 = CARTESIAN_POINT ( 'NONE',  ( 757.7880784355613741, -354.0090635724250774, -312.4576283171834916 ) ) ;
#33773 = CARTESIAN_POINT ( 'NONE',  ( 810.4231160770870019, -216.5545181178800931, 321.9338519418446936 ) ) ;
#33774 = CARTESIAN_POINT ( 'NONE',  ( 774.6858677611749044, -297.7255117493286889, -315.5713283507209894 ) ) ;
#33775 = DIRECTION ( 'NONE',  ( -1.880165489482579047E-16, -1.000000000000000000, -0.000000000000000000 ) ) ;
#33776 = CARTESIAN_POINT ( 'NONE',  ( 804.4086373105744769, -169.6454272087892718, -333.3843516231986541 ) ) ;
#33777 = PRODUCT_DEFINITION ( 'UNKNOWN', '', #33406, #43063 ) ;
#33778 = CARTESIAN_POINT ( 'NONE',  ( 787.4397851343537695, -45.72551174932949181, 374.2001403089903988 ) ) ;
#33779 = DIRECTION ( 'NONE',  ( -1.880165489482579047E-16, -1.000000000000000000, -0.000000000000000000 ) ) ;
#33780 = CARTESIAN_POINT ( 'NONE',  ( 763.2262854647970016, -392.6346026584193396, -309.2812353651462445 ) ) ;
#33781 = CARTESIAN_POINT ( 'NONE',  ( 804.6798772138708955, -39.72551174932951312, 334.6312213355107019 ) ) ;
#33782 = AXIS2_PLACEMENT_3D ( 'NONE', #39054, #35799, #3710 ) ;
#33783 = CARTESIAN_POINT ( 'NONE',  ( 757.7880784355613741, -330.0090635724251342, 312.4576283171834916 ) ) ;
#33784 = CARTESIAN_POINT ( 'NONE',  ( 754.9967657858570647, -265.5436935675106156, 365.0032342141425374 ) ) ;
#33785 = CARTESIAN_POINT ( 'NONE',  ( 763.2262854647970016, -32.63460265842044095, -309.2812353651462445 ) ) ;
#33786 = CARTESIAN_POINT ( 'NONE',  ( 771.1735550268778070, -249.1800572038742416, -316.3353852180827630 ) ) ;
#33787 = DIRECTION ( 'NONE',  ( -0.000000000000000000, -1.110223024625155554E-15, -1.000000000000000000 ) ) ;
#33788 = CARTESIAN_POINT ( 'NONE',  ( 785.3687786644884454, -371.3618753856919739, 315.3201227861279676 ) ) ;
#33789 = CARTESIAN_POINT ( 'NONE',  ( 760.7433823573367135, -108.0090635724258448, 355.9930595647440441 ) ) ;
#33790 = CARTESIAN_POINT ( 'NONE',  ( 775.9200461376533440, -23.80559628986938847, -315.3028492785443291 ) ) ;
#33791 = CARTESIAN_POINT ( 'NONE',  ( 756.5762568750052424, -387.1800572038738437, 348.7366044899774238 ) ) ;
#33792 = DIRECTION ( 'NONE',  ( 0.000000000000000000, -1.000000000000000000, 0.000000000000000000 ) ) ;
#33793 = DIRECTION ( 'NONE',  ( -1.000000000000000000, -0.000000000000000000, 0.000000000000000000 ) ) ;
#33794 = CARTESIAN_POINT ( 'NONE',  ( 792.1044303154645831, -396.4527844766010389, 317.8323909638837677 ) ) ;
#33795 = ORIENTED_EDGE ( 'NONE', *, *, #18559, .T. ) ;
#33796 = CARTESIAN_POINT ( 'NONE',  ( 754.8983024940795303, -330.8965053807774552, -336.9254006560228163 ) ) ;
#33798 = CARTESIAN_POINT ( 'NONE',  ( 754.8072714833583632, -148.8164208402382656, 338.1981804954721156 ) ) ;
#33797 = CARTESIAN_POINT ( 'NONE',  ( 781.7834795799800531, -202.8164208402380950, 315.0636971347436202 ) ) ;
#33799 = CARTESIAN_POINT ( 'NONE',  ( 756.1443688327750579, -381.6237781080500326, -314.3581564841659315 ) ) ;
#33800 = DIRECTION ( 'NONE',  ( 0.000000000000000000, 0.000000000000000000, 1.000000000000000000 ) ) ;
#33801 = ORIENTED_EDGE ( 'NONE', *, *, #34615, .T. ) ;
#33802 = CARTESIAN_POINT ( 'NONE',  ( 759.9864689768902508, -362.0891481129648923, 354.9819416627836404 ) ) ;
#33803 = ORIENTED_EDGE ( 'NONE', *, *, #34811, .F. ) ;
#33804 =( NAMED_UNIT ( * ) SI_UNIT ( $, .STERADIAN. ) SOLID_ANGLE_UNIT ( ) );
#33805 = CARTESIAN_POINT ( 'NONE',  ( 796.7737145352015204, -212.6346026584198796, -370.7187646348536987 ) ) ;
#33806 = CARTESIAN_POINT ( 'NONE',  ( 810.7187646348534145, -114.4527844766020053, 356.7737145352016341 ) ) ;
#33807 = EDGE_LOOP ( 'NONE', ( #21765, #23045, #1383, #26002 ) ) ;
#33808 = CARTESIAN_POINT ( 'NONE',  ( 756.3353852180820240, -173.9073299311472454, -331.1735550268787733 ) ) ;
#33809 = EDGE_LOOP ( 'NONE', ( #28717, #33932, #19385, #8990 ) ) ;
#33810 = AXIS2_PLACEMENT_3D ( 'NONE', #9945, #17107, #30496 ) ;
#33811 = CARTESIAN_POINT ( 'NONE',  ( 756.5762568750052424, -339.1800572038740142, -348.7366044899774238 ) ) ;
#33812 = CARTESIAN_POINT ( 'NONE',  ( 802.9823548866075953, -457.0999726633339151, -330.0799878456151077 ) ) ;
#33813 = CARTESIAN_POINT ( 'NONE',  ( 814.2001403089898304, -257.3618753856924286, 347.4397851343538264 ) ) ;
#33814 = CARTESIAN_POINT ( 'NONE',  ( 760.5453621957607311, -189.0783235625961822, 323.8424801807151425 ) ) ;
#33816 = LINE ( 'NONE', #26431, #6349 ) ;
#33815 = CARTESIAN_POINT ( 'NONE',  ( 927.9999999999992042, 219.9999999999998863, 360.0000000000000000 ) ) ;
#33817 = DIRECTION ( 'NONE',  ( 0.000000000000000000, 0.000000000000000000, 1.000000000000000000 ) ) ;
#33818 = VERTEX_POINT ( 'NONE', #35444 ) ;
#33819 = CARTESIAN_POINT ( 'NONE',  ( 755.3028492785439312, -423.2817908451521589, -335.9200461376539693 ) ) ;
#33820 = DIRECTION ( 'NONE',  ( -0.000000000000000000, -1.000000000000000000, -0.000000000000000000 ) ) ;
#33821 = DIRECTION ( 'NONE',  ( 0.000000000000000000, 0.000000000000000000, -1.000000000000000000 ) ) ;
#33822 = ORIENTED_EDGE ( 'NONE', *, *, #39112, .F. ) ;
#33823 = CARTESIAN_POINT ( 'NONE',  ( 745.1792804349281596, -230.1908817542436338, -343.7566961878542884 ) ) ;
#33824 = CARTESIAN_POINT ( 'NONE',  ( 754.3581564841646241, -89.46360902697134065, 316.1443688327762516 ) ) ;
#33826 = CARTESIAN_POINT ( 'NONE',  ( 765.0180583372156207, -192.9982390220562820, -360.0135310231089534 ) ) ;
#33825 = CARTESIAN_POINT ( 'NONE',  ( 799.9999999999993179, 205.0000000000000568, -360.0000000000000000 ) ) ;
#33827 = CARTESIAN_POINT ( 'NONE',  ( 754.8983024940795303, -354.8965053807774552, -336.9254006560228163 ) ) ;
#33828 = CARTESIAN_POINT ( 'NONE',  ( 51.16348990802859475, 256.5000000000000568, -199.9999999999945146 ) ) ;
#33829 = CARTESIAN_POINT ( 'NONE',  ( 807.2620300519052989, -240.0090635724253900, -318.0141637701419768 ) ) ;
#33830 = CARTESIAN_POINT ( 'NONE',  ( 919.9999999999993179, 219.9999999999998863, 359.9749999999999659 ) ) ;
#33831 = DIRECTION ( 'NONE',  ( 0.000000000000000000, -0.3826834323650837866, -0.9238795325112891810 ) ) ;
#33832 = CARTESIAN_POINT ( 'NONE',  ( 804.6971507214547046, -99.28179084515313946, -344.0799538623459739 ) ) ;
#33833 = CARTESIAN_POINT ( 'NONE',  ( 761.4292242960306112, -449.4636090269702322, 323.2154366446414429 ) ) ;
#33834 = DIRECTION ( 'NONE',  ( -0.000000000000000000, 1.000000000000000000, -0.000000000000000000 ) ) ;
#33835 = CARTESIAN_POINT ( 'NONE',  ( 782.5225473063383106, -262.2709662947832499, -375.2698199232970637 ) ) ;
#33836 = CARTESIAN_POINT ( 'NONE',  ( -858.8365100919713768, 240.0000000000002274, -199.9999999999881481 ) ) ;
#33837 = DIRECTION ( 'NONE',  ( 0.000000000000000000, -0.9238795325112892920, 0.3826834323650836756 ) ) ;
#33838 = CARTESIAN_POINT ( 'NONE',  ( 804.6798772138708955, -63.72551174932939233, -334.6312213355107019 ) ) ;
#33839 = CARTESIAN_POINT ( 'NONE',  ( 745.1792804349281596, -230.1908817542436338, 343.7566961878542884 ) ) ;
#33840 = CARTESIAN_POINT ( 'NONE',  ( 808.7758568127978833, -172.1692326535052757, -320.0363995740631822 ) ) ;
#33841 = CARTESIAN_POINT ( 'NONE',  ( 782.4968714119720516, -154.8164208402382371, 305.0891759886411023 ) ) ;
#33842 = CARTESIAN_POINT ( 'NONE',  ( 763.2262854647970016, -392.6346026584193396, -309.2812353651462445 ) ) ;
#33843 = CARTESIAN_POINT ( 'NONE',  ( -789.9999999999992042, 205.0000000000000568, -339.9999999999999432 ) ) ;
#33844 = CARTESIAN_POINT ( 'NONE',  ( 771.2633955100217236, -263.9073299311469327, 363.4237431249939618 ) ) ;
#33845 = CARTESIAN_POINT ( 'NONE',  ( 784.1219089521767955, -45.28179084515329578, 315.0488828828318333 ) ) ;
#33846 = CARTESIAN_POINT ( 'NONE',  ( 758.0580252608178853, -390.4527844766011526, -328.0187753319985404 ) ) ;
#33847 = AXIS2_PLACEMENT_3D ( 'NONE', #12996, #2350, #27522 ) ;
#33848 = DIRECTION ( 'NONE',  ( 0.000000000000000000, 0.000000000000000000, -1.000000000000000000 ) ) ;
#33849 = DIRECTION ( 'NONE',  ( 0.000000000000000000, 0.7517448203044204691, 0.6594541114781790059 ) ) ;
#33851 = CARTESIAN_POINT ( 'NONE',  ( 795.1360043628807261, -308.0891481129650629, 360.2193346964456282 ) ) ;
#33850 = CARTESIAN_POINT ( 'NONE',  ( 804.1601925771018387, -79.44195992623286884, 346.5483106153029098 ) ) ;
#33852 = ORIENTED_EDGE ( 'NONE', *, *, #37624, .F. ) ;
#33853 = CARTESIAN_POINT ( 'NONE',  ( 758.6633372737375112, -236.5328690171414792, -326.9102291470432533 ) ) ;
#33854 = CARTESIAN_POINT ( 'NONE',  ( 774.6312213355099630, -47.36187538569312494, 364.6798772138717482 ) ) ;
#33855 = CARTESIAN_POINT ( 'NONE',  ( 800.1688906516307043, -250.1692326535050199, -369.0717654672308186 ) ) ;
#33856 = DIRECTION ( 'NONE',  ( -0.000000000000000000, -0.000000000000000000, -1.000000000000000000 ) ) ;
#33857 = CARTESIAN_POINT ( 'NONE',  ( 810.1134526219336749, -392.5328690171409107, 357.8822607201570349 ) ) ;
#33858 = EDGE_LOOP ( 'NONE', ( #23525, #11982, #30170, #5743 ) ) ;
#33859 = CARTESIAN_POINT ( 'NONE',  ( 792.2312462859673587, 12.09267006885214180, 307.2067596250082602 ) ) ;
#33860 = CARTESIAN_POINT ( 'NONE',  ( 803.6646147819161570, -161.9073299311472454, -348.8264449731210561 ) ) ;
#33861 = CARTESIAN_POINT ( 'NONE',  ( 804.6798772138708955, -375.7255117493283478, 334.6312213355107019 ) ) ;
#33862 = CARTESIAN_POINT ( 'NONE',  ( 796.7737145352015204, -92.63460265842026331, -370.7187646348536987 ) ) ;
#33863 = CARTESIAN_POINT ( 'NONE',  ( 757.8323909638828582, -74.63460265842030594, -352.1044303154654358 ) ) ;
#33864 = EDGE_LOOP ( 'NONE', ( #10837, #43029, #24220, #12248, #18761, #26755, #29163, #40118, #16146, #39688, #13984, #31938 ) ) ;
#33865 = CARTESIAN_POINT ( 'NONE',  ( 802.9823548866075953, -1.099972663335260226, -330.0799878456151077 ) ) ;
#33866 = EDGE_LOOP ( 'NONE', ( #10060, #38996, #8711, #31534 ) ) ;
#33867 = CARTESIAN_POINT ( 'NONE',  ( 802.5472867521000353, -364.3726999360614514, -350.8726784830461156 ) ) ;
#33869 = CARTESIAN_POINT ( 'NONE',  ( 755.3028492785439312, -399.2817908451522726, 335.9200461376539693 ) ) ;
#33868 = CARTESIAN_POINT ( 'NONE',  ( 774.6312213355099630, -95.36187538569294020, 364.6798772138717482 ) ) ;
#33872 = CARTESIAN_POINT ( 'NONE',  ( 768.8385539511368734, -311.2601417444139429, 306.4236121716840557 ) ) ;
#33871 = CARTESIAN_POINT ( 'NONE',  ( -200.7583438952259485, 394.6698570112193920, -224.9999999999999716 ) ) ;
#33870 = CARTESIAN_POINT ( 'NONE',  ( 777.4774526936600978, -418.2709662947828519, 304.7301800767028226 ) ) ;
#33873 = CARTESIAN_POINT ( 'NONE',  ( 776.9254006560222479, -308.1908817542434349, -314.8983024940802125 ) ) ;
#33874 = CARTESIAN_POINT ( 'NONE',  ( 756.3353852180819104, -317.9073299311468190, -331.1735550268788302 ) ) ;
#33875 = CARTESIAN_POINT ( 'NONE',  ( 771.3260364891663130, -139.6454272087893571, -306.0683387631859773 ) ) ;
#33876 = VECTOR ( 'NONE', #33949, 1000.000000000000000 ) ;
#33877 = CARTESIAN_POINT ( 'NONE',  ( 815.2698199232961542, -448.8164208402371855, 342.5225473063383106 ) ) ;
#33879 = CARTESIAN_POINT ( 'NONE',  ( -26.63011601220122060, -513.1383975375929367, -369.9999999999999432 ) ) ;
#33878 = CARTESIAN_POINT ( 'NONE',  ( 928.0249999999991815, 154.9999999999998863, 360.0000000000000000 ) ) ;
#33880 = CARTESIAN_POINT ( 'NONE',  ( 744.6391490659812007, -110.7363362996985501, -338.7502325331110455 ) ) ;
#33881 = DIRECTION ( 'NONE',  ( -1.000000000000000000, 0.000000000000000000, 0.000000000000000000 ) ) ;
#33882 = CARTESIAN_POINT ( 'NONE',  ( 769.9999999999992042, 240.0000000000000568, -319.9999999999999432 ) ) ;
#33883 = CARTESIAN_POINT ( 'NONE',  ( 801.5560724626406000, -336.5545181178796952, 326.7756240680316182 ) ) ;
#33884 = CARTESIAN_POINT ( 'NONE',  ( 788.8264449731200330, -189.1800572038744122, 363.6646147819171233 ) ) ;
#33885 = VERTEX_POINT ( 'NONE', #18141 ) ;
#33886 = CARTESIAN_POINT ( 'NONE',  ( 762.1177392798416577, -306.5545181178797520, 309.8865473780659272 ) ) ;
#33887 = CARTESIAN_POINT ( 'NONE',  ( 777.4774526936600978, -178.2709662947835909, -304.7301800767028226 ) ) ;
#33888 = CYLINDRICAL_SURFACE ( 'NONE', #28251, 9.999999999999982236 ) ;
#33889 = CARTESIAN_POINT ( 'NONE',  ( 812.3518521366052028, -121.0999726633348956, 326.5853460496235243 ) ) ;
#33890 = CARTESIAN_POINT ( 'NONE',  ( 813.1304606946830518, -305.9073299311467622, -352.3570229623690580 ) ) ;
#33891 = CARTESIAN_POINT ( 'NONE',  ( 814.9108240113580450, -448.2709662947827951, -337.5031285880265273 ) ) ;
#33892 = CARTESIAN_POINT ( 'NONE',  ( 804.9363028652555840, -160.2709662947836762, 338.2165204200192079 ) ) ;
#33893 = EDGE_LOOP ( 'NONE', ( #27448, #31027, #31699, #37155 ) ) ;
#33894 = CARTESIAN_POINT ( 'NONE',  ( 786.2694204179717872, -405.2817908451522158, 305.1769319972829067 ) ) ;
#33895 = CARTESIAN_POINT ( 'NONE',  ( 808.7758568127978833, -340.1692326535047641, -320.0363995740631822 ) ) ;
#33896 = CARTESIAN_POINT ( 'NONE',  ( 751.9810565676468741, -98.08914811296568814, -360.9747183278973921 ) ) ;
#33897 = CARTESIAN_POINT ( 'NONE',  ( 769.0155153010367712, -58.37269993606236085, 362.7791456095907279 ) ) ;
#33898 = CARTESIAN_POINT ( 'NONE',  ( 777.5031285880264704, -382.8164208402374697, -374.9108240113588408 ) ) ;
#33899 = PLANE ( 'NONE',  #41674 ) ;
#33900 = CARTESIAN_POINT ( 'NONE',  ( 764.0069404352550464, -423.0783235625953580, 359.2566176426627180 ) ) ;
#33901 = ORIENTED_EDGE ( 'NONE', *, *, #7216, .F. ) ;
#33902 = CARTESIAN_POINT ( 'NONE',  ( 804.9511171171677688, -77.80559628986920018, 335.8780910478229202 ) ) ;
#33903 = CARTESIAN_POINT ( 'NONE',  ( 813.9316612368132837, -103.4419599262327836, -348.6739635108323228 ) ) ;
#33904 = DIRECTION ( 'NONE',  ( 1.880165489482579047E-16, 1.000000000000000000, 0.000000000000000000 ) ) ;
#33905 = CARTESIAN_POINT ( 'NONE',  ( 810.1134526219336749, -272.5328690171413086, 357.8822607201570349 ) ) ;
#33906 = CARTESIAN_POINT ( 'NONE',  ( 804.9363028652555840, -88.27096629478390355, 338.2165204200192079 ) ) ;
#33907 = ORIENTED_EDGE ( 'NONE', *, *, #2999, .F. ) ;
#33908 = CARTESIAN_POINT ( 'NONE',  ( 802.7791456095903868, -4.714687198960358039, -329.0155153010375102 ) ) ;
#33909 = CARTESIAN_POINT ( 'NONE',  ( 788.8264449731200330, -261.1800572038741848, 363.6646147819171233 ) ) ;
#33910 = CARTESIAN_POINT ( 'NONE',  ( 793.4146539503750546, -433.9874144716862361, -307.6481478633938877 ) ) ;
#33911 = CARTESIAN_POINT ( 'NONE',  ( 939.9999999999992042, 50.81038600091411439, 209.9999999999999716 ) ) ;
#33912 = ORIENTED_EDGE ( 'NONE', *, *, #32345, .T. ) ;
#33913 = ORIENTED_EDGE ( 'NONE', *, *, #9206, .F. ) ;
#33914 = CARTESIAN_POINT ( 'NONE',  ( 815.3608509340175488, -386.7363362996977116, -341.2497674668889545 ) ) ;
#33915 = CARTESIAN_POINT ( 'NONE',  ( 788.8264449731200330, -237.1800572038742985, -363.6646147819171233 ) ) ;
#33916 = EDGE_CURVE ( 'NONE', #36028, #22786, #43321, .T. ) ;
#33918 = CARTESIAN_POINT ( 'NONE',  ( 747.3154664389472828, -211.9874144716869750, 326.4474001241230781 ) ) ;
#33917 = CARTESIAN_POINT ( 'NONE',  ( 814.5518280994195948, -327.7255117493285752, 332.4837098697145166 ) ) ;
#33919 = CARTESIAN_POINT ( 'NONE',  ( 763.8424801807145741, -210.0090635724255321, -320.5453621957614700 ) ) ;
#33920 = CARTESIAN_POINT ( 'NONE',  ( 797.6776695296629214, -211.5436935675107861, -357.6776695296636603 ) ) ;
#33921 = CARTESIAN_POINT ( 'NONE',  ( 788.8264449731201466, -429.1800572038737300, -363.6646147819170665 ) ) ;
#33922 = ORIENTED_EDGE ( 'NONE', *, *, #1789, .T. ) ;
#33923 = CARTESIAN_POINT ( 'NONE',  ( 755.3201227861273992, -219.7255117493289447, 345.3687786644892981 ) ) ;
#33924 = CARTESIAN_POINT ( 'NONE',  ( 764.8639956371174549, -104.0891481129656881, -319.7806653035542013 ) ) ;
#33925 = ORIENTED_EDGE ( 'NONE', *, *, #23560, .T. ) ;
#33926 = CARTESIAN_POINT ( 'NONE',  ( 792.3570229623688874, -357.1800572038739006, 373.1304606946836202 ) ) ;
#33927 = CARTESIAN_POINT ( 'NONE',  ( 959.5497976682736407, 229.9999999999998579, 339.9999999999998863 ) ) ;
#33928 = CARTESIAN_POINT ( 'NONE',  ( 769.9999999999992042, 240.0000000000000853, -360.0000000000000000 ) ) ;
#33929 = CARTESIAN_POINT ( 'NONE',  ( 959.5497976682736407, 229.9999999999998579, 339.9999999999998863 ) ) ;
#33930 = CARTESIAN_POINT ( 'NONE',  ( 799.2566176426618085, -216.0090635724255037, 324.0069404352559559 ) ) ;
#33931 = CARTESIAN_POINT ( 'NONE',  ( 771.2633955100217236, -71.90732993114760063, 363.4237431249939618 ) ) ;
#33932 = ORIENTED_EDGE ( 'NONE', *, *, #37641, .T. ) ;
#33933 = CARTESIAN_POINT ( 'NONE',  ( 778.7629533639073998, -440.7363362996975980, -375.0009284576466371 ) ) ;
#33934 = CARTESIAN_POINT ( 'NONE',  ( 749.2812353651451076, -30.45278447660226817, -323.2262854647983090 ) ) ;
#33935 = CARTESIAN_POINT ( 'NONE',  ( 796.7845633553578182, -273.6237781080504305, 358.5707757039688204 ) ) ;
#33936 = CARTESIAN_POINT ( 'NONE',  ( 758.0580252608178853, -438.4527844766009821, -328.0187753319985404 ) ) ;
#33937 = CARTESIAN_POINT ( 'NONE',  ( 756.3353852180820240, -53.90732993114765037, -331.1735550268787733 ) ) ;
#33938 = CARTESIAN_POINT ( 'NONE',  ( 763.2262854647970016, -440.6346026584191122, 309.2812353651462445 ) ) ;
#33939 = DIRECTION ( 'NONE',  ( -1.000000000000000000, -0.000000000000000000, -0.000000000000000000 ) ) ;
#33940 = CARTESIAN_POINT ( 'NONE',  ( 769.0155153010367712, -298.3726999360616787, -362.7791456095907279 ) ) ;
#33941 = CARTESIAN_POINT ( 'NONE',  ( 763.2262854647970016, -176.6346026584199933, -309.2812353651462445 ) ) ;
#33942 = CARTESIAN_POINT ( 'NONE',  ( 796.7737145352015204, -68.63460265842033436, 370.7187646348536987 ) ) ;
#33943 = ADVANCED_FACE ( 'NONE', ( #14902 ), #35910, .F. ) ;
#33944 = CARTESIAN_POINT ( 'NONE',  ( 754.9967657858570647, -145.5436935675109851, 365.0032342141425374 ) ) ;
#33945 = CARTESIAN_POINT ( 'NONE',  ( -858.8365100919713768, 240.0000000000002274, -197.2499999999882903 ) ) ;
#33946 = SURFACE_STYLE_USAGE ( .BOTH. , #33730 ) ;
#33947 = CARTESIAN_POINT ( 'NONE',  ( 808.7758568127978833, -220.1692326535051052, -320.0363995740631822 ) ) ;
#33948 = CARTESIAN_POINT ( 'NONE',  ( 813.5763878283155464, -411.8272453906067199, 351.1614460488615350 ) ) ;
#33949 = DIRECTION ( 'NONE',  ( -1.000000000000000000, -0.000000000000000000, -0.000000000000000000 ) ) ;
#33950 = CARTESIAN_POINT ( 'NONE',  ( 748.9653473494363425, -410.6346026584191122, 356.9462024416521331 ) ) ;
#33951 = CARTESIAN_POINT ( 'NONE',  ( 747.2067596250078623, -27.18005720387500901, 352.2312462859687230 ) ) ;
#33952 = CARTESIAN_POINT ( 'NONE',  ( 788.8264449731200330, -357.1800572038739006, -363.6646147819171233 ) ) ;
#33953 = CARTESIAN_POINT ( 'NONE',  ( 772.3691319403857278, -23.26014174441484883, 315.8894580844506663 ) ) ;
#33954 = CARTESIAN_POINT ( 'NONE',  ( 747.6481478633932056, -85.09997266333499510, -353.4146539503763620 ) ) ;
#33955 = CARTESIAN_POINT ( 'NONE',  ( 796.7845633553578182, -153.6237781080508000, -358.5707757039688204 ) ) ;
#33956 = CARTESIAN_POINT ( 'NONE',  ( 795.6651683502461765, -154.7146871989598935, 371.3240766477733814 ) ) ;
#33957 = VERTEX_POINT ( 'NONE', #43511 ) ;
#33958 = CARTESIAN_POINT ( 'NONE',  ( 765.0180583372156207, -48.99823902205675807, -360.0135310231089534 ) ) ;
#33959 = CARTESIAN_POINT ( 'NONE',  ( 757.2208543904082489, -160.7146871989598651, -350.9844846989624330 ) ) ;
#33960 = CARTESIAN_POINT ( 'NONE',  ( 788.7366044899766848, -179.9073299311472454, 316.5762568750059813 ) ) ;
#33961 = EDGE_CURVE ( 'NONE', #40052, #3816, #34477, .T. ) ;
#33962 = PRODUCT_DEFINITION_SHAPE ( 'NONE', 'NONE',  #45727 ) ;
#33963 = CARTESIAN_POINT ( 'NONE',  ( 746.0683387631852383, 4.558040073766884248, -331.3260364891676204 ) ) ;
#33964 = CARTESIAN_POINT ( 'NONE',  ( 805.1927285166399315, -304.8164208402376971, 341.8018195045277707 ) ) ;
#33965 = FACE_OUTER_BOUND ( 'NONE', #35505, .T. ) ;
#33966 = ORIENTED_EDGE ( 'NONE', *, *, #2367, .F. ) ;
#33967 = CARTESIAN_POINT ( 'NONE',  ( 780.5290396650775619, -12.35105083532396897, 365.2837595273619513 ) ) ;
#33968 = CARTESIAN_POINT ( 'NONE',  ( 745.7194118038753459, -277.6454272087889308, -348.7631598425976449 ) ) ;
#33969 = ORIENTED_EDGE ( 'NONE', *, *, #14520, .F. ) ;
#33970 = DIRECTION ( 'NONE',  ( 0.000000000000000000, 0.000000000000000000, 1.000000000000000000 ) ) ;
#33971 = ADVANCED_FACE ( 'NONE', ( #18374 ), #22261, .F. ) ;
#33972 = CARTESIAN_POINT ( 'NONE',  ( 796.7737145352015204, -236.6346026584198228, 370.7187646348536987 ) ) ;
#33973 = CARTESIAN_POINT ( 'NONE',  ( 798.5707757039680246, -317.4636090269706301, 356.7845633553585003 ) ) ;
#33974 = CARTESIAN_POINT ( 'NONE',  ( 775.9200461376533440, -383.8055962898682765, 315.3028492785443291 ) ) ;
#33975 = ORIENTED_EDGE ( 'NONE', *, *, #18712, .F. ) ;
#33976 = CARTESIAN_POINT ( 'NONE',  ( 754.7162404726377645, -110.7363362996985501, -339.4709603349214717 ) ) ;
#33977 = CARTESIAN_POINT ( 'NONE',  ( 758.0580252608178853, -126.4527844766019626, -328.0187753319985404 ) ) ;
#33978 = CARTESIAN_POINT ( 'NONE',  ( 781.8018195045267476, -310.2709662947832499, -365.1927285166407273 ) ) ;
#33979 = ORIENTED_EDGE ( 'NONE', *, *, #13335, .F. ) ;
#33980 = CARTESIAN_POINT ( 'NONE',  ( 756.3353852180819104, -437.9073299311463074, -331.1735550268788302 ) ) ;
#33981 = CARTESIAN_POINT ( 'NONE',  ( 770.0799878456142551, -301.9874144716867477, 362.9823548866085616 ) ) ;
#33982 = DIRECTION ( 'NONE',  ( -1.000000000000000000, -0.000000000000000000, 0.000000000000000000 ) ) ;
#33983 = CARTESIAN_POINT ( 'NONE',  ( -338.8365100919713200, 260.0000000000001137, -197.2499999999919282 ) ) ;
#33984 = CARTESIAN_POINT ( 'NONE',  ( 778.1981804954714335, 13.72903370521577138, 314.8072714833589885 ) ) ;
#33985 = ORIENTED_EDGE ( 'NONE', *, *, #38013, .F. ) ;
#33986 = CARTESIAN_POINT ( 'NONE',  ( 762.1177392798416577, -330.5545181178796952, -309.8865473780659272 ) ) ;
#33987 = EDGE_CURVE ( 'NONE', #22437, #2273, #21961, .T. ) ;
#33988 = CARTESIAN_POINT ( 'NONE',  ( 795.1360043628807261, -308.0891481129650629, -360.2193346964456282 ) ) ;
#33989 = EDGE_CURVE ( 'NONE', #17477, #791, #18995, .T. ) ;
#33990 = CARTESIAN_POINT ( 'NONE',  ( 311.1634899080286232, 229.9999999999999716, -199.9999999999963336 ) ) ;
#33991 = CARTESIAN_POINT ( 'NONE',  ( 769.0155153010367712, -202.3726999360618777, -362.7791456095907279 ) ) ;
#33992 = CARTESIAN_POINT ( 'NONE',  ( 812.7932403749906598, -39.18005720387496638, 327.7687537140311633 ) ) ;
#33993 = CARTESIAN_POINT ( 'NONE',  ( 51.16348990802859475, 240.0000000000000568, -199.9999999999945146 ) ) ;
#33994 = CARTESIAN_POINT ( 'NONE',  ( 782.4968714119720516, -370.8164208402375834, -305.0891759886411023 ) ) ;
#33995 = DIRECTION ( 'NONE',  ( 0.000000000000000000, -1.000000000000000000, 0.000000000000000000 ) ) ;
#33996 = CARTESIAN_POINT ( 'NONE',  ( 766.4474001241216001, -331.0999726633342561, 307.3154664389482491 ) ) ;
#33997 = CARTESIAN_POINT ( 'NONE',  ( 927.9999999999990905, 219.9999999999998863, -360.0000000000000000 ) ) ;
#33998 = CARTESIAN_POINT ( 'NONE',  ( 805.0032342141412300, -301.5436935675105588, 314.9967657858571783 ) ) ;
#33999 = CARTESIAN_POINT ( 'NONE',  ( 792.2312462859673587, -35.90732993114770011, -307.2067596250082602 ) ) ;
#34000 = CARTESIAN_POINT ( 'NONE',  ( 803.6646147819161570, -257.9073299311469896, -348.8264449731210561 ) ) ;
#34001 = CARTESIAN_POINT ( 'NONE',  ( -200.7583438952259485, 394.6698570112193920, -274.9999999999999432 ) ) ;
#34002 = CARTESIAN_POINT ( 'NONE',  ( 805.1927285166397041, -376.8164208402375834, 341.8018195045277707 ) ) ;
#34003 = CARTESIAN_POINT ( 'NONE',  ( 802.5472867521000353, -124.3726999360621619, 350.8726784830461156 ) ) ;
#34004 = CARTESIAN_POINT ( 'NONE',  ( 756.1348686366196716, -41.26014174441479554, -347.5531968255698416 ) ) ;
#34005 = CARTESIAN_POINT ( 'NONE',  ( 749.8865473780648472, -44.53286901714205470, 322.1177392798429082 ) ) ;
#34006 = CARTESIAN_POINT ( 'NONE',  ( 804.4286716492782716, -353.3618753856922012, 345.3141322388244703 ) ) ;
#34007 = CARTESIAN_POINT ( 'NONE',  ( 812.7932403749906598, 8.819942796124882634, 327.7687537140311633 ) ) ;
#34008 = EDGE_CURVE ( 'NONE', #24267, #14504, #11613, .T. ) ;
#34009 = CARTESIAN_POINT ( 'NONE',  ( 989.9999999999992042, 240.0000000000001990, -201.9999999999999716 ) ) ;
#34010 = CARTESIAN_POINT ( 'NONE',  ( 778.1981804954714335, -418.2709662947827383, 314.8072714833589885 ) ) ;
#34011 = VERTEX_POINT ( 'NONE', #802 ) ;
#34012 = EDGE_CURVE ( 'NONE', #33397, #3427, #4974, .T. ) ;
#34013 = CARTESIAN_POINT ( 'NONE',  ( 756.7813123517142913, -379.9874144716865203, -329.9779781133712504 ) ) ;
#34015 = CARTESIAN_POINT ( 'NONE',  ( 771.1735550268780344, -177.1800572038744974, 316.3353852180828198 ) ) ;
#34014 = CARTESIAN_POINT ( 'NONE',  ( 781.7834795799800531, -178.8164208402381519, 315.0636971347436202 ) ) ;
#34016 = CARTESIAN_POINT ( 'NONE',  ( 751.2241431872005251, -376.1692326535046504, -359.9636004259367610 ) ) ;
#34017 = CARTESIAN_POINT ( 'NONE',  ( 759.9999999999992042, -462.9681489794448339, 309.9999999999998863 ) ) ;
#34018 = ORIENTED_EDGE ( 'NONE', *, *, #15390, .F. ) ;
#34019 = CARTESIAN_POINT ( 'NONE',  ( 794.9819416627830151, -396.9982390220556567, 319.9864689768909898 ) ) ;
#34020 = ORIENTED_EDGE ( 'NONE', *, *, #39704, .T. ) ;
#34021 = ADVANCED_FACE ( 'NONE', ( #22048, #11663, #25739 ), #31973, .F. ) ;
#34022 = CARTESIAN_POINT ( 'NONE',  ( 808.3070685750230950, -210.9982390220561967, -361.1904061080339261 ) ) ;
#34023 = CARTESIAN_POINT ( 'NONE',  ( 811.0346526505617248, -134.6346026584201070, 323.0537975583478101 ) ) ;
#34024 = VERTEX_POINT ( 'NONE', #344 ) ;
#34025 = CARTESIAN_POINT ( 'NONE',  ( 765.0180583372156207, -216.9982390220562252, -360.0135310231089534 ) ) ;
#34026 = ORIENTED_EDGE ( 'NONE', *, *, #43817, .T. ) ;
#34027 = CARTESIAN_POINT ( 'NONE',  ( 754.8072714833581358, -340.8164208402376971, -338.1981804954720587 ) ) ;
#34028 = CARTESIAN_POINT ( 'NONE',  ( 776.9254006560222479, -452.1908817542428665, -314.8983024940802125 ) ) ;
#34029 = CARTESIAN_POINT ( 'NONE',  ( 777.5031285880264704, -262.8164208402379245, 374.9108240113588408 ) ) ;
#34030 = CARTESIAN_POINT ( 'NONE',  ( 803.8651313633788504, -197.2601417444143124, 332.4468031744301015 ) ) ;
#34032 = LINE ( 'NONE', #20850, #10044 ) ;
#34031 = DIRECTION ( 'NONE',  ( 0.000000000000000000, 0.000000000000000000, 1.000000000000000000 ) ) ;
#34033 = PLANE ( 'NONE',  #16171 ) ;
#34034 = ORIENTED_EDGE ( 'NONE', *, *, #29262, .T. ) ;
#34035 = CARTESIAN_POINT ( 'NONE',  ( 803.4237431249931660, 8.819942796124882634, -331.2633955100225194 ) ) ;
#34036 = DIRECTION ( 'NONE',  ( -0.000000000000000000, -0.000000000000000000, -1.000000000000000000 ) ) ;
#34037 = DIRECTION ( 'NONE',  ( 0.000000000000000000, 0.000000000000000000, 1.000000000000000000 ) ) ;
#34038 = ORIENTED_EDGE ( 'NONE', *, *, #5773, .T. ) ;
#34039 = CARTESIAN_POINT ( 'NONE',  ( 750.9282345327678740, -232.9181544815163249, -319.8311093483690115 ) ) ;
#34040 = MECHANICAL_DESIGN_GEOMETRIC_PRESENTATION_REPRESENTATION (  '', ( #25201 ), #884 ) ;
#34041 = CARTESIAN_POINT ( 'NONE',  ( 795.8262568251477660, -118.3726999360621619, 308.3538107759623585 ) ) ;
#34043 = CARTESIAN_POINT ( 'NONE',  ( 788.7366044899766848, -179.9073299311472454, -316.5762568750059813 ) ) ;
#34042 = FACE_OUTER_BOUND ( 'NONE', #5504, .T. ) ;
#34044 = CARTESIAN_POINT ( 'NONE',  ( 798.7617431975189675, -363.6237781080502032, -323.0428371773161871 ) ) ;
#34045 = CARTESIAN_POINT ( 'NONE',  ( 746.4236121716829757, -231.8272453906072315, -328.8385539511384650 ) ) ;
#34046 = DIRECTION ( 'NONE',  ( 0.000000000000000000, 1.000000000000000000, 0.000000000000000000 ) ) ;
#34047 = CYLINDRICAL_SURFACE ( 'NONE', #37089, 1.000000000000000888 ) ;
#34048 = CARTESIAN_POINT ( 'NONE',  ( 757.4527132478984868, -88.37269993606226137, -329.1273215169538844 ) ) ;
#34049 = CARTESIAN_POINT ( 'NONE',  ( 796.9571628226829034, -431.4636090269702322, 321.2382568024804641 ) ) ;
#34050 = CARTESIAN_POINT ( 'NONE',  ( 787.4999999999992042, -462.9681489794447202, -270.0000000000000568 ) ) ;
#34051 = CARTESIAN_POINT ( 'NONE',  ( 794.1144889064781864, -418.1692326535044799, -360.9840315886528401 ) ) ;
#34052 = CARTESIAN_POINT ( 'NONE',  ( 763.0537975583476964, -264.4527844766016074, -371.0346526505628617 ) ) ;
#34053 = CARTESIAN_POINT ( 'NONE',  ( 1007.605605532488426, 35.55895481007120651, 914.5706932916501728 ) ) ;
#34054 = LINE ( 'NONE', #9121, #43778 ) ;
#34055 = CARTESIAN_POINT ( 'NONE',  ( 759.9864689768902508, -50.08914811296584446, -354.9819416627836404 ) ) ;
#34056 = CARTESIAN_POINT ( 'NONE',  ( 750.9282345327678740, -208.9181544815164102, 319.8311093483690115 ) ) ;
#34057 = CARTESIAN_POINT ( 'NONE',  ( 786.2056067578752163, -155.8055962898689586, -374.4686193811670023 ) ) ;
#34058 = CARTESIAN_POINT ( 'NONE',  ( 811.0346526505616112, -182.6346026584199649, 323.0537975583477532 ) ) ;
#34059 = CARTESIAN_POINT ( 'NONE',  ( 782.5225473063381969, -406.2709662947829088, -375.2698199232970637 ) ) ;
#34060 = CARTESIAN_POINT ( 'NONE',  ( 911.9999999999992042, 219.9999999999998863, -359.9749999999999659 ) ) ;
#34061 = CARTESIAN_POINT ( 'NONE',  ( 754.8072714833581358, -268.8164208402378108, 338.1981804954720587 ) ) ;
#34062 = CARTESIAN_POINT ( 'NONE',  ( 755.5913626894240451, -61.64542720878961291, 346.6156483768012890 ) ) ;
#34063 = CARTESIAN_POINT ( 'NONE',  ( 771.1735550268778070, -417.1800572038736163, -316.3353852180827630 ) ) ;
#34064 = DIRECTION ( 'NONE',  ( 1.000000000000000000, 0.000000000000000000, 0.000000000000000000 ) ) ;
#34065 = EDGE_CURVE ( 'NONE', #41099, #21104, #4717, .T. ) ;
#34066 = CARTESIAN_POINT ( 'NONE',  ( 927.9999999999993179, 154.9999999999998863, -359.9749999999999659 ) ) ;
#34067 = CARTESIAN_POINT ( 'NONE',  ( 802.7791456095903868, -76.71468719896012090, 329.0155153010375102 ) ) ;
#34068 = ORIENTED_EDGE ( 'NONE', *, *, #4642, .T. ) ;
#34069 = CARTESIAN_POINT ( 'NONE',  ( 769.1273215169530886, -238.7146871989596661, -317.4527132478988847 ) ) ;
#34070 = CARTESIAN_POINT ( 'NONE',  ( 797.6776695296629214, -67.54369356751125508, 357.6776695296636603 ) ) ;
#34071 = AXIS2_PLACEMENT_3D ( 'NONE', #611, #22515, #29013 ) ;
#34072 = CARTESIAN_POINT ( 'NONE',  ( 795.6651683502461765, -250.7146871989595809, -371.3240766477733814 ) ) ;
#34073 = FILL_AREA_STYLE ('',( #12392 ) ) ;
#34074 = CARTESIAN_POINT ( 'NONE',  ( 815.0009284576459549, -366.3510508353228374, 338.7629533639073429 ) ) ;
#34075 = ORIENTED_EDGE ( 'NONE', *, *, #7988, .F. ) ;
#34076 = CARTESIAN_POINT ( 'NONE',  ( 778.2165204200184689, -166.8164208402382087, -364.9363028652563230 ) ) ;
#34077 = CARTESIAN_POINT ( 'NONE',  ( 754.8072714833581358, -388.8164208402374129, 338.1981804954720587 ) ) ;
#34078 = CARTESIAN_POINT ( 'NONE',  ( 745.0891759886404770, -124.2709662947837899, -342.4968714119734159 ) ) ;
#34079 = CARTESIAN_POINT ( 'NONE',  ( 804.4286716492782716, -65.36187538569306810, -345.3141322388244703 ) ) ;
#34080 = ORIENTED_EDGE ( 'NONE', *, *, #33474, .F. ) ;
#34081 = CARTESIAN_POINT ( 'NONE',  ( 790.9844846989617508, -46.37269993606239638, -317.2208543904092721 ) ) ;
#34082 = CARTESIAN_POINT ( 'NONE',  ( 763.0428371773158460, -371.4636090269705164, -358.7617431975195359 ) ) ;
#34084 = CARTESIAN_POINT ( 'NONE',  ( 772.4468031744293057, -417.8272453906067199, 363.8651313633793620 ) ) ;
#34083 = CARTESIAN_POINT ( 'NONE',  ( 797.6776695296629214, -91.54369356751116982, 357.6776695296636603 ) ) ;
#34087 = CARTESIAN_POINT ( 'NONE',  ( 800.1688906516307043, -346.1692326535047641, 369.0717654672308186 ) ) ;
#34086 = CARTESIAN_POINT ( 'NONE',  ( 799.9999999999993179, -512.9681489794448908, 350.0000000000000000 ) ) ;
#34085 = CARTESIAN_POINT ( 'NONE',  ( 747.2067596250078623, -435.1800572038737869, 352.2312462859687230 ) ) ;
#34088 = CARTESIAN_POINT ( 'NONE',  ( 787.5531968255692163, -333.8272453906070041, -316.1348686366205811 ) ) ;
#34089 = CARTESIAN_POINT ( 'NONE',  ( 797.6776695296629214, -331.5436935675104451, -357.6776695296636603 ) ) ;
#34090 = AXIS2_PLACEMENT_3D ( 'NONE', #42696, #664, #17766 ) ;
#34091 = CARTESIAN_POINT ( 'NONE',  ( 815.3608509340175488, -146.7363362996984506, -341.2497674668889545 ) ) ;
#34092 = CARTESIAN_POINT ( 'NONE',  ( 795.1271208383656131, -452.8379544210779954, 371.6178728169206238 ) ) ;
#34094 = DIRECTION ( 'NONE',  ( 1.258530456726092671E-16, -0.7651688349527167032, 0.6438296778008156807 ) ) ;
#34093 = CARTESIAN_POINT ( 'NONE',  ( 791.0733055594794223, 17.05262341476191068, 312.1184307474205184 ) ) ;
#34095 = CARTESIAN_POINT ( 'NONE',  ( 760.0363995740630116, -106.9181544815167371, -368.7758568127991907 ) ) ;
#34096 = CARTESIAN_POINT ( 'NONE',  ( -949.5497976682736407, 230.0000000000002274, 339.9999999999999432 ) ) ;
#34097 = DIRECTION ( 'NONE',  ( 0.000000000000000000, 0.000000000000000000, 1.000000000000000000 ) ) ;
#34098 = CARTESIAN_POINT ( 'NONE',  ( 802.5472867521000353, -316.3726999360615082, 350.8726784830461156 ) ) ;
#34099 = CARTESIAN_POINT ( 'NONE',  ( 771.2633955100217236, -191.9073299311471885, 363.4237431249939618 ) ) ;
#34100 = VERTEX_POINT ( 'NONE', #14447 ) ;
#34101 = CARTESIAN_POINT ( 'NONE',  ( 750.9282345327678740, -304.9181544815161828, 319.8311093483690115 ) ) ;
#34102 = CARTESIAN_POINT ( 'NONE',  ( 747.2067596250078623, -171.1800572038745543, -352.2312462859687230 ) ) ;
#34103 = DIRECTION ( 'NONE',  ( -0.000000000000000000, -0.000000000000000000, 1.000000000000000000 ) ) ;
#34104 = CARTESIAN_POINT ( 'NONE',  ( 771.3260364891663130, -115.6454272087894424, 306.0683387631859773 ) ) ;
#34105 = CARTESIAN_POINT ( 'NONE',  ( 792.3570229623688874, -309.1800572038740711, -373.1304606946836202 ) ) ;
#34106 = DIRECTION ( 'NONE',  ( 1.000000000000000000, 0.000000000000000000, 0.000000000000000000 ) ) ;
#34107 = DIRECTION ( 'NONE',  ( 0.000000000000000000, 0.9238795325112891810, -0.3826834323650838421 ) ) ;
#34108 = CARTESIAN_POINT ( 'NONE',  ( 756.5762568750052424, -147.1800572038746395, 348.7366044899774238 ) ) ;
#34109 = ORIENTED_EDGE ( 'NONE', *, *, #27246, .T. ) ;
#34110 = CARTESIAN_POINT ( 'NONE',  ( 766.4474001241216001, -427.0999726633338582, 307.3154664389482491 ) ) ;
#34111 = CARTESIAN_POINT ( 'NONE',  ( 808.7758568127978833, -364.1692326535046504, -320.0363995740631822 ) ) ;
#34112 = CARTESIAN_POINT ( 'NONE',  ( 814.2001403089898304, -137.3618753856928265, -347.4397851343538264 ) ) ;
#34113 = CARTESIAN_POINT ( 'NONE',  ( 775.8780910478218402, -57.28179084515326736, 364.9511171171680530 ) ) ;
#34114 = CARTESIAN_POINT ( 'NONE',  ( 800.9747183278959710, -396.9982390220556567, -311.9810565676471583 ) ) ;
#34115 = DIRECTION ( 'NONE',  ( 1.000000000000000000, 0.000000000000000000, 0.000000000000000000 ) ) ;
#34116 = CARTESIAN_POINT ( 'NONE',  ( 759.2295555964440155, -424.1692326535044799, 353.9708237608231229 ) ) ;
#34117 = VERTEX_POINT ( 'NONE', #42622 ) ;
#34118 = CIRCLE ( 'NONE', #20866, 10.00000000000000888 ) ;
#34119 = CARTESIAN_POINT ( 'NONE',  ( 759.8311093483677041, -166.1692326535053041, -310.9282345327691814 ) ) ;
#34120 = CARTESIAN_POINT ( 'NONE',  ( 784.9999999999992042, 205.0000000000000568, -255.0000000000000000 ) ) ;
#34121 = CARTESIAN_POINT ( 'NONE',  ( 798.0661480581538854, -290.5328690171412518, 309.5768839229118043 ) ) ;
#34122 = CARTESIAN_POINT ( 'NONE',  ( 801.9419747391806368, -90.45278447660209054, 351.9812246680014027 ) ) ;
#34123 = ORIENTED_EDGE ( 'NONE', *, *, #42732, .T. ) ;
#34124 = CARTESIAN_POINT ( 'NONE',  ( 775.9200461376533440, 0.1944037101305369775, -315.3028492785443291 ) ) ;
#34125 = CARTESIAN_POINT ( 'NONE',  ( 755.5713283507202505, -269.3618753856924286, 334.6858677611754729 ) ) ;
#34126 = CARTESIAN_POINT ( 'NONE',  ( 801.1904061080336987, 3.910851887033985896, -368.3070685750235498 ) ) ;
#34127 = CARTESIAN_POINT ( 'NONE',  ( 799.9999999999993179, 166.4563064324884465, -360.0000000000000000 ) ) ;
#34128 = ORIENTED_EDGE ( 'NONE', *, *, #25747, .F. ) ;
#34129 = ORIENTED_EDGE ( 'NONE', *, *, #24044, .F. ) ;
#34130 = CARTESIAN_POINT ( 'NONE',  ( 764.1737431748507561, -418.3726999360612808, -371.6461892240376415 ) ) ;
#34132 = CARTESIAN_POINT ( 'NONE',  ( 773.7943932421234194, -263.8055962898686175, 305.5313806188329409 ) ) ;
#34131 = CARTESIAN_POINT ( 'NONE',  ( 801.1904061080338124, -332.0891481129649492, 368.3070685750236066 ) ) ;
#34133 = CARTESIAN_POINT ( 'NONE',  ( 755.5913626894240451, -229.6454272087890729, -346.6156483768012890 ) ) ;
#34134 = CARTESIAN_POINT ( 'NONE',  ( 771.2633955100217236, -215.9073299311471317, -363.4237431249939618 ) ) ;
#34135 = CARTESIAN_POINT ( 'NONE',  ( 762.1405469898973024, -433.5436935675100472, -357.8594530101016176 ) ) ;
#34136 = CARTESIAN_POINT ( 'NONE',  ( 778.2165204200184689, -214.8164208402380666, 364.9363028652563230 ) ) ;
#34137 = EDGE_LOOP ( 'NONE', ( #26187, #874, #27906, #36600 ) ) ;
#34138 = CARTESIAN_POINT ( 'NONE',  ( 814.2001403089898304, -353.3618753856922012, 347.4397851343538264 ) ) ;
#34139 = CARTESIAN_POINT ( 'NONE',  ( 959.5497976682736407, 239.9999999999998863, -209.9999999999999716 ) ) ;
#34140 = CARTESIAN_POINT ( 'NONE',  ( 772.1467562141141343, 16.45630643248850689, 315.9110025235851253 ) ) ;
#34141 = FACE_BOUND ( 'NONE', #39350, .T. ) ;
#34142 = CARTESIAN_POINT ( 'NONE',  ( 802.9823548866075953, -217.0999726633345972, 330.0799878456151077 ) ) ;
#34143 = CARTESIAN_POINT ( 'NONE',  ( 755.0636971347428243, -100.2709662947838609, 341.7834795799807353 ) ) ;
#34144 = ORIENTED_EDGE ( 'NONE', *, *, #2947, .F. ) ;
#34145 = CARTESIAN_POINT ( 'NONE',  ( 812.3518521366052028, -433.0999726633339151, -326.5853460496235243 ) ) ;
#34146 = CIRCLE ( 'NONE', #6136, 10.00000000000000888 ) ;
#34147 = CARTESIAN_POINT ( 'NONE',  ( 796.9462024416508257, -60.45278447660216159, -308.9653473494370246 ) ) ;
#34148 = CARTESIAN_POINT ( 'NONE',  ( 793.2243759319678702, -242.5328690171414507, 318.4439275373583200 ) ) ;
#34149 = CARTESIAN_POINT ( 'NONE',  ( 762.1405469898971887, -433.5436935675099903, -357.8594530101015607 ) ) ;
#34150 = CARTESIAN_POINT ( 'NONE',  ( 785.3687786644885591, -35.36187538569316047, -315.3201227861280813 ) ) ;
#34151 = CARTESIAN_POINT ( 'NONE',  ( 757.7880784355613741, -18.00906357242611477, 312.4576283171834916 ) ) ;
#34152 = DIRECTION ( 'NONE',  ( 0.000000000000000000, 0.000000000000000000, 1.000000000000000000 ) ) ;
#34153 = CARTESIAN_POINT ( 'NONE',  ( 779.4763451958990572, -296.7363362996979390, -365.0264073115438919 ) ) ;
#34154 = CARTESIAN_POINT ( 'NONE',  ( 814.9108240113580450, -208.2709662947835341, -337.5031285880265273 ) ) ;
#34155 = CARTESIAN_POINT ( 'NONE',  ( 754.9967657858570647, -97.54369356751112718, 365.0032342141425374 ) ) ;
#34156 = CARTESIAN_POINT ( 'NONE',  ( 792.2312462859673587, -131.9073299311473875, 307.2067596250082602 ) ) ;
#34157 = CARTESIAN_POINT ( 'NONE',  ( 939.9999999999993179, -600.0000000000001137, 350.0000000000000000 ) ) ;
#34158 = DIRECTION ( 'NONE',  ( -1.000000000000000000, -0.000000000000000000, -0.000000000000000000 ) ) ;
#34159 = CARTESIAN_POINT ( 'NONE',  ( 766.5853460496234675, -229.9874144716869466, -372.3518521366060554 ) ) ;
#34160 = VECTOR ( 'NONE', #33856, 1000.000000000000000 ) ;
#34161 = CARTESIAN_POINT ( 'NONE',  ( 754.3581564841646241, -425.4636090269703459, 316.1443688327762516 ) ) ;
#34162 = CARTESIAN_POINT ( 'NONE',  ( 748.9653473494363425, -266.6346026584197375, -356.9462024416521331 ) ) ;
#34163 = CARTESIAN_POINT ( 'NONE',  ( -879.9999999999992042, 529.9999999999997726, -244.9999999999999716 ) ) ;
#34164 = CARTESIAN_POINT ( 'NONE',  ( 815.2698199232961542, -400.8164208402373561, 342.5225473063383106 ) ) ;
#34165 = CARTESIAN_POINT ( 'NONE',  ( 782.4968714119720516, -10.81642084023869543, 305.0891759886411023 ) ) ;
#34166 = CARTESIAN_POINT ( 'NONE',  ( 765.0180583372156207, -336.9982390220558273, -360.0135310231089534 ) ) ;
#34167 = CARTESIAN_POINT ( 'NONE',  ( 757.2208543904082489, -16.71468719896031985, 350.9844846989624330 ) ) ;
#34168 = CARTESIAN_POINT ( 'NONE',  ( 751.2241431872005251, -40.16923265350570915, -359.9636004259367610 ) ) ;
#34169 = CARTESIAN_POINT ( 'NONE',  ( 773.3843516231979720, -157.4419599262326130, -364.4086373105754433 ) ) ;
#34170 = CARTESIAN_POINT ( 'NONE',  ( 815.0009284576459549, -174.3510508353234627, 338.7629533639073429 ) ) ;
#34171 = CARTESIAN_POINT ( 'NONE',  ( 778.1981804954715471, 13.72903370521577315, 314.8072714833591021 ) ) ;
#34172 = CARTESIAN_POINT ( 'NONE',  ( 800.1688906516307043, -178.1692326535052473, 369.0717654672308186 ) ) ;
#34173 = VERTEX_POINT ( 'NONE', #10983 ) ;
#34174 = CARTESIAN_POINT ( 'NONE',  ( 797.6776695296629214, -67.54369356751125508, -357.6776695296636603 ) ) ;
#34175 = CARTESIAN_POINT ( 'NONE',  ( 763.2154366446407039, -165.6237781080507716, -321.4292242960311228 ) ) ;
#34176 = CARTESIAN_POINT ( 'NONE',  ( 756.3353852180819104, -149.9073299311473875, 331.1735550268788302 ) ) ;
#34177 = CARTESIAN_POINT ( 'NONE',  ( 749.8865473780648472, 3.467130982857797417, -322.1177392798429082 ) ) ;
#34178 = CARTESIAN_POINT ( 'NONE',  ( 800.0135310231082713, -302.0891481129650629, 325.0180583372163028 ) ) ;
#34179 = VECTOR ( 'NONE', #1294, 1000.000000000000000 ) ;
#34180 = LINE ( 'NONE', #6487, #11675 ) ;
#34181 = ORIENTED_EDGE ( 'NONE', *, *, #29510, .T. ) ;
#34182 = CARTESIAN_POINT ( 'NONE',  ( 786.6156483768007774, -25.44195992623301450, 315.5913626894246136 ) ) ;
#34183 = AXIS2_PLACEMENT_3D ( 'NONE', #25411, #485, #15029 ) ;
#34184 = CARTESIAN_POINT ( 'NONE',  ( 812.3518521366052028, -289.0999726633343698, -326.5853460496235243 ) ) ;
#34185 = ORIENTED_EDGE ( 'NONE', *, *, #23904, .T. ) ;
#34186 = CARTESIAN_POINT ( 'NONE',  ( 0.000000000000000000, 0.000000000000000000, 0.000000000000000000 ) ) ;
#34187 = CARTESIAN_POINT ( 'NONE',  ( 811.0346526505617248, -206.6346026584198796, 323.0537975583478101 ) ) ;
#34188 = CARTESIAN_POINT ( 'NONE',  ( 755.1538015810308480, -326.1908817542433781, 343.0433043558613804 ) ) ;
#34189 = CARTESIAN_POINT ( 'NONE',  ( 770.0799878456142551, -421.9874144716863498, 362.9823548866085616 ) ) ;
#34190 = EDGE_CURVE ( 'NONE', #7001, #41246, #5693, .T. ) ;
#34191 = VERTEX_POINT ( 'NONE', #34017 ) ;
#34192 = CARTESIAN_POINT ( 'NONE',  ( 802.5472867521000353, -124.3726999360621619, -350.8726784830461156 ) ) ;
#34193 = CARTESIAN_POINT ( 'NONE',  ( 794.9819416627830151, -108.9982390220565804, -319.9864689768909898 ) ) ;
#34194 = CARTESIAN_POINT ( 'NONE',  ( 785.3687786644885591, -323.3618753856922581, -315.3201227861280813 ) ) ;
#34195 = ORIENTED_EDGE ( 'NONE', *, *, #4964, .F. ) ;
#34196 = CARTESIAN_POINT ( 'NONE',  ( 758.0580252608178853, -438.4527844766009821, -328.0187753319985404 ) ) ;
#34197 = VECTOR ( 'NONE', #7265, 1000.000000000000000 ) ;
#34198 = CARTESIAN_POINT ( 'NONE',  ( 760.5453621957607311, -309.0783235625957559, 323.8424801807151425 ) ) ;
#34199 = CARTESIAN_POINT ( 'NONE',  ( 793.3938497862117174, -453.0432664090020580, 372.3358127763067955 ) ) ;
#34200 = LINE ( 'NONE', #9960, #4236 ) ;
#34201 = CARTESIAN_POINT ( 'NONE',  ( 769.9779781133707957, -115.0999726633348956, 316.7813123517150871 ) ) ;
#34202 = DIRECTION ( 'NONE',  ( -1.000000000000000000, 0.000000000000000000, 0.000000000000000000 ) ) ;
#34203 = ORIENTED_EDGE ( 'NONE', *, *, #26099, .F. ) ;
#34204 = CARTESIAN_POINT ( 'NONE',  ( 805.6418435158337843, -341.4636090269705733, -363.8556311672236916 ) ) ;
#34205 = CARTESIAN_POINT ( 'NONE',  ( 804.1009440267234822, -215.4636090269709712, 314.0944755984392600 ) ) ;
#34206 = CARTESIAN_POINT ( 'NONE',  ( 755.3201227861273992, -315.7255117493286320, -345.3687786644892981 ) ) ;
#34207 = CARTESIAN_POINT ( 'NONE',  ( 783.0745993439762742, -176.1908817542438328, -365.1016975059196739 ) ) ;
#34208 = EDGE_CURVE ( 'NONE', #43693, #1691, #12107, .T. ) ;
#34209 = CARTESIAN_POINT ( 'NONE',  ( 811.0346526505616112, -38.63460265842041252, 323.0537975583477532 ) ) ;
#34210 =( GEOMETRIC_REPRESENTATION_CONTEXT ( 3 ) GLOBAL_UNCERTAINTY_ASSIGNED_CONTEXT ( ( #36592 ) ) GLOBAL_UNIT_ASSIGNED_CONTEXT ( ( #43968, #37497, #1925 ) ) REPRESENTATION_CONTEXT ( 'NONE', 'WORKASPACE' ) );
#34211 = DIRECTION ( 'NONE',  ( -0.000000000000000000, -0.000000000000000000, -1.000000000000000000 ) ) ;
#34212 = CARTESIAN_POINT ( 'NONE',  ( 772.4837098697145166, -383.3618753856920875, -374.5518280994205611 ) ) ;
#34213 = FACE_OUTER_BOUND ( 'NONE', #6179, .T. ) ;
#34214 = CARTESIAN_POINT ( 'NONE',  ( 807.2620300519052989, -336.0090635724251911, 318.0141637701419768 ) ) ;
#34215 = DIRECTION ( 'NONE',  ( 1.000000000000000000, 0.000000000000000000, 0.000000000000000000 ) ) ;
#34216 = CARTESIAN_POINT ( 'NONE',  ( 814.2001403089898304, -281.3618753856923718, 347.4397851343538264 ) ) ;
#34217 = CARTESIAN_POINT ( 'NONE',  ( 810.7187646348534145, -18.45278447660230725, -356.7737145352016341 ) ) ;
#34218 = ADVANCED_FACE ( 'NONE', ( #15569 ), #42604, .F. ) ;
#34219 = CARTESIAN_POINT ( 'NONE',  ( 804.6798772138708955, -255.7255117493287742, -334.6312213355107019 ) ) ;
#34220 = CARTESIAN_POINT ( 'NONE',  ( 831.1634899080286232, 239.9999999999998863, -199.9999999999999432 ) ) ;
#34221 = CARTESIAN_POINT ( 'NONE',  ( 794.9819416627830151, -396.9982390220556567, 319.9864689768909898 ) ) ;
#34222 = CARTESIAN_POINT ( 'NONE',  ( 804.8461984189677878, -170.1908817542438328, 336.9566956441385628 ) ) ;
#34223 = CARTESIAN_POINT ( 'NONE',  ( 775.9200461376533440, -47.80559628986931386, -315.3028492785443291 ) ) ;
#34224 = CARTESIAN_POINT ( 'NONE',  ( 805.9055244015594326, -75.62377810805104161, 315.8990559732753240 ) ) ;
#34225 = CARTESIAN_POINT ( 'NONE',  ( 788.7366044899766848, -371.9073299311465917, 316.5762568750059813 ) ) ;
#34226 = CARTESIAN_POINT ( 'NONE',  ( -454.7528517110262101, 230.0000000000001421, -2132.806278688367456 ) ) ;
#34227 =( NAMED_UNIT ( * ) SI_UNIT ( $, .STERADIAN. ) SOLID_ANGLE_UNIT ( ) );
#34228 = CARTESIAN_POINT ( 'NONE',  ( 755.5713283507202505, -437.3618753856919170, 334.6858677611754729 ) ) ;
#34229 = ORIENTED_EDGE ( 'NONE', *, *, #29559, .F. ) ;
#34230 = CARTESIAN_POINT ( 'NONE',  ( 758.0580252608178853, -54.45278447660219001, -328.0187753319985404 ) ) ;
#34231 = AXIS2_PLACEMENT_3D ( 'NONE', #29691, #40558, #1512 ) ;
#34232 = CARTESIAN_POINT ( 'NONE',  ( 755.0488828828309806, -353.8055962898683333, -344.1219089521771934 ) ) ;
#34234 = CARTESIAN_POINT ( 'NONE',  ( 802.1676090361155502, -182.6346026584199649, 327.8955696845344505 ) ) ;
#34233 = CARTESIAN_POINT ( 'NONE',  ( 778.1981804954714335, -178.2709662947835625, 314.8072714833589885 ) ) ;
#34235 = CARTESIAN_POINT ( 'NONE',  ( 776.2433038121456548, -372.8965053807773415, -374.8207195650711014 ) ) ;
#34236 = DIRECTION ( 'NONE',  ( 0.000000000000000000, 0.3826834323650836756, 0.9238795325112892920 ) ) ;
#34237 = ORIENTED_EDGE ( 'NONE', *, *, #6961, .F. ) ;
#34238 = CARTESIAN_POINT ( 'NONE',  ( 781.8018195045266339, -406.2709662947829088, 365.1927285166406705 ) ) ;
#34239 = ADVANCED_FACE ( 'NONE', ( #22484 ), #43963, .F. ) ;
#34240 = ORIENTED_EDGE ( 'NONE', *, *, #27881, .F. ) ;
#34241 = DIRECTION ( 'NONE',  ( 0.000000000000000000, 0.000000000000000000, 1.000000000000000000 ) ) ;
#34242 = CARTESIAN_POINT ( 'NONE',  ( 810.7187646348534145, -210.4527844766016926, -356.7737145352016341 ) ) ;
#34243 = CARTESIAN_POINT ( 'NONE',  ( 745.7998596910086917, -101.3618753856929544, 332.5602148656461168 ) ) ;
#34244 = AXIS2_PLACEMENT_3D ( 'NONE', #26834, #2355, #12327 ) ;
#34245 = EDGE_CURVE ( 'NONE', #40829, #22852, #36594, .T. ) ;
#34246 = ORIENTED_EDGE ( 'NONE', *, *, #59, .F. ) ;
#34247 = CARTESIAN_POINT ( 'NONE',  ( 768.0187753319979720, -200.6346026584199365, -318.0580252608186242 ) ) ;
#34248 = AXIS2_PLACEMENT_3D ( 'NONE', #38611, #6281, #10203 ) ;
#34249 = VERTEX_POINT ( 'NONE', #30323 ) ;
#34250 = CARTESIAN_POINT ( 'NONE',  ( 758.0580252608178853, -318.4527844766014368, -328.0187753319985404 ) ) ;
#34251 = CARTESIAN_POINT ( 'NONE',  ( 757.0176451133909268, -445.0999726633338582, -349.9200121543848354 ) ) ;
#34252 = VECTOR ( 'NONE', #32195, 1000.000000000000000 ) ;
#34253 = CARTESIAN_POINT ( 'NONE',  ( 770.0799878456142551, -205.9874144716870035, 362.9823548866085616 ) ) ;
#34255 = CARTESIAN_POINT ( 'NONE',  ( -728.8365100919714905, 260.0000000000001705, -197.2499999999891998 ) ) ;
#34254 = DIRECTION ( 'NONE',  ( -0.000000000000000000, 1.000000000000000000, -0.000000000000000000 ) ) ;
#34256 = DIRECTION ( 'NONE',  ( 0.000000000000000000, -0.000000000000000000, -1.000000000000000000 ) ) ;
#34257 = ORIENTED_EDGE ( 'NONE', *, *, #29765, .F. ) ;
#34258 = CARTESIAN_POINT ( 'NONE',  ( 805.1927285166397041, 7.183579159761247723, -341.8018195045277707 ) ) ;
#34259 = LINE ( 'NONE', #16492, #7043 ) ;
#34260 = DIRECTION ( 'NONE',  ( 0.000000000000000000, 0.000000000000000000, 1.000000000000000000 ) ) ;
#34261 = CARTESIAN_POINT ( 'NONE',  ( 778.7629533639073998, -248.7363362996981380, -375.0009284576466371 ) ) ;
#34262 = CIRCLE ( 'NONE', #23208, 2.749999999999863665 ) ;
#34263 = CARTESIAN_POINT ( 'NONE',  ( 764.1737431748507561, -106.3726999360621903, 371.6461892240376415 ) ) ;
#34264 = VECTOR ( 'NONE', #35037, 1000.000000000000000 ) ;
#34266 = CARTESIAN_POINT ( 'NONE',  ( 805.1927285166397041, -232.8164208402379245, -341.8018195045277707 ) ) ;
#34265 = CYLINDRICAL_SURFACE ( 'NONE', #26093, 2.749999999999863665 ) ;
#34267 = ADVANCED_FACE ( 'NONE', ( #26850 ), #25949, .F. ) ;
#34268 = CARTESIAN_POINT ( 'NONE',  ( 766.7756240680305382, -374.5328690171410813, -361.5560724626415663 ) ) ;
#34269 = CARTESIAN_POINT ( 'NONE',  ( 747.6481478633932056, -253.0999726633345119, -353.4146539503763620 ) ) ;
#34270 = DIRECTION ( 'NONE',  ( -1.000000000000000000, -4.625929269271485914E-16, 0.000000000000000000 ) ) ;
#34271 = CARTESIAN_POINT ( 'NONE',  ( -26.63011601220122060, -110.5936016518799221, 750.6326042729449455 ) ) ;
#34272 = CARTESIAN_POINT ( 'NONE',  ( 793.0897708529556667, -78.55451811788046257, -361.3366627262616362 ) ) ;
#34273 = CARTESIAN_POINT ( 'NONE',  ( 790.9844846989617508, -430.3726999360611671, 317.2208543904092721 ) ) ;
#34274 = EDGE_CURVE ( 'NONE', #8204, #36310, #5618, .T. ) ;
#34275 = DIRECTION ( 'NONE',  ( 0.000000000000000000, 0.000000000000000000, -1.000000000000000000 ) ) ;
#34276 = CARTESIAN_POINT ( 'NONE',  ( 803.2186876482843445, -415.9874144716862361, -350.0220218866286928 ) ) ;
#34277 = CARTESIAN_POINT ( 'NONE',  ( 755.2512626584698410, -271.5436935675106156, -315.2512626584710915 ) ) ;
#34278 = CARTESIAN_POINT ( 'NONE',  ( -454.7528517110261532, 8.550106180308601742E-14, 339.9999999999999432 ) ) ;
#34279 = DIRECTION ( 'NONE',  ( 0.000000000000000000, 0.000000000000000000, 1.000000000000000000 ) ) ;
#34280 = CARTESIAN_POINT ( 'NONE',  ( 788.7366044899766848, -35.90732993114770011, -316.5762568750059813 ) ) ;
#34281 = CARTESIAN_POINT ( 'NONE',  ( 814.8207195650702488, -218.1908817542437191, 336.2433038121456548 ) ) ;
#34282 = CARTESIAN_POINT ( 'NONE',  ( 759.8311093483677041, -166.1692326535053041, -310.9282345327691814 ) ) ;
#34283 = CARTESIAN_POINT ( 'NONE',  ( 759.0252816721024374, -192.9982390220562820, 368.0189434323527280 ) ) ;
#34284 = CARTESIAN_POINT ( 'NONE',  ( 754.9967657858570647, -409.5436935675101040, -365.0032342141425374 ) ) ;
#34285 = EDGE_CURVE ( 'NONE', #10220, #45115, #40959, .T. ) ;
#34286 = EDGE_CURVE ( 'NONE', #41197, #8149, #19042, .T. ) ;
#34287 = DIRECTION ( 'NONE',  ( 1.000000000000000000, -0.000000000000000000, -0.000000000000000000 ) ) ;
#34288 = VECTOR ( 'NONE', #23134, 1000.000000000000000 ) ;
#34289 = CARTESIAN_POINT ( 'NONE',  ( 764.8639956371174549, -296.0891481129650629, 319.7806653035542013 ) ) ;
#34290 = CIRCLE ( 'NONE', #14399, 6.118999999999985562 ) ;
#34291 = CARTESIAN_POINT ( 'NONE',  ( 805.2837595273609850, -50.73633629969874193, 340.5290396650784714 ) ) ;
#34292 = CARTESIAN_POINT ( 'NONE',  ( 797.8594530101008786, -421.5436935675101040, -322.1405469898980982 ) ) ;
#34293 = AXIS2_PLACEMENT_3D ( 'NONE', #27755, #34460, #14130 ) ;
#34294 = CARTESIAN_POINT ( 'NONE',  ( 786.4999999999993179, 26.27639943461418426, 900.0000000000004547 ) ) ;
#34295 = CARTESIAN_POINT ( 'NONE',  ( 879.9999999999990905, 479.9999999999998863, -210.0000000000000000 ) ) ;
#34297 = CARTESIAN_POINT ( 'NONE',  ( 774.6312213355099630, -335.3618753856920307, 364.6798772138717482 ) ) ;
#34296 = CARTESIAN_POINT ( 'NONE',  ( 798.7617431975189675, -75.62377810805104161, 323.0428371773161871 ) ) ;
#34298 = VERTEX_POINT ( 'NONE', #5168 ) ;
#34299 = CARTESIAN_POINT ( 'NONE',  ( 796.7845633553578182, -273.6237781080504305, -358.5707757039688204 ) ) ;
#34300 = CARTESIAN_POINT ( 'NONE',  ( 788.8264449731200330, -45.18005720387493085, 363.6646147819171233 ) ) ;
#34301 = AXIS2_PLACEMENT_3D ( 'NONE', #9241, #5771, #39199 ) ;
#34302 = CARTESIAN_POINT ( 'NONE',  ( 807.5423716828161105, -249.0783235625959549, -362.2119215644372048 ) ) ;
#34303 = LINE ( 'NONE', #16993, #36689 ) ;
#34304 = CARTESIAN_POINT ( 'NONE',  ( 813.2346286133761168, -365.2601417444137155, 328.9521613784389160 ) ) ;
#34305 = VERTEX_POINT ( 'NONE', #16470 ) ;
#34306 = CARTESIAN_POINT ( 'NONE',  ( 804.4286716492782716, -281.3618753856923718, 345.3141322388244703 ) ) ;
#34307 = AXIS2_PLACEMENT_3D ( 'NONE', #1732, #26906, #33622 ) ;
#34308 = CARTESIAN_POINT ( 'NONE',  ( 804.7487373415286811, 4.456306432488530866, 364.7487373415288516 ) ) ;
#34309 = ADVANCED_FACE ( 'NONE', ( #33133, #40300 ), #12340, .T. ) ;
#34310 = CARTESIAN_POINT ( 'NONE',  ( 772.3691319403857278, -23.26014174441484883, -315.8894580844506663 ) ) ;
#34311 = CARTESIAN_POINT ( 'NONE',  ( 804.9363028652555840, -160.2709662947836762, -338.2165204200192079 ) ) ;
#34312 = CARTESIAN_POINT ( 'NONE',  ( 757.8323909638827445, -386.6346026584191691, 352.1044303154654358 ) ) ;
#34313 = CONICAL_SURFACE ( 'NONE', #32109, 8.025000000000003908, 0.7853981633974410625 ) ;
#34314 = CARTESIAN_POINT ( 'NONE',  ( 755.2512626584698410, -103.5436935675111272, -315.2512626584710915 ) ) ;
#34315 = CARTESIAN_POINT ( 'NONE',  ( 801.9419747391806368, -114.4527844766020053, -351.9812246680014027 ) ) ;
#34316 = ORIENTED_EDGE ( 'NONE', *, *, #43568, .T. ) ;
#34317 = CARTESIAN_POINT ( 'NONE',  ( 760.7433823573367135, -36.00906357242605793, -355.9930595647440441 ) ) ;
#34318 = CARTESIAN_POINT ( 'NONE',  ( 754.7162404726377645, -350.7363362996978253, -339.4709603349214717 ) ) ;
#34320 = CARTESIAN_POINT ( 'NONE',  ( 769.9779781133707957, -403.0999726633339719, 316.7813123517150871 ) ) ;
#34319 = CARTESIAN_POINT ( 'NONE',  ( 785.3687786644884454, -83.36187538569296862, 315.3201227861279676 ) ) ;
#34321 = CARTESIAN_POINT ( 'NONE',  ( 761.2382568024794409, -87.62377810805102740, 356.9571628226838129 ) ) ;
#34324 = CARTESIAN_POINT ( 'NONE',  ( 791.1614460488616487, -347.2601417444138860, 373.5763878283158874 ) ) ;
#34323 = CARTESIAN_POINT ( 'NONE',  ( 879.9999999999992042, 240.0000000000000568, -244.9999999999999716 ) ) ;
#34322 = LINE ( 'NONE', #31085, #27724 ) ;
#34325 = CARTESIAN_POINT ( 'NONE',  ( 780.5236548040995785, -356.7363362996978253, -314.9735926884559944 ) ) ;
#34326 = CARTESIAN_POINT ( 'NONE',  ( 774.6858677611749044, -345.7255117493285184, -315.5713283507209894 ) ) ;
#34327 = CARTESIAN_POINT ( 'NONE',  ( 795.8262568251477660, -118.3726999360621619, -308.3538107759623585 ) ) ;
#34328 = AXIS2_PLACEMENT_3D ( 'NONE', #30735, #16180, #20096 ) ;
#34329 = CARTESIAN_POINT ( 'NONE',  ( 764.1737431748507561, -10.37269993606250473, 371.6461892240376415 ) ) ;
#34330 = VECTOR ( 'NONE', #40587, 1000.000000000000000 ) ;
#34332 = DIRECTION ( 'NONE',  ( -0.7071067811857625340, -8.659560562345319848E-17, -0.7071067811873326114 ) ) ;
#34331 = DIRECTION ( 'NONE',  ( 0.000000000000000000, 0.000000000000000000, -1.000000000000000000 ) ) ;
#34333 = EDGE_CURVE ( 'NONE', #13729, #12447, #29652, .T. ) ;
#34334 = CARTESIAN_POINT ( 'NONE',  ( 790.8726784830453198, -274.7146871989594388, -362.5472867521010585 ) ) ;
#34335 = CARTESIAN_POINT ( 'NONE',  ( 813.5763878283155464, -147.8272453906075157, -351.1614460488615350 ) ) ;
#34336 = CARTESIAN_POINT ( 'NONE',  ( -180.7583438952258916, 294.6698570112193920, -274.9999999999999432 ) ) ;
#34337 = CARTESIAN_POINT ( 'NONE',  ( -775.4999999999993179, -513.1383975375929367, -369.9999999999999432 ) ) ;
#34338 = CARTESIAN_POINT ( 'NONE',  ( 804.1105419155481968, -315.8272453906070609, 347.6308680596136469 ) ) ;
#34339 = ADVANCED_FACE ( 'NONE', ( #16244 ), #12769, .T. ) ;
#34340 = ORIENTED_EDGE ( 'NONE', *, *, #1266, .F. ) ;
#34341 = CARTESIAN_POINT ( 'NONE',  ( 799.9636004259356241, -310.9181544815160123, 311.2241431872006956 ) ) ;
#34342 = CARTESIAN_POINT ( 'NONE',  ( 808.3070685750232087, -186.9982390220563104, -361.1904061080339829 ) ) ;
#34343 = CARTESIAN_POINT ( 'NONE',  ( -180.7583438952258916, 294.6698570112193920, -274.9999999999999432 ) ) ;
#34344 = CIRCLE ( 'NONE', #24745, 20.00000000000001776 ) ;
#34345 = CARTESIAN_POINT ( 'NONE',  ( 813.5763878283155464, -123.8272453906076009, 351.1614460488615350 ) ) ;
#34346 = CARTESIAN_POINT ( 'NONE',  ( 805.0032342141412300, -301.5436935675105588, -314.9967657858571783 ) ) ;
#34347 = AXIS2_PLACEMENT_3D ( 'NONE', #17474, #31555, #45655 ) ;
#34348 = DIRECTION ( 'NONE',  ( 1.000000000000000000, 0.000000000000000000, -0.000000000000000000 ) ) ;
#34349 = DIRECTION ( 'NONE',  ( -1.880165489482579047E-16, -1.000000000000000000, -0.000000000000000000 ) ) ;
#34350 = CARTESIAN_POINT ( 'NONE',  ( 791.9812246680005501, -140.6346026584201070, 361.9419747391813189 ) ) ;
#34351 = VERTEX_POINT ( 'NONE', #11878 ) ;
#34352 = CARTESIAN_POINT ( 'NONE',  ( 804.1009440267234822, -407.4636090269703459, 314.0944755984392600 ) ) ;
#34353 = CARTESIAN_POINT ( 'NONE',  ( 813.9316612368132837, -391.4419599262317888, -348.6739635108323228 ) ) ;
#34354 = CARTESIAN_POINT ( 'NONE',  ( 745.0891759886404770, -124.2709662947837899, -342.4968714119734159 ) ) ;
#34355 = CARTESIAN_POINT ( 'NONE',  ( 763.0428371773158460, -59.46360902697142592, 358.7617431975195359 ) ) ;
#34356 = CARTESIAN_POINT ( 'NONE',  ( 813.1304606946830518, -377.9073299311466485, -352.3570229623690580 ) ) ;
#34357 = DIRECTION ( 'NONE',  ( 1.000000000000000000, 0.000000000000000000, 0.000000000000000000 ) ) ;
#34358 = CARTESIAN_POINT ( 'NONE',  ( 787.6308680596127942, -419.2601417444136587, 364.1105419155492768 ) ) ;
#34359 = ORIENTED_EDGE ( 'NONE', *, *, #12538, .T. ) ;
#34360 = CARTESIAN_POINT ( 'NONE',  ( 757.8323909638827445, -266.6346026584197375, 352.1044303154654358 ) ) ;
#34361 = CARTESIAN_POINT ( 'NONE',  ( 744.8212110874229666, -138.8965053807781374, -336.2046728542121627 ) ) ;
#34362 = CARTESIAN_POINT ( 'NONE',  ( 794.9999999999993179, 212.6707680665973612, -236.5295014342203785 ) ) ;
#34363 = CARTESIAN_POINT ( 'NONE',  ( 752.4576283171824116, -261.0783235625959264, 317.7880784355627952 ) ) ;
#34364 = CARTESIAN_POINT ( 'NONE',  ( 756.3353852180820240, -101.9073299311474869, 331.1735550268787733 ) ) ;
#34365 = VERTEX_POINT ( 'NONE', #26414 ) ;
#34366 = VECTOR ( 'NONE', #3318, 1000.000000000000000 ) ;
#34367 = CARTESIAN_POINT ( 'NONE',  ( 755.0488828828309806, -17.80559628986940979, -344.1219089521771934 ) ) ;
#34368 = CARTESIAN_POINT ( 'NONE',  ( 757.8323909638827445, -266.6346026584197375, 352.1044303154654358 ) ) ;
#34369 = CARTESIAN_POINT ( 'NONE',  ( 815.2698199232961542, 7.183579159761247723, -342.5225473063383106 ) ) ;
#34370 = CARTESIAN_POINT ( 'NONE',  ( 792.1975848984933464, -449.0899794596732022, 370.7630750413119927 ) ) ;
#34371 = ORIENTED_EDGE ( 'NONE', *, *, #13291, .T. ) ;
#34372 = CARTESIAN_POINT ( 'NONE',  ( 804.6798772138708955, -183.7255117493290015, -334.6312213355107019 ) ) ;
#34373 = CARTESIAN_POINT ( 'NONE',  ( 745.1792804349281596, -398.1908817542431507, -343.7566961878542884 ) ) ;
#34374 = AXIS2_PLACEMENT_3D ( 'NONE', #8969, #40618, #13133 ) ;
#34375 = CARTESIAN_POINT ( 'NONE',  ( 762.3223304703356007, -247.5436935675106724, -322.3223304703362828 ) ) ;
#34376 = VECTOR ( 'NONE', #45484, 1000.000000000000000 ) ;
#34378 = CARTESIAN_POINT ( 'NONE',  ( 747.3154664389472828, -259.9874144716869182, 326.4474001241230781 ) ) ;
#34377 = CARTESIAN_POINT ( 'NONE',  ( 744.7301800767020268, -364.8164208402375266, 337.4774526936615189 ) ) ;
#34379 = CARTESIAN_POINT ( 'NONE',  ( 793.0897708529556667, -270.5545181178798657, -361.3366627262616362 ) ) ;
#34380 = CARTESIAN_POINT ( 'NONE',  ( 774.6312213355099630, -215.3618753856925423, -364.6798772138717482 ) ) ;
#34381 = CARTESIAN_POINT ( 'NONE',  ( 785.3141322388236176, -429.7255117493282910, -364.4286716492789537 ) ) ;
#34382 = CARTESIAN_POINT ( 'NONE',  ( 788.7366044899766848, -227.9073299311471033, 316.5762568750059813 ) ) ;
#34383 = ORIENTED_EDGE ( 'NONE', *, *, #9705, .T. ) ;
#34384 = CARTESIAN_POINT ( 'NONE',  ( 772.5602148656447525, -345.7255117493285184, 305.7998596910095443 ) ) ;
#34385 = FACE_OUTER_BOUND ( 'NONE', #39933, .T. ) ;
#34386 = CARTESIAN_POINT ( 'NONE',  ( 768.9521613784389729, -9.827245390607961539, -373.2346286133773106 ) ) ;
#34387 = CARTESIAN_POINT ( 'NONE',  ( 770.1068079863199500, 16.45630643248850333, 316.7980005127122922 ) ) ;
#34388 = CARTESIAN_POINT ( 'NONE',  ( 914.9999999999992042, 74.99999999999984368, 360.0000000000000000 ) ) ;
#34389 = CARTESIAN_POINT ( 'NONE',  ( 763.8424801807145741, -234.0090635724255037, 320.5453621957614700 ) ) ;
#34390 = CARTESIAN_POINT ( 'NONE',  ( 759.9864689768902508, -122.0891481129656171, 354.9819416627836404 ) ) ;
#34391 = EDGE_LOOP ( 'NONE', ( #17267, #39509, #18448, #22214, #44095, #33975 ) ) ;
#34392 = CARTESIAN_POINT ( 'NONE',  ( 784.1219089521767955, -21.28179084515337749, -315.0488828828318333 ) ) ;
#34393 = CARTESIAN_POINT ( 'NONE',  ( 777.4774526936600978, -58.27096629478398881, -304.7301800767028226 ) ) ;
#34394 = CARTESIAN_POINT ( 'NONE',  ( 761.2382568024794409, -255.6237781080504874, 356.9571628226838129 ) ) ;
#34395 = VECTOR ( 'NONE', #35873, 999.9999999999998863 ) ;
#34396 = CARTESIAN_POINT ( 'NONE',  ( 804.6798772138708955, -423.7255117493281205, -334.6312213355107019 ) ) ;
#34397 = CARTESIAN_POINT ( 'NONE',  ( 765.0180583372156207, -48.99823902205675807, -360.0135310231089534 ) ) ;
#34398 = CARTESIAN_POINT ( 'NONE',  ( 810.4231160770870019, -0.5545181178807169209, 321.9338519418446936 ) ) ;
#34399 = DIRECTION ( 'NONE',  ( 0.000000000000000000, 0.000000000000000000, 1.000000000000000000 ) ) ;
#34401 = VECTOR ( 'NONE', #39129, 1000.000000000000114 ) ;
#34400 = CARTESIAN_POINT ( 'NONE',  ( 763.0537975583475827, -216.4527844766016926, -371.0346526505627480 ) ) ;
#34402 = CARTESIAN_POINT ( 'NONE',  ( 745.4481719005789273, -99.72551174932928575, 347.5162901302853129 ) ) ;
#34403 = CARTESIAN_POINT ( 'NONE',  ( 814.2001403089898304, -185.3618753856926844, 347.4397851343538264 ) ) ;
#34404 = VECTOR ( 'NONE', #28362, 999.9999999999998863 ) ;
#34405 = LINE ( 'NONE', #6684, #35791 ) ;
#34406 = LINE ( 'NONE', #2775, #40215 ) ;
#34407 = CARTESIAN_POINT ( 'NONE',  ( 791.1614460488616487, -275.2601417444140566, -373.5763878283158874 ) ) ;
#34408 = CARTESIAN_POINT ( 'NONE',  ( 749.5768839229115201, -420.5545181178793541, 358.0661480581553064 ) ) ;
#34409 = CARTESIAN_POINT ( 'NONE',  ( 814.9108240113580450, -280.2709662947833067, -337.5031285880265273 ) ) ;
#34410 = CYLINDRICAL_SURFACE ( 'NONE', #22083, 1.000000000000000888 ) ;
#34411 = CARTESIAN_POINT ( 'NONE',  ( 754.9967657858570647, -385.5436935675102745, 365.0032342141425374 ) ) ;
#34412 = CARTESIAN_POINT ( 'NONE',  ( 763.0537975583476964, -24.45278447660228949, 371.0346526505628617 ) ) ;
#34413 = CARTESIAN_POINT ( 'NONE',  ( 798.0661480581538854, -26.53286901714210799, -309.5768839229118043 ) ) ;
#34414 = CARTESIAN_POINT ( 'NONE',  ( 759.9864689768902508, -338.0891481129649492, -354.9819416627836404 ) ) ;
#34415 = AXIS2_PLACEMENT_3D ( 'NONE', #1549, #12632, #15646 ) ;
#34416 = CARTESIAN_POINT ( 'NONE',  ( 802.7791456095903868, -28.71468719896028077, 329.0155153010375102 ) ) ;
#34417 = CARTESIAN_POINT ( 'NONE',  ( 813.9316612368132837, -55.44195992623293989, -348.6739635108323228 ) ) ;
#34418 = CARTESIAN_POINT ( 'NONE',  ( 779.4709603349208464, -168.3510508353234911, -314.7162404726379918 ) ) ;
#34419 = CARTESIAN_POINT ( 'NONE',  ( 758.0141637701419768, -183.0783235625961538, 367.2620300519063790 ) ) ;
#34420 = CARTESIAN_POINT ( 'NONE',  ( 766.5853460496234675, -181.9874144716870887, 372.3518521366060554 ) ) ;
#34421 = ORIENTED_EDGE ( 'NONE', *, *, #6961, .T. ) ;
#34422 = CARTESIAN_POINT ( 'NONE',  ( 754.8072714833581358, -76.81642084023845030, -338.1981804954720587 ) ) ;
#34423 = CARTESIAN_POINT ( 'NONE',  ( 805.1016975059191054, -150.8965053807781089, -343.0745993439771837 ) ) ;
#34424 = PRODUCT_DEFINITION_CONTEXT ( 'detailed design', #21377, 'design' ) ;
#34425 = CARTESIAN_POINT ( 'NONE',  ( 771.2633955100217236, -167.9073299311473022, 363.4237431249939618 ) ) ;
#34426 = CARTESIAN_POINT ( 'NONE',  ( 781.2497674668890113, 11.64894916467595642, -375.3608509340180603 ) ) ;
#34428 = CARTESIAN_POINT ( 'NONE',  ( 765.0180583372156207, -288.9982390220559978, 360.0135310231089534 ) ) ;
#34427 = CARTESIAN_POINT ( 'NONE',  ( 759.7806653035534055, -294.9982390220560546, 324.8639956371180801 ) ) ;
#34429 = DIRECTION ( 'NONE',  ( 1.000000000000000000, -1.880165489482579047E-16, 0.000000000000000000 ) ) ;
#34430 = ORIENTED_EDGE ( 'NONE', *, *, #4683, .F. ) ;
#34431 = CARTESIAN_POINT ( 'NONE',  ( 802.7791456095903868, -28.71468719896028077, 329.0155153010375102 ) ) ;
#34432 = CARTESIAN_POINT ( 'NONE',  ( 812.3518521366052028, -313.0999726633342561, -326.5853460496235243 ) ) ;
#34433 = ITEM_DEFINED_TRANSFORMATION ( 'NONE', 'NONE', #35614,  #26858 ) ;
#34434 = CIRCLE ( 'NONE', #7183, 10.00000000000000888 ) ;
#34435 = CARTESIAN_POINT ( 'NONE',  ( 759.0252816721024374, -240.9982390220561683, 368.0189434323527280 ) ) ;
#34436 = CARTESIAN_POINT ( 'NONE',  ( 775.8780910478218402, -321.2817908451525000, 364.9511171171680530 ) ) ;
#34437 = CARTESIAN_POINT ( 'NONE',  ( 759.2295555964440155, -424.1692326535044799, 353.9708237608231229 ) ) ;
#34439 = VECTOR ( 'NONE', #3147, 1000.000000000000000 ) ;
#34438 = CARTESIAN_POINT ( 'NONE',  ( 804.6971507214547046, -147.2817908451529547, -344.0799538623459739 ) ) ;
#34440 = CARTESIAN_POINT ( 'NONE',  ( 764.8639956371174549, -128.0891481129655176, -319.7806653035542013 ) ) ;
#34441 = CARTESIAN_POINT ( 'NONE',  ( 785.3687786644885591, -299.3618753856923149, -315.3201227861280813 ) ) ;
#34442 = EDGE_LOOP ( 'NONE', ( #21993, #44675, #32499, #19951 ) ) ;
#34443 = CARTESIAN_POINT ( 'NONE',  ( 802.1676090361156639, -422.6346026584192259, -327.8955696845344505 ) ) ;
#34444 = VECTOR ( 'NONE', #39345, 1000.000000000000000 ) ;
#34445 = CARTESIAN_POINT ( 'NONE',  ( 795.9930595647434757, -315.0783235625957559, 320.7433823573372820 ) ) ;
#34446 = CARTESIAN_POINT ( 'NONE',  ( -208.8365100919714052, 230.0000000000000853, -197.2499999999928377 ) ) ;
#34447 = CARTESIAN_POINT ( 'NONE',  ( 919.9999999999993179, 219.9999999999998863, 360.0000000000000000 ) ) ;
#34448 = AXIS2_PLACEMENT_3D ( 'NONE', #38967, #826, #35467 ) ;
#34449 = CARTESIAN_POINT ( 'NONE',  ( 766.0291762391763086, -106.9181544815167371, 360.7704444035551319 ) ) ;
#34450 = CARTESIAN_POINT ( 'NONE',  ( 804.9363028652555840, 7.729033705215793582, 338.2165204200192079 ) ) ;
#34451 = VERTEX_POINT ( 'NONE', #8654 ) ;
#34452 = CARTESIAN_POINT ( 'NONE',  ( 814.4686193811664907, -339.2817908451524431, -346.2056067578752732 ) ) ;
#34453 = EDGE_CURVE ( 'NONE', #3603, #29779, #21929, .T. ) ;
#34454 = CARTESIAN_POINT ( 'NONE',  ( 758.4439275373578084, -228.5545181178799794, 353.2243759319684386 ) ) ;
#34455 = CARTESIAN_POINT ( 'NONE',  ( 791.0478386215596629, -237.8272453906072599, 306.7653713866226326 ) ) ;
#34456 = CARTESIAN_POINT ( 'NONE',  ( 797.6776695296629214, -331.5436935675104451, -357.6776695296636603 ) ) ;
#34457 = DIRECTION ( 'NONE',  ( -0.000000000000000000, -1.000000000000000000, -0.000000000000000000 ) ) ;
#34458 = CARTESIAN_POINT ( 'NONE',  ( 790.0220218866281812, -175.0999726633346825, -363.2186876482849129 ) ) ;
#34459 = CARTESIAN_POINT ( 'NONE',  ( 800.9747183278959710, -36.99823902205679360, 311.9810565676471583 ) ) ;
#34460 = DIRECTION ( 'NONE',  ( 1.892425610156518354E-16, 1.000000000000000000, -0.000000000000000000 ) ) ;
#34461 = CARTESIAN_POINT ( 'NONE',  ( 814.5518280994195948, -375.7255117493284047, -332.4837098697145166 ) ) ;
#34462 = CARTESIAN_POINT ( 'NONE',  ( 989.9999999999992042, 249.9999999999998863, -360.0000000000000000 ) ) ;
#34463 = VECTOR ( 'NONE', #33009, 1000.000000000000000 ) ;
#34464 = CARTESIAN_POINT ( 'NONE',  ( 744.6391490659812007, -302.7363362996979959, 338.7502325331110455 ) ) ;
#34465 = CARTESIAN_POINT ( 'NONE',  ( 998.9999999999992042, -600.0000000000001137, -360.0000000000000000 ) ) ;
#34466 = CARTESIAN_POINT ( 'NONE',  ( 744.7301800767019131, -292.8164208402376971, 337.4774526936615757 ) ) ;
#34467 = CARTESIAN_POINT ( 'NONE',  ( 805.0032342141412300, -13.54369356751140785, -314.9967657858571783 ) ) ;
#34468 = AXIS2_PLACEMENT_3D ( 'NONE', #17489, #38972, #34572 ) ;
#34469 = CARTESIAN_POINT ( 'NONE',  ( 759.9864689768902508, -242.0891481129652618, -354.9819416627836404 ) ) ;
#34470 = FACE_BOUND ( 'NONE', #20902, .T. ) ;
#34471 = CARTESIAN_POINT ( 'NONE',  ( 804.4286716492782716, -377.3618753856920875, 345.3141322388244703 ) ) ;
#34472 = CARTESIAN_POINT ( 'NONE',  ( 802.5472867521000353, -148.3726999360620198, 350.8726784830461156 ) ) ;
#34473 = CARTESIAN_POINT ( 'NONE',  ( 744.6391490659812007, -38.73633629969877035, -338.7502325331110455 ) ) ;
#34474 = CARTESIAN_POINT ( 'NONE',  ( 772.3691319403857278, -47.26014174441477422, -315.8894580844506663 ) ) ;
#34475 = CARTESIAN_POINT ( 'NONE',  ( 803.8556311672234642, -57.62377810805111267, 365.6418435158340117 ) ) ;
#34476 = CARTESIAN_POINT ( 'NONE',  ( 764.8639956371174549, -368.0891481129647786, 319.7806653035542581 ) ) ;
#34477 = CIRCLE ( 'NONE', #19702, 10.00000000000000888 ) ;
#34478 = CARTESIAN_POINT ( 'NONE',  ( -911.9749999999993406, 219.9999999999998863, -360.0000000000000000 ) ) ;
#34479 = SURFACE_STYLE_USAGE ( .BOTH. , #27319 ) ;
#34480 = CARTESIAN_POINT ( 'NONE',  ( 804.6798772138708955, -447.7255117493280636, 334.6312213355107019 ) ) ;
#34481 = ORIENTED_EDGE ( 'NONE', *, *, #44997, .F. ) ;
#34482 = CARTESIAN_POINT ( 'NONE',  ( 756.3353852180819104, -77.90732993114757221, -331.1735550268788302 ) ) ;
#34483 = CARTESIAN_POINT ( 'NONE',  ( 800.7704444035546203, -364.1692326535046504, -326.0291762391768771 ) ) ;
#34485 = CARTESIAN_POINT ( 'NONE',  ( 771.1735550268780344, -201.1800572038744690, 316.3353852180828198 ) ) ;
#34484 = CARTESIAN_POINT ( 'NONE',  ( 756.5762568750052424, -195.1800572038744974, 348.7366044899774238 ) ) ;
#34486 = CARTESIAN_POINT ( 'NONE',  ( 746.0683387631852383, -355.4419599262319593, -331.3260364891676204 ) ) ;
#34487 = LINE ( 'NONE', #38639, #13822 ) ;
#34488 = ORIENTED_EDGE ( 'NONE', *, *, #36506, .T. ) ;
#34489 = CARTESIAN_POINT ( 'NONE',  ( 800.0135310231082713, -398.0891481129647218, 325.0180583372163028 ) ) ;
#34490 = EDGE_LOOP ( 'NONE', ( #45398, #15924, #20687, #13018 ) ) ;
#34491 = CARTESIAN_POINT ( 'NONE',  ( 814.2001403089898304, -233.3618753856925423, -347.4397851343538264 ) ) ;
#34492 = CARTESIAN_POINT ( 'NONE',  ( 792.3570229623691148, -117.1800572038747106, 373.1304606946836770 ) ) ;
#34493 = VERTEX_POINT ( 'NONE', #19252 ) ;
#34494 = CARTESIAN_POINT ( 'NONE',  ( 759.7806653035535192, -222.9982390220561683, -324.8639956371181370 ) ) ;
#34495 = EDGE_CURVE ( 'NONE', #31811, #10985, #27094, .T. ) ;
#34496 = ORIENTED_EDGE ( 'NONE', *, *, #18978, .F. ) ;
#34497 = CARTESIAN_POINT ( 'NONE',  ( 771.2633955100217236, -311.9073299311468759, -363.4237431249939618 ) ) ;
#34498 = CARTESIAN_POINT ( 'NONE',  ( 797.6776695296629214, 4.456306432488530866, -357.6776695296636603 ) ) ;
#34499 = CARTESIAN_POINT ( 'NONE',  ( 757.2208543904082489, -184.7146871989598083, 350.9844846989624330 ) ) ;
#34501 = DIRECTION ( 'NONE',  ( 0.000000000000000000, 1.000000000000000000, 0.000000000000000000 ) ) ;
#34500 = DIRECTION ( 'NONE',  ( 0.000000000000000000, 0.000000000000000000, 1.000000000000000000 ) ) ;
#34502 = ADVANCED_FACE ( 'NONE', ( #37026 ), #5380, .T. ) ;
#34503 = LINE ( 'NONE', #42115, #42750 ) ;
#34504 = VERTEX_POINT ( 'NONE', #24528 ) ;
#34505 = CARTESIAN_POINT ( 'NONE',  ( 796.9571628226829034, -455.4636090269701754, -321.2382568024804641 ) ) ;
#34506 = CARTESIAN_POINT ( 'NONE',  ( 766.1799889109151991, 20.32535068748918050, -313.3728091324376237 ) ) ;
#34507 = CARTESIAN_POINT ( 'NONE',  ( -879.9999999999992042, 260.0000000000002274, -219.9999999999999716 ) ) ;
#34508 = ORIENTED_EDGE ( 'NONE', *, *, #23271, .T. ) ;
#34509 = CARTESIAN_POINT ( 'NONE',  ( 745.5313806188320314, -255.2817908451526705, -333.7943932421247268 ) ) ;
#34510 = CARTESIAN_POINT ( 'NONE',  ( 760.0363995740630116, -106.9181544815167371, 368.7758568127991907 ) ) ;
#34512 = CARTESIAN_POINT ( 'NONE',  ( 754.8072714833581358, -220.8164208402379529, -338.1981804954720587 ) ) ;
#34511 = CARTESIAN_POINT ( 'NONE',  ( -786.4999999999993179, -544.8427095258973623, -369.9999999999999432 ) ) ;
#34513 = CARTESIAN_POINT ( 'NONE',  ( 802.7791456095903868, -412.7146871989590409, -329.0155153010375102 ) ) ;
#34514 = CARTESIAN_POINT ( 'NONE',  ( 811.3240766477731540, -244.3726999360617924, -355.6651683502462902 ) ) ;
#34515 = CARTESIAN_POINT ( 'NONE',  ( 769.9999999999992042, 205.0000000000000568, -319.9999999999999432 ) ) ;
#34516 = LINE ( 'NONE', #40754, #29711 ) ;
#34517 = CARTESIAN_POINT ( 'NONE',  ( 776.9254006560222479, -92.19088175424406018, -314.8983024940802125 ) ) ;
#34518 = CARTESIAN_POINT ( 'NONE',  ( 804.8461984189677878, -434.1908817542430370, 336.9566956441385628 ) ) ;
#34519 = CARTESIAN_POINT ( 'NONE',  ( 814.2805881961230625, -361.6454272087887603, 331.2368401574024119 ) ) ;
#34520 = CARTESIAN_POINT ( 'NONE',  ( 441.1634899080286232, 258.0939999999999372, -199.9999999999972431 ) ) ;
#34521 = CARTESIAN_POINT ( 'NONE',  ( 760.5453621957607311, -429.0783235625953580, -323.8424801807151425 ) ) ;
#34522 = CARTESIAN_POINT ( 'NONE',  ( 748.9653473494365699, -290.6346026584196238, -356.9462024416520762 ) ) ;
#34523 = SURFACE_SIDE_STYLE ('',( #6793 ) ) ;
#34524 = FACE_OUTER_BOUND ( 'NONE', #4617, .T. ) ;
#34525 = CARTESIAN_POINT ( 'NONE',  ( 768.0187753319979720, -80.63460265842029173, -318.0580252608186242 ) ) ;
#34526 = CARTESIAN_POINT ( 'NONE',  ( 811.3240766477731540, -220.3726999360618208, 355.6651683502462902 ) ) ;
#34527 = CARTESIAN_POINT ( 'NONE',  ( 771.2368401574024119, -157.4419599262326130, -374.2805881961240857 ) ) ;
#34528 = CARTESIAN_POINT ( 'NONE',  ( 801.1904061080336987, -188.0891481129653187, 368.3070685750235498 ) ) ;
#34529 = CARTESIAN_POINT ( 'NONE',  ( 763.2262854647970016, -416.6346026584192259, -309.2812353651462445 ) ) ;
#34530 = CARTESIAN_POINT ( 'NONE',  ( -959.5497976682736407, 240.0000000000002274, 350.0000000000000000 ) ) ;
#34531 = CARTESIAN_POINT ( 'NONE',  ( 781.7834795799800531, -274.8164208402378108, 315.0636971347436202 ) ) ;
#34532 = CARTESIAN_POINT ( 'NONE',  ( 804.6971507214547046, -75.28179084515321051, 344.0799538623459739 ) ) ;
#34533 = CARTESIAN_POINT ( 'NONE',  ( 768.0187753319979720, -440.6346026584191122, -318.0580252608186242 ) ) ;
#34534 = DIRECTION ( 'NONE',  ( 0.000000000000000000, 1.000000000000000000, 0.000000000000000000 ) ) ;
#34535 = DIRECTION ( 'NONE',  ( -1.000000000000000000, -0.000000000000000000, -0.000000000000000000 ) ) ;
#34537 = CARTESIAN_POINT ( 'NONE',  ( 785.3141322388236176, -333.7255117493286320, 364.4286716492789537 ) ) ;
#34536 = CARTESIAN_POINT ( 'NONE',  ( 787.6308680596127942, -107.2601417444145824, 364.1105419155492768 ) ) ;
#34538 = EDGE_LOOP ( 'NONE', ( #19829, #3183, #5252, #40902 ) ) ;
#34539 = CARTESIAN_POINT ( 'NONE',  ( 805.1016975059191054, -246.8965053807777679, -343.0745993439771837 ) ) ;
#34540 = CARTESIAN_POINT ( 'NONE',  ( 792.1044303154645831, -84.45278447660206211, 317.8323909638837677 ) ) ;
#34541 = CARTESIAN_POINT ( 'NONE',  ( 759.8311093483677041, -262.1692326535049347, -310.9282345327691814 ) ) ;
#34542 = LINE ( 'NONE', #27844, #6152 ) ;
#34543 = CARTESIAN_POINT ( 'NONE',  ( 807.5423716828161105, -369.0783235625956422, 362.2119215644372048 ) ) ;
#34544 = EDGE_LOOP ( 'NONE', ( #23477, #40201, #41436, #43001 ) ) ;
#34545 = CARTESIAN_POINT ( 'NONE',  ( 800.0135310231082713, -278.0891481129651197, 325.0180583372163028 ) ) ;
#34546 = CONICAL_SURFACE ( 'NONE', #24211, 8.024999999999948841, 0.7853981633974337351 ) ;
#34547 = CARTESIAN_POINT ( 'NONE',  ( 756.7813123517142913, -43.98741447168752217, -329.9779781133712504 ) ) ;
#34548 = CARTESIAN_POINT ( 'NONE',  ( 785.3141322388236176, -165.7255117493291152, -364.4286716492789537 ) ) ;
#34549 = CARTESIAN_POINT ( 'NONE',  ( 767.8955696845333705, -360.4527844766010958, 362.1676090361162323 ) ) ;
#34550 = ADVANCED_FACE ( 'NONE', ( #10004 ), #16939, .T. ) ;
#34551 = CARTESIAN_POINT ( 'NONE',  ( 808.3070685750230950, -114.9982390220565236, -361.1904061080339261 ) ) ;
#34552 = CARTESIAN_POINT ( 'NONE',  ( 767.8955696845334842, -96.45278447660204790, -362.1676090361161755 ) ) ;
#34553 = ORIENTED_EDGE ( 'NONE', *, *, #33712, .F. ) ;
#34554 = CARTESIAN_POINT ( 'NONE',  ( 766.0291762391763086, -58.91815448151690759, -360.7704444035551319 ) ) ;
#34555 = CARTESIAN_POINT ( 'NONE',  ( 783.0745993439762742, -344.1908817542433212, -365.1016975059196739 ) ) ;
#34557 = CARTESIAN_POINT ( 'NONE',  ( 775.8780910478218402, -417.2817908451522158, 364.9511171171680530 ) ) ;
#34556 = CARTESIAN_POINT ( 'NONE',  ( 801.9419747391806368, -138.4527844766019200, 351.9812246680014027 ) ) ;
#34558 = CARTESIAN_POINT ( 'NONE',  ( 772.3691319403857278, -95.26014174441461080, 315.8894580844506663 ) ) ;
#34561 = CARTESIAN_POINT ( 'NONE',  ( 810.1134526219336749, -368.5328690171409676, 357.8822607201570349 ) ) ;
#34560 = DIRECTION ( 'NONE',  ( -1.000000000000000000, -0.000000000000000000, -0.000000000000000000 ) ) ;
#34559 = DIRECTION ( 'NONE',  ( 0.000000000000000000, 0.000000000000000000, 1.000000000000000000 ) ) ;
#34562 = EDGE_CURVE ( 'NONE', #14035, #14977, #44889, .T. ) ;
#34563 = CARTESIAN_POINT ( 'NONE',  ( 764.3348316497523456, -118.7146871989600072, 308.6759233522265617 ) ) ;
#34564 = CARTESIAN_POINT ( 'NONE',  ( 755.8894580844503253, -375.8272453906069472, -332.3691319403863531 ) ) ;
#34565 = CARTESIAN_POINT ( 'NONE',  ( 794.9819416627830151, -372.9982390220557704, -319.9864689768909898 ) ) ;
#34566 = CARTESIAN_POINT ( 'NONE',  ( 776.2046728542105711, -140.1908817542438896, -304.8212110874238761 ) ) ;
#34567 = CARTESIAN_POINT ( 'NONE',  ( 766.4474001241216001, 4.900027336664720679, 307.3154664389482491 ) ) ;
#34569 = DIRECTION ( 'NONE',  ( -1.000000000000000000, -0.000000000000000000, -0.000000000000000000 ) ) ;
#34568 = DIRECTION ( 'NONE',  ( -0.000000000000000000, 1.000000000000000000, -0.000000000000000000 ) ) ;
#34570 = CARTESIAN_POINT ( 'NONE',  ( 804.9511171171677688, -269.8055962898686175, -335.8780910478229202 ) ) ;
#34571 = CARTESIAN_POINT ( 'NONE',  ( 776.2046728542105711, -140.1908817542438896, -304.8212110874238761 ) ) ;
#34572 = DIRECTION ( 'NONE',  ( -1.000000000000000000, 0.000000000000000000, 0.000000000000000000 ) ) ;
#34573 = CARTESIAN_POINT ( 'NONE',  ( 311.1634899080286232, 260.0000000000000000, -199.9999999999963336 ) ) ;
#34574 = CARTESIAN_POINT ( 'NONE',  ( 772.4468031744293057, -345.8272453906069472, 363.8651313633793620 ) ) ;
#34575 = CARTESIAN_POINT ( 'NONE',  ( 814.4686193811664907, -291.2817908451525000, 346.2056067578752732 ) ) ;
#34576 = CARTESIAN_POINT ( 'NONE',  ( 811.0346526505617248, -182.6346026584199649, -323.0537975583478101 ) ) ;
#34577 = ADVANCED_FACE ( 'NONE', ( #20836 ), #24073, .T. ) ;
#34578 = DIRECTION ( 'NONE',  ( -5.551115123125783688E-16, -1.000000000000000000, 0.000000000000000000 ) ) ;
#34579 = VECTOR ( 'NONE', #39891, 1000.000000000000000 ) ;
#34580 = CARTESIAN_POINT ( 'NONE',  ( 788.6739635108323228, -127.6454272087894140, 373.9316612368139090 ) ) ;
#34581 = ADVANCED_FACE ( 'NONE', ( #20390, #34935 ), #10226, .F. ) ;
#34582 = CARTESIAN_POINT ( 'NONE',  ( 755.2512626584698410, -319.5436935675104451, -315.2512626584710915 ) ) ;
#34583 = DIRECTION ( 'NONE',  ( 0.000000000000000000, 0.000000000000000000, 1.000000000000000000 ) ) ;
#34584 = FACE_OUTER_BOUND ( 'NONE', #14913, .T. ) ;
#34585 = EDGE_CURVE ( 'NONE', #35556, #45366, #34487, .T. ) ;
#34586 = CARTESIAN_POINT ( 'NONE',  ( 756.5762568750052424, -195.1800572038744974, 348.7366044899774238 ) ) ;
#34587 = VERTEX_POINT ( 'NONE', #27327 ) ;
#34588 = CARTESIAN_POINT ( 'NONE',  ( 814.2805881961230625, -409.6454272087884760, 331.2368401574024119 ) ) ;
#34589 = CARTESIAN_POINT ( 'NONE',  ( 788.7631598425961101, -385.4419599262319593, -305.7194118038759143 ) ) ;
#34590 = CARTESIAN_POINT ( 'NONE',  ( 751.9810565676468741, -122.0891481129656171, -360.9747183278973921 ) ) ;
#34591 = CARTESIAN_POINT ( 'NONE',  ( 804.1105419155481968, -51.82724539060782121, 347.6308680596136469 ) ) ;
#34592 = CARTESIAN_POINT ( 'NONE',  ( 815.2698199232961542, -400.8164208402373561, -342.5225473063383106 ) ) ;
#34593 = DIRECTION ( 'NONE',  ( -1.000000000000000000, 0.000000000000000000, 0.000000000000000000 ) ) ;
#34594 = CARTESIAN_POINT ( 'NONE',  ( 803.2186876482843445, -439.9874144716862929, 350.0220218866286928 ) ) ;
#34595 = ORIENTED_EDGE ( 'NONE', *, *, #15946, .T. ) ;
#34596 = CARTESIAN_POINT ( 'NONE',  ( 778.7502325331095108, -168.3510508353234911, -304.6391490659818828 ) ) ;
#34597 = DIRECTION ( 'NONE',  ( 0.000000000000000000, 0.000000000000000000, 1.000000000000000000 ) ) ;
#34598 = CARTESIAN_POINT ( 'NONE',  ( 807.5423716828161105, -273.0783235625958696, 362.2119215644372048 ) ) ;
#34599 = CARTESIAN_POINT ( 'NONE',  ( 781.7834795799800531, -130.8164208402383224, 315.0636971347436202 ) ) ;
#34600 = ORIENTED_EDGE ( 'NONE', *, *, #6377, .F. ) ;
#34601 = ADVANCED_FACE ( 'NONE', ( #35166 ), #3545, .F. ) ;
#34602 = CARTESIAN_POINT ( 'NONE',  ( 767.8955696845333705, -264.4527844766016074, 362.1676090361162323 ) ) ;
#34603 = EDGE_CURVE ( 'NONE', #24990, #33757, #20160, .T. ) ;
#34604 = CARTESIAN_POINT ( 'NONE',  ( 777.4774526936600978, -10.27096629478414691, -304.7301800767027657 ) ) ;
#34605 = CARTESIAN_POINT ( 'NONE',  ( 794.9999999999993179, 205.0000000000000568, -245.0000000000000284 ) ) ;
#34606 = ORIENTED_EDGE ( 'NONE', *, *, #39356, .F. ) ;
#34607 = EDGE_LOOP ( 'NONE', ( #2710, #43820 ) ) ;
#34608 = CARTESIAN_POINT ( 'NONE',  ( 762.1177392798416577, -402.5545181178795247, -309.8865473780659272 ) ) ;
#34609 = AXIS2_PLACEMENT_3D ( 'NONE', #5995, #37425, #19637 ) ;
#34610 = CARTESIAN_POINT ( 'NONE',  ( 797.8594530101008786, -37.54369356751132614, 322.1405469898980982 ) ) ;
#34611 = CARTESIAN_POINT ( 'NONE',  ( 803.4237431249931660, -255.1800572038742700, -331.2633955100225194 ) ) ;
#34612 = EDGE_CURVE ( 'NONE', #30278, #22547, #41882, .T. ) ;
#34614 = CARTESIAN_POINT ( 'NONE',  ( 773.7943932421234194, -239.8055962898687028, 305.5313806188329409 ) ) ;
#34613 = CARTESIAN_POINT ( 'NONE',  ( 772.5602148656447525, -369.7255117493284615, 305.7998596910095443 ) ) ;
#34615 = EDGE_CURVE ( 'NONE', #8204, #27240, #41196, .T. ) ;
#34616 = CARTESIAN_POINT ( 'NONE',  ( 798.5707757039680246, -245.4636090269709143, -356.7845633553585003 ) ) ;
#34617 = CARTESIAN_POINT ( 'NONE',  ( 762.1405469898971887, -265.5436935675106156, -357.8594530101015607 ) ) ;
#34618 = CARTESIAN_POINT ( 'NONE',  ( 795.1360043628808398, -428.0891481129645513, -360.2193346964456282 ) ) ;
#34619 = CARTESIAN_POINT ( 'NONE',  ( 800.2193346964447755, -66.99823902205672255, -355.1360043628815788 ) ) ;
#34620 = CARTESIAN_POINT ( 'NONE',  ( 778.1981804954714335, -250.2709662947832783, 314.8072714833589885 ) ) ;
#34621 = ORIENTED_EDGE ( 'NONE', *, *, #32833, .T. ) ;
#34622 = CARTESIAN_POINT ( 'NONE',  ( 759.0252816721024374, -360.9982390220557704, 368.0189434323527280 ) ) ;
#34623 = DIRECTION ( 'NONE',  ( 1.000000000000000000, 0.000000000000000000, -0.000000000000000000 ) ) ;
#34624 = CARTESIAN_POINT ( 'NONE',  ( 793.5525998758768083, -55.09997266333508747, -372.6845335610516941 ) ) ;
#34625 = CARTESIAN_POINT ( 'NONE',  ( -919.9999999999993179, 219.9999999999998863, -360.0000000000000000 ) ) ;
#34626 = CARTESIAN_POINT ( 'NONE',  ( -784.4999999999993179, -365.3551492539851893, -28.13243251470704109 ) ) ;
#34627 = CARTESIAN_POINT ( 'NONE',  ( 780.5236548040995785, -212.7363362996982232, 314.9735926884559944 ) ) ;
#34628 = CARTESIAN_POINT ( 'NONE',  ( 803.4237431249931660, -135.1800572038746679, 331.2633955100225194 ) ) ;
#34629 = VERTEX_POINT ( 'NONE', #2611 ) ;
#34630 = CARTESIAN_POINT ( 'NONE',  ( 787.5531968255692163, 2.172754609392001601, -316.1348686366205811 ) ) ;
#34631 = CARTESIAN_POINT ( 'NONE',  ( 800.9747183278959710, -84.99823902205663728, -311.9810565676471583 ) ) ;
#34632 = CARTESIAN_POINT ( 'NONE',  ( 780.5290396650775619, -276.3510508353231785, 365.2837595273619513 ) ) ;
#34633 = CARTESIAN_POINT ( 'NONE',  ( 802.1676090361156639, -446.6346026584189985, -327.8955696845344505 ) ) ;
#34634 = CARTESIAN_POINT ( 'NONE',  ( 792.1044303154646968, -36.45278447660224685, -317.8323909638837677 ) ) ;
#34635 = CARTESIAN_POINT ( 'NONE',  ( 788.6739635108323228, -7.645427208789786100, 373.9316612368139090 ) ) ;
#34636 = CARTESIAN_POINT ( 'NONE',  ( 751.9810565676468741, -194.0891481129654039, -360.9747183278973921 ) ) ;
#34637 = CARTESIAN_POINT ( 'NONE',  ( 782.5225473063381969, -166.2709662947835909, 375.2698199232970637 ) ) ;
#34638 = CARTESIAN_POINT ( 'NONE',  ( 804.6798772138708955, -63.72551174932939233, 334.6312213355107019 ) ) ;
#34639 = DIRECTION ( 'NONE',  ( 1.000000000000000000, 0.000000000000000000, -0.000000000000000000 ) ) ;
#34640 = CARTESIAN_POINT ( 'NONE',  ( 190.7583438952258916, 294.6698570112193920, -274.9999999999999432 ) ) ;
#34641 = CARTESIAN_POINT ( 'NONE',  ( 783.7566961878529810, -264.8965053807776826, -305.1792804349288417 ) ) ;
#34642 = CIRCLE ( 'NONE', #44233, 10.00000000000000888 ) ;
#34643 = CARTESIAN_POINT ( 'NONE',  ( 771.3260364891663130, -403.6454272087884760, 306.0683387631859773 ) ) ;
#34644 = CARTESIAN_POINT ( 'NONE',  ( 763.2262854647970016, -272.6346026584196807, -309.2812353651462445 ) ) ;
#34645 = DIRECTION ( 'NONE',  ( 1.000000000000000000, 0.000000000000000000, 0.000000000000000000 ) ) ;
#34646 = CARTESIAN_POINT ( 'NONE',  ( 746.8695393053150156, -413.9073299311465348, 327.6429770376306010 ) ) ;
#34647 = CARTESIAN_POINT ( 'NONE',  ( 746.8695393053151292, -29.90732993114772142, 327.6429770376306578 ) ) ;
#34648 = CARTESIAN_POINT ( 'NONE',  ( 778.1981804954714335, -370.2709662947831362, -314.8072714833589885 ) ) ;
#34649 = CARTESIAN_POINT ( 'NONE',  ( 790.8726784830453198, -34.71468719896025590, 362.5472867521010585 ) ) ;
#34650 = CARTESIAN_POINT ( 'NONE',  ( 814.8230680027162407, -53.80559628986930676, -333.7305795820267917 ) ) ;
#34651 = CARTESIAN_POINT ( 'NONE',  ( 779.4709603349208464, -144.3510508353235764, -314.7162404726379918 ) ) ;
#34652 = CARTESIAN_POINT ( 'NONE',  ( 746.7653713866222915, -185.2601417444143692, 351.0478386215610271 ) ) ;
#34653 = CARTESIAN_POINT ( 'NONE',  ( 802.1676090361155502, 9.365397341579424051, 327.8955696845344505 ) ) ;
#34654 = ADVANCED_FACE ( 'NONE', ( #10451 ), #16711, .F. ) ;
#34655 = ORIENTED_EDGE ( 'NONE', *, *, #39901, .F. ) ;
#34656 = CARTESIAN_POINT ( 'NONE',  ( 771.2633955100217236, -47.90732993114767169, -363.4237431249939618 ) ) ;
#34657 = CARTESIAN_POINT ( 'NONE',  ( 780.5290396650775619, -180.3510508353234343, -365.2837595273619513 ) ) ;
#34658 = CARTESIAN_POINT ( 'NONE',  ( 771.1735550268778070, -177.1800572038744690, 316.3353852180827630 ) ) ;
#34659 = CARTESIAN_POINT ( 'NONE',  ( 798.0661480581538854, -2.532869017142183932, -309.5768839229118043 ) ) ;
#34660 = CARTESIAN_POINT ( 'NONE',  ( 791.9812246680005501, -284.6346026584196807, 361.9419747391813189 ) ) ;
#34661 = DIRECTION ( 'NONE',  ( 0.000000000000000000, 0.000000000000000000, 1.000000000000000000 ) ) ;
#34662 = ORIENTED_EDGE ( 'NONE', *, *, #22985, .T. ) ;
#34663 = CARTESIAN_POINT ( 'NONE',  ( 779.4709603349208464, -24.35105083532392811, 314.7162404726379918 ) ) ;
#34664 = CARTESIAN_POINT ( 'NONE',  ( 802.2119215644370342, -294.0090635724253048, -367.5423716828165084 ) ) ;
#34665 = ADVANCED_FACE ( 'NONE', ( #3301 ), #38190, .F. ) ;
#34666 = CARTESIAN_POINT ( 'NONE',  ( 805.0032342141413437, -253.5436935675105588, 314.9967657858572352 ) ) ;
#34667 = CARTESIAN_POINT ( 'NONE',  ( 799.2566176426618085, -336.0090635724251911, 324.0069404352559559 ) ) ;
#34668 = CARTESIAN_POINT ( 'NONE',  ( 768.8385539511368734, 24.73985825558500551, 306.4236121716840557 ) ) ;
#34669 = CARTESIAN_POINT ( 'NONE',  ( 784.1219089521767955, -165.2817908451529547, -315.0488828828318333 ) ) ;
#34670 = CARTESIAN_POINT ( 'NONE',  ( 791.9812246680005501, -164.6346026584200217, -361.9419747391813189 ) ) ;
#34671 = CARTESIAN_POINT ( 'NONE',  ( 756.3353852180820240, -317.9073299311467622, -331.1735550268787733 ) ) ;
#34672 = ORIENTED_EDGE ( 'NONE', *, *, #33498, .F. ) ;
#34673 =( BOUNDED_CURVE ( )  B_SPLINE_CURVE ( 3, ( #6911, #6221, #10155, #24231 ),
 .UNSPECIFIED., .F., .T. ) 
 B_SPLINE_CURVE_WITH_KNOTS ( ( 4, 4 ),
 ( 0.000000000000000000, 1.570796326794896558 ),
 .UNSPECIFIED. ) 
 CURVE ( )  GEOMETRIC_REPRESENTATION_ITEM ( )  RATIONAL_B_SPLINE_CURVE ( ( 1.000000000000000000, 0.8047378541243649375, 0.8047378541243649375, 1.000000000000000000 ) ) 
 REPRESENTATION_ITEM ( '' )  );
#34674 = CARTESIAN_POINT ( 'NONE',  ( 796.7845633553578182, -345.6237781080501463, 358.5707757039688204 ) ) ;
#34675 = CARTESIAN_POINT ( 'NONE',  ( -598.8365100919716042, 260.0000000000001705, -208.0249999999899160 ) ) ;
#34676 = CARTESIAN_POINT ( 'NONE',  ( 761.4292242960306112, -137.4636090269711985, 323.2154366446414429 ) ) ;
#34677 = CARTESIAN_POINT ( 'NONE',  ( 781.8018195045266339, 1.729033705215812011, 365.1927285166406705 ) ) ;
#34678 = ORIENTED_EDGE ( 'NONE', *, *, #15877, .T. ) ;
#34679 = CARTESIAN_POINT ( 'NONE',  ( 805.6418435158337843, -365.4636090269705164, -363.8556311672236916 ) ) ;
#34680 = DIRECTION ( 'NONE',  ( -0.000000000000000000, 0.000000000000000000, 1.000000000000000000 ) ) ;
#34681 = CARTESIAN_POINT ( 'NONE',  ( 804.1601925771018387, -175.4419599262325562, 346.5483106153029098 ) ) ;
#34682 = CARTESIAN_POINT ( 'NONE',  ( 756.3353852180819104, -341.9073299311465917, -331.1735550268788302 ) ) ;
#34683 = CARTESIAN_POINT ( 'NONE',  ( 879.9999999999992042, 239.9999999999998863, -224.9999999999999716 ) ) ;
#34684 = CARTESIAN_POINT ( 'NONE',  ( 786.5483106153019435, -199.6454272087891582, -364.1601925771022366 ) ) ;
#34685 = CARTESIAN_POINT ( 'NONE',  ( 808.3070685750230950, -90.99823902205663728, 361.1904061080339261 ) ) ;
#34686 = CARTESIAN_POINT ( 'NONE',  ( 808.6629988358042738, -452.9681489794447771, 336.2505073875255448 ) ) ;
#34687 = CARTESIAN_POINT ( 'NONE',  ( 745.7998596910086917, -413.3618753856920307, -332.5602148656461168 ) ) ;
#34688 = DIRECTION ( 'NONE',  ( -1.000000000000000000, -0.000000000000000000, 0.000000000000000000 ) ) ;
#34689 = CARTESIAN_POINT ( 'NONE',  ( 805.6418435158337843, -341.4636090269705733, 363.8556311672236916 ) ) ;
#34690 = DIRECTION ( 'NONE',  ( 0.000000000000000000, 0.000000000000000000, -1.000000000000000000 ) ) ;
#34691 = CARTESIAN_POINT ( 'NONE',  ( 748.9653473494363425, -290.6346026584195101, 356.9462024416521331 ) ) ;
#34692 = CARTESIAN_POINT ( 'NONE',  ( 808.3070685750230950, -42.99823902205675807, -361.1904061080339261 ) ) ;
#34693 = CARTESIAN_POINT ( 'NONE',  ( 767.8955696845333705, -240.4527844766015221, -362.1676090361162323 ) ) ;
#34694 = DIRECTION ( 'NONE',  ( 0.000000000000000000, -0.7651688349527138167, 0.6438296778008192334 ) ) ;
#34695 = CARTESIAN_POINT ( 'NONE',  ( 797.6776695296629214, -379.5436935675102745, 357.6776695296636603 ) ) ;
#34696 = CARTESIAN_POINT ( 'NONE',  ( 757.0176451133909268, -157.0999726633347962, 349.9200121543848354 ) ) ;
#34697 = CARTESIAN_POINT ( 'NONE',  ( 813.5763878283155464, -27.82724539060790292, -351.1614460488615350 ) ) ;
#34698 = CARTESIAN_POINT ( 'NONE',  ( 776.9566956441375396, -60.89650538077837894, -364.8461984189686405 ) ) ;
#34699 = CARTESIAN_POINT ( 'NONE',  ( 807.5423716828161105, -81.07832356259649487, 362.2119215644372048 ) ) ;
#34700 = CARTESIAN_POINT ( 'NONE',  ( 767.8955696845334842, -360.4527844766011526, 362.1676090361161755 ) ) ;
#34701 = DIRECTION ( 'NONE',  ( -0.000000000000000000, 1.000000000000000000, -0.000000000000000000 ) ) ;
#34702 = DIRECTION ( 'NONE',  ( -0.000000000000000000, 1.000000000000000000, -0.000000000000000000 ) ) ;
#34703 = CARTESIAN_POINT ( 'NONE',  ( 781.8018195045266339, -430.2709662947827383, 365.1927285166406705 ) ) ;
#34704 = ORIENTED_EDGE ( 'NONE', *, *, #9784, .F. ) ;
#34705 = CARTESIAN_POINT ( 'NONE',  ( 797.6776695296629214, -67.54369356751125508, -357.6776695296636603 ) ) ;
#34706 = CARTESIAN_POINT ( 'NONE',  ( 779.4709603349208464, -360.3510508353228374, -314.7162404726379918 ) ) ;
#34708 = CARTESIAN_POINT ( 'NONE',  ( 762.1405469898973024, -193.5436935675108714, 357.8594530101016176 ) ) ;
#34707 = CARTESIAN_POINT ( 'NONE',  ( 758.0580252608178853, -198.4527844766017495, 328.0187753319985404 ) ) ;
#34709 = CARTESIAN_POINT ( 'NONE',  ( 798.0661480581538854, -362.5328690171410813, -309.5768839229118043 ) ) ;
#34710 = DIRECTION ( 'NONE',  ( 1.892425610156518354E-16, 1.000000000000000000, -0.000000000000000000 ) ) ;
#34711 = VERTEX_POINT ( 'NONE', #37720 ) ;
#34712 = CARTESIAN_POINT ( 'NONE',  ( 795.1360043628807261, -380.0891481129646650, 360.2193346964456282 ) ) ;
#34713 = ORIENTED_EDGE ( 'NONE', *, *, #2708, .F. ) ;
#34714 = CARTESIAN_POINT ( 'NONE',  ( 777.4774526936600978, -226.2709662947834204, -304.7301800767027657 ) ) ;
#34715 = CARTESIAN_POINT ( 'NONE',  ( 754.9967657858570647, -145.5436935675109851, 365.0032342141425943 ) ) ;
#34716 = ORIENTED_EDGE ( 'NONE', *, *, #43588, .T. ) ;
#34717 = CARTESIAN_POINT ( 'NONE',  ( 795.1360043628808398, -212.0891481129653187, -360.2193346964456282 ) ) ;
#34718 = EDGE_LOOP ( 'NONE', ( #15617, #21967 ) ) ;
#34719 = CARTESIAN_POINT ( 'NONE',  ( 802.1676090361156639, -374.6346026584192828, -327.8955696845344505 ) ) ;
#34720 = CARTESIAN_POINT ( 'NONE',  ( 758.0580252608178853, -30.45278447660226817, -328.0187753319985404 ) ) ;
#34721 = CARTESIAN_POINT ( 'NONE',  ( 754.9735926884551418, -210.3510508353233490, 340.5236548041000333 ) ) ;
#34722 = CARTESIAN_POINT ( 'NONE',  ( -786.4999999999993179, -544.8427095258973623, -350.0000000000000000 ) ) ;
#34723 = LINE ( 'NONE', #41212, #36851 ) ;
#34724 = EDGE_LOOP ( 'NONE', ( #23633, #9773 ) ) ;
#34725 = CARTESIAN_POINT ( 'NONE',  ( 795.1360043628807261, 3.910851887033985896, -360.2193346964456282 ) ) ;
#34726 = CARTESIAN_POINT ( 'NONE',  ( 911.9999999999993179, 219.9999999999998863, 360.0000000000000000 ) ) ;
#34727 = FACE_OUTER_BOUND ( 'NONE', #16034, .T. ) ;
#34728 = ORIENTED_EDGE ( 'NONE', *, *, #20468, .T. ) ;
#34729 = CARTESIAN_POINT ( 'NONE',  ( 754.3581564841646241, -281.4636090269706870, -316.1443688327762516 ) ) ;
#34730 = CARTESIAN_POINT ( 'NONE',  ( 745.5313806188320314, -135.2817908451530116, 333.7943932421247268 ) ) ;
#34732 = CARTESIAN_POINT ( 'NONE',  ( 797.8594530101008786, -229.5436935675106440, -322.1405469898980982 ) ) ;
#34731 = CARTESIAN_POINT ( 'NONE',  ( -190.7583438952258916, 294.6698570112193920, -244.9999999999999716 ) ) ;
#34733 = CARTESIAN_POINT ( 'NONE',  ( 755.8398074228967971, -403.4419599262317888, -333.4516893846970333 ) ) ;
#34734 = DIRECTION ( 'NONE',  ( 0.000000000000000000, 0.000000000000000000, -1.000000000000000000 ) ) ;
#34735 = CARTESIAN_POINT ( 'NONE',  ( 768.0187753319979720, 15.36539734157940629, -318.0580252608186242 ) ) ;
#34736 = CARTESIAN_POINT ( 'NONE',  ( 796.9571628226829034, -95.46360902697132644, -321.2382568024804641 ) ) ;
#34737 = CARTESIAN_POINT ( 'NONE',  ( 939.9999999999993179, -600.0000000000001137, -350.0000000000000000 ) ) ;
#34738 = CARTESIAN_POINT ( 'NONE',  ( 805.9055244015594326, -3.623778108051270319, -315.8990559732753240 ) ) ;
#34739 = CARTESIAN_POINT ( 'NONE',  ( 811.0346526505617248, -278.6346026584196807, -323.0537975583478101 ) ) ;
#34740 = CYLINDRICAL_SURFACE ( 'NONE', #44552, 2.749999999999835687 ) ;
#34741 = DIRECTION ( 'NONE',  ( 1.000000000000000000, 0.000000000000000000, -0.000000000000000000 ) ) ;
#34742 = CARTESIAN_POINT ( 'NONE',  ( 755.3201227861273992, -75.72551174932937101, -345.3687786644892981 ) ) ;
#34743 = CARTESIAN_POINT ( 'NONE',  ( 791.0478386215596629, -213.8272453906073167, 306.7653713866226326 ) ) ;
#34744 = CARTESIAN_POINT ( 'NONE',  ( 758.0141637701419768, -183.0783235625961538, -367.2620300519063790 ) ) ;
#34745 = CARTESIAN_POINT ( 'NONE',  ( 782.4968714119720516, -202.8164208402380950, 305.0891759886411023 ) ) ;
#34746 = CARTESIAN_POINT ( 'NONE',  ( 792.2312462859673587, -419.9073299311465348, -307.2067596250082602 ) ) ;
#34747 = CARTESIAN_POINT ( 'NONE',  ( -468.8365100919714337, 230.0000000000001421, -202.7499999999907345 ) ) ;
#34748 = CARTESIAN_POINT ( 'NONE',  ( 804.9363028652555840, -280.2709662947833067, 338.2165204200192079 ) ) ;
#34749 = CARTESIAN_POINT ( 'NONE',  ( 773.4516893846965786, -43.64542720878966975, 315.8398074228977066 ) ) ;
#34750 = CARTESIAN_POINT ( 'NONE',  ( 757.8323909638827445, -410.6346026584191122, -352.1044303154654358 ) ) ;
#34751 = DIRECTION ( 'NONE',  ( 0.000000000000000000, 0.000000000000000000, 1.000000000000000000 ) ) ;
#34752 = CARTESIAN_POINT ( 'NONE',  ( 779.9999999999992042, 16.45630643248849267, 339.9999999999999432 ) ) ;
#34754 = CARTESIAN_POINT ( 'NONE',  ( 764.8639956371174549, -320.0891481129648355, 319.7806653035542013 ) ) ;
#34753 = CARTESIAN_POINT ( 'NONE',  ( 755.0488828828309806, -113.8055962898691149, 344.1219089521771934 ) ) ;
#34755 = ORIENTED_EDGE ( 'NONE', *, *, #31758, .F. ) ;
#34756 = CARTESIAN_POINT ( 'NONE',  ( 787.6308680596127942, -251.2601417444141134, -364.1105419155492768 ) ) ;
#34757 = CARTESIAN_POINT ( 'NONE',  ( 764.8639956371174549, -104.0891481129656881, 319.7806653035542013 ) ) ;
#34758 = CARTESIAN_POINT ( 'NONE',  ( 801.9858362298568863, -243.0783235625959833, -312.7379699480935642 ) ) ;
#34759 = DIRECTION ( 'NONE',  ( 1.000000000000000000, 0.000000000000000000, 0.000000000000000000 ) ) ;
#34760 = CARTESIAN_POINT ( 'NONE',  ( 781.2497674668890113, -420.3510508353225532, 375.3608509340180603 ) ) ;
#34761 = VERTEX_POINT ( 'NONE', #13474 ) ;
#34762 = CARTESIAN_POINT ( 'NONE',  ( 771.1735550268778070, -297.1800572038740711, 316.3353852180827630 ) ) ;
#34763 = CARTESIAN_POINT ( 'NONE',  ( 754.9735926884551418, -42.35105083532388193, -340.5236548041000333 ) ) ;
#34764 = CARTESIAN_POINT ( 'NONE',  ( 804.6798772138708955, -159.7255117493291436, -334.6312213355107019 ) ) ;
#34765 = CARTESIAN_POINT ( 'NONE',  ( 792.1044303154645831, -204.4527844766016926, -317.8323909638837677 ) ) ;
#34766 = CARTESIAN_POINT ( 'NONE',  ( 805.1927285166397041, -424.8164208402372992, 341.8018195045277707 ) ) ;
#34767 = CARTESIAN_POINT ( 'NONE',  ( 777.4774526936600978, -130.2709662947837899, -304.7301800767027657 ) ) ;
#34768 = CARTESIAN_POINT ( 'NONE',  ( 757.8323909638828582, -122.6346026584201496, -352.1044303154654358 ) ) ;
#34769 = ORIENTED_EDGE ( 'NONE', *, *, #26159, .T. ) ;
#34770 = CARTESIAN_POINT ( 'NONE',  ( 793.9708237608222134, -46.91815448151694312, -319.2295555964448681 ) ) ;
#34771 = CARTESIAN_POINT ( 'NONE',  ( 772.4468031744293057, -393.8272453906067199, -363.8651313633793620 ) ) ;
#34773 = CARTESIAN_POINT ( 'NONE',  ( 757.4527132478984868, -424.3726999360612808, 329.1273215169538844 ) ) ;
#34772 = CARTESIAN_POINT ( 'NONE',  ( 797.6776695296629214, -115.5436935675110988, 357.6776695296636603 ) ) ;
#34776 = CARTESIAN_POINT ( 'NONE',  ( 786.2056067578752163, -347.8055962898683333, 374.4686193811670023 ) ) ;
#34775 = CARTESIAN_POINT ( 'NONE',  ( 51.16348990802859475, 260.0000000000000568, -199.9999999999945146 ) ) ;
#34774 = CARTESIAN_POINT ( 'NONE',  ( 927.9999999999990905, 154.9999999999998863, 360.0000000000000000 ) ) ;
#34777 = ORIENTED_EDGE ( 'NONE', *, *, #31181, .F. ) ;
#34778 = EDGE_CURVE ( 'NONE', #23783, #33757, #27544, .T. ) ;
#34779 = CARTESIAN_POINT ( 'NONE',  ( 755.3028492785439312, -351.2817908451523294, -335.9200461376539693 ) ) ;
#34780 = CARTESIAN_POINT ( 'NONE',  ( 800.0135310231082713, -374.0891481129647786, -325.0180583372163028 ) ) ;
#34781 = CARTESIAN_POINT ( 'NONE',  ( 757.7880784355613741, -138.0090635724257311, -312.4576283171834916 ) ) ;
#34782 = CARTESIAN_POINT ( 'NONE',  ( 750.9282345327678740, -16.91815448151702839, 319.8311093483690115 ) ) ;
#34784 = DIRECTION ( 'NONE',  ( 1.000000000000000000, 0.000000000000000000, 0.000000000000000000 ) ) ;
#34783 = CARTESIAN_POINT ( 'NONE',  ( 759.9999999999992042, -462.9681489794448339, -309.9999999999998863 ) ) ;
#34785 = CARTESIAN_POINT ( 'NONE',  ( 763.2154366446407039, -285.6237781080502600, -321.4292242960311228 ) ) ;
#34786 = CARTESIAN_POINT ( 'NONE',  ( 768.0187753319979720, -440.6346026584191122, -318.0580252608186242 ) ) ;
#34787 = CARTESIAN_POINT ( 'NONE',  ( 805.6418435158337843, -149.4636090269711417, -363.8556311672236916 ) ) ;
#34788 = LINE ( 'NONE', #6622, #11638 ) ;
#34789 = FACE_OUTER_BOUND ( 'NONE', #42809, .T. ) ;
#34790 = CARTESIAN_POINT ( 'NONE',  ( 757.0176451133909268, -349.0999726633342561, 349.9200121543848354 ) ) ;
#34791 = CARTESIAN_POINT ( 'NONE',  ( 749.5768839229115201, -300.5545181178797520, 358.0661480581553064 ) ) ;
#34792 = CARTESIAN_POINT ( 'NONE',  ( 805.0032342141413437, -181.5436935675108430, -314.9967657858572352 ) ) ;
#34793 = FACE_OUTER_BOUND ( 'NONE', #22710, .T. ) ;
#34794 =( BOUNDED_CURVE ( )  B_SPLINE_CURVE ( 3, ( #9733, #23799, #6500, #20352 ),
 .UNSPECIFIED., .F., .T. ) 
 B_SPLINE_CURVE_WITH_KNOTS ( ( 4, 4 ),
 ( 4.691336726374857768, 4.712707788662813257 ),
 .UNSPECIFIED. ) 
 CURVE ( )  GEOMETRIC_REPRESENTATION_ITEM ( )  RATIONAL_B_SPLINE_CURVE ( ( 1.000000000000000000, 0.9999619401702002364, 0.9999619401702002364, 1.000000000000000000 ) ) 
 REPRESENTATION_ITEM ( '' )  );
#34795 = CARTESIAN_POINT ( 'NONE',  ( 745.7194118038753459, -109.6454272087894566, 348.7631598425976449 ) ) ;
#34796 = CARTESIAN_POINT ( 'NONE',  ( 763.0537975583475827, -288.4527844766014937, -371.0346526505627480 ) ) ;
#34797 = EDGE_CURVE ( 'NONE', #30554, #44542, #40425, .T. ) ;
#34798 = DIRECTION ( 'NONE',  ( 1.000000000000000000, 0.000000000000000000, 0.000000000000000000 ) ) ;
#34799 = LINE ( 'NONE', #17030, #18347 ) ;
#34800 = CARTESIAN_POINT ( 'NONE',  ( 794.9819416627830151, -180.9982390220563389, 319.9864689768909898 ) ) ;
#34801 = CIRCLE ( 'NONE', #4549, 2.749999999999919176 ) ;
#34802 = ORIENTED_EDGE ( 'NONE', *, *, #10942, .T. ) ;
#34803 = CARTESIAN_POINT ( 'NONE',  ( 768.9521613784389729, -441.8272453906066630, 373.2346286133773106 ) ) ;
#34804 = CARTESIAN_POINT ( 'NONE',  ( 807.5423716828161105, -369.0783235625956422, -362.2119215644372048 ) ) ;
#34805 = CARTESIAN_POINT ( 'NONE',  ( 767.7687537140311633, -119.9073299311474443, -372.7932403749916830 ) ) ;
#34806 = CARTESIAN_POINT ( 'NONE',  ( 787.5162901302840055, -371.3618753856919739, -305.4481719005792684 ) ) ;
#34808 = AXIS2_PLACEMENT_3D ( 'NONE', #27884, #2472, #38498 ) ;
#34807 = CARTESIAN_POINT ( 'NONE',  ( 831.1634899080286232, 259.9999999999998863, -208.0249999999998920 ) ) ;
#34809 = CARTESIAN_POINT ( 'NONE',  ( 761.9338519418445230, 9.467130982857780097, 370.4231160770881957 ) ) ;
#34810 = VERTEX_POINT ( 'NONE', #31479 ) ;
#34811 = EDGE_CURVE ( 'NONE', #13136, #44609, #17159, .T. ) ;
#34812 = CARTESIAN_POINT ( 'NONE',  ( 791.1614460488616487, -155.2601417444144261, -373.5763878283158874 ) ) ;
#34813 = FACE_OUTER_BOUND ( 'NONE', #22806, .T. ) ;
#34814 = CARTESIAN_POINT ( 'NONE',  ( 764.3348316497523456, -286.7146871989594388, 308.6759233522265617 ) ) ;
#34815 = CARTESIAN_POINT ( 'NONE',  ( 803.4237431249931660, -135.1800572038746679, 331.2633955100225194 ) ) ;
#34816 = VERTEX_POINT ( 'NONE', #24304 ) ;
#34817 = CARTESIAN_POINT ( 'NONE',  ( 785.3687786644884454, -299.3618753856922581, 315.3201227861279676 ) ) ;
#34818 = CARTESIAN_POINT ( 'NONE',  ( 772.4837098697144029, 0.6381246143067236254, -374.5518280994205611 ) ) ;
#34819 = CARTESIAN_POINT ( 'NONE',  ( 998.9999999999992042, -600.0000000000001137, -360.0000000000000000 ) ) ;
#34820 = EDGE_CURVE ( 'NONE', #30067, #39336, #45583, .T. ) ;
#34821 = ORIENTED_EDGE ( 'NONE', *, *, #16443, .T. ) ;
#34822 = CARTESIAN_POINT ( 'NONE',  ( 748.6759233522253680, -424.3726999360612808, -324.3348316497537098 ) ) ;
#34823 = EDGE_CURVE ( 'NONE', #3234, #14904, #41149, .T. ) ;
#34824 = CARTESIAN_POINT ( 'NONE',  ( 755.0636971347428243, -28.27096629478409540, 341.7834795799807353 ) ) ;
#34825 = CARTESIAN_POINT ( 'NONE',  ( 755.0636971347428243, -268.2709662947833067, -341.7834795799807353 ) ) ;
#34827 = CARTESIAN_POINT ( 'NONE',  ( 746.0683387631852383, -259.4419599262322436, 331.3260364891676204 ) ) ;
#34826 = CARTESIAN_POINT ( 'NONE',  ( 801.1904061080338124, -356.0891481129648355, 368.3070685750236066 ) ) ;
#34828 = CARTESIAN_POINT ( 'NONE',  ( 760.7433823573367135, -252.0090635724254184, -355.9930595647440441 ) ) ;
#34829 = CARTESIAN_POINT ( 'NONE',  ( 805.1927285166397041, -256.8164208402379245, -341.8018195045277707 ) ) ;
#34830 = AXIS2_PLACEMENT_3D ( 'NONE', #32006, #27630, #42406 ) ;
#34831 = CARTESIAN_POINT ( 'NONE',  ( 939.9999999999992042, -184.9457194955397767, -62.92409052808234549 ) ) ;
#34832 = CARTESIAN_POINT ( 'NONE',  ( 781.8018195045266339, -94.27096629478386092, -365.1927285166406705 ) ) ;
#34833 = CARTESIAN_POINT ( 'NONE',  ( 804.9363028652555840, -256.2709662947834204, 338.2165204200192079 ) ) ;
#34834 = CARTESIAN_POINT ( 'NONE',  ( 787.5162901302840055, -371.3618753856919739, 305.4481719005792684 ) ) ;
#34835 = DIRECTION ( 'NONE',  ( -0.000000000000000000, 1.000000000000000000, -0.000000000000000000 ) ) ;
#34836 = CARTESIAN_POINT ( 'NONE',  ( 795.8262568251477660, -46.37269993606239638, -308.3538107759623585 ) ) ;
#34837 = CARTESIAN_POINT ( 'NONE',  ( 999.9999999999992042, 478.9999999999999432, -359.0000000000000000 ) ) ;
#34838 = CARTESIAN_POINT ( 'NONE',  ( 831.1634899080286232, 258.0939999999998804, -206.1189999999999429 ) ) ;
#34839 = CARTESIAN_POINT ( 'NONE',  ( 804.8461984189677878, -218.1908817542437191, 336.9566956441385628 ) ) ;
#34840 = CARTESIAN_POINT ( 'NONE',  ( 800.0135310231082713, -134.0891481129655745, 325.0180583372163028 ) ) ;
#34841 = EDGE_LOOP ( 'NONE', ( #27334, #8424, #36976, #43072 ) ) ;
#34842 = CARTESIAN_POINT ( 'NONE',  ( 773.4516893846965786, 4.354572791210176597, -315.8398074228977066 ) ) ;
#34843 = CARTESIAN_POINT ( 'NONE',  ( 814.9108240113580450, -64.27096629478397460, -337.5031285880265273 ) ) ;
#34844 = CARTESIAN_POINT ( 'NONE',  ( 794.1144889064781864, -298.1692326535049347, 360.9840315886528401 ) ) ;
#34845 = CARTESIAN_POINT ( 'NONE',  ( 755.0636971347428243, -436.2709662947827951, -341.7834795799807353 ) ) ;
#34846 = ADVANCED_FACE ( 'NONE', ( #31696 ), #8712, .F. ) ;
#34847 = CARTESIAN_POINT ( 'NONE',  ( 754.3581564841646241, 6.536390973028352924, 316.1443688327762516 ) ) ;
#34848 = CARTESIAN_POINT ( 'NONE',  ( 787.4397851343537695, -189.7255117493290300, -374.2001403089903988 ) ) ;
#34849 = EDGE_CURVE ( 'NONE', #15138, #12788, #23416, .T. ) ;
#34850 = CARTESIAN_POINT ( 'NONE',  ( 808.0189434323515343, -182.0891481129654323, 319.0252816721025511 ) ) ;
#34851 = CARTESIAN_POINT ( 'NONE',  ( 791.9812246680005501, -92.63460265842026331, 361.9419747391813189 ) ) ;
#34852 = AXIS2_PLACEMENT_3D ( 'NONE', #17990, #4804, #18672 ) ;
#34853 = LINE ( 'NONE', #3216, #35822 ) ;
#34854 = DIRECTION ( 'NONE',  ( 0.000000000000000000, 0.000000000000000000, -1.000000000000000000 ) ) ;
#34855 = CARTESIAN_POINT ( 'NONE',  ( 758.0141637701419768, -255.0783235625958980, -367.2620300519063790 ) ) ;
#34856 = CARTESIAN_POINT ( 'NONE',  ( 757.7880784355613741, -426.0090635724247932, 312.4576283171834916 ) ) ;
#34857 = CARTESIAN_POINT ( 'NONE',  ( 782.4968714119720516, -274.8164208402378108, -305.0891759886411023 ) ) ;
#34858 = CARTESIAN_POINT ( 'NONE',  ( 200.7583438952257211, -1.114432678890474281E-13, -244.9999999999999716 ) ) ;
#34859 = CARTESIAN_POINT ( 'NONE',  ( 803.8651313633788504, -365.2601417444137155, 332.4468031744301015 ) ) ;
#34860 = CARTESIAN_POINT ( 'NONE',  ( 751.6929314249750860, -54.99823902205672965, 318.8095938919659034 ) ) ;
#34861 = EDGE_CURVE ( 'NONE', #10866, #15586, #8148, .T. ) ;
#34862 = CARTESIAN_POINT ( 'NONE',  ( 801.9858362298568863, -27.07832356259665474, -312.7379699480935642 ) ) ;
#34863 = CARTESIAN_POINT ( 'NONE',  ( 781.7834795799800531, -394.8164208402374697, -315.0636971347436202 ) ) ;
#34864 = EDGE_CURVE ( 'NONE', #28618, #21201, #965, .T. ) ;
#34865 = CARTESIAN_POINT ( 'NONE',  ( 790.8726784830453198, -10.71468719896033761, 362.5472867521010585 ) ) ;
#34866 = CARTESIAN_POINT ( 'NONE',  ( 791.1614460488616487, -59.26014174441473870, -373.5763878283158874 ) ) ;
#34867 = CARTESIAN_POINT ( 'NONE',  ( 755.8398074228967971, -187.4419599262325278, -333.4516893846970333 ) ) ;
#34868 = CARTESIAN_POINT ( 'NONE',  ( 773.7943932421234194, -167.8055962898689586, 305.5313806188329409 ) ) ;
#34869 = CARTESIAN_POINT ( 'NONE',  ( 771.1735550268780344, -9.180057203875058747, 316.3353852180828198 ) ) ;
#34870 = VERTEX_POINT ( 'NONE', #18081 ) ;
#34871 = CARTESIAN_POINT ( 'NONE',  ( 756.5762568750052424, -51.18005720387493085, -348.7366044899774238 ) ) ;
#34872 = CARTESIAN_POINT ( 'NONE',  ( 786.6156483768007774, -217.4419599262324141, -315.5913626894246136 ) ) ;
#34873 = UNCERTAINTY_MEASURE_WITH_UNIT (LENGTH_MEASURE( 1.000000000000000082E-05 ), #11832, 'distance_accuracy_value', 'NONE');
#34874 = CARTESIAN_POINT ( 'NONE',  ( 800.0135310231082713, -182.0891481129654323, 325.0180583372163028 ) ) ;
#34875 = CARTESIAN_POINT ( 'NONE',  ( 808.7758568127978833, -4.169232653505813069, -320.0363995740631822 ) ) ;
#34876 = CARTESIAN_POINT ( 'NONE',  ( 756.5762568750052424, -339.1800572038740142, 348.7366044899774238 ) ) ;
#34877 = CARTESIAN_POINT ( 'NONE',  ( 914.9999999999992042, 99.99999999999984368, -360.0000000000000000 ) ) ;
#34878 = ORIENTED_EDGE ( 'NONE', *, *, #28677, .T. ) ;
#34879 = CARTESIAN_POINT ( 'NONE',  ( 805.1016975059191054, -30.89650538077846065, 343.0745993439771837 ) ) ;
#34880 = CARTESIAN_POINT ( 'NONE',  ( 752.7379699480933368, -300.0090635724252479, -361.9858362298580232 ) ) ;
#34881 = EDGE_CURVE ( 'NONE', #27295, #31800, #45571, .T. ) ;
#34882 = CARTESIAN_POINT ( 'NONE',  ( 751.6929314249750860, -270.9982390220561115, 318.8095938919659034 ) ) ;
#34883 = CARTESIAN_POINT ( 'NONE',  ( 760.7433823573367135, -348.0090635724251342, 355.9930595647440441 ) ) ;
#34884 = CARTESIAN_POINT ( 'NONE',  ( 804.9511171171677688, -437.8055962898679923, 335.8780910478229202 ) ) ;
#34885 = CARTESIAN_POINT ( 'NONE',  ( 796.9571628226829034, -143.4636090269711701, -321.2382568024804641 ) ) ;
#34886 = CARTESIAN_POINT ( 'NONE',  ( 797.6776695296629214, -139.5436935675110135, -357.6776695296636603 ) ) ;
#34887 = AXIS2_PLACEMENT_3D ( 'NONE', #21620, #14240, #21171 ) ;
#34888 = CARTESIAN_POINT ( 'NONE',  ( 794.9819416627830151, -324.9982390220559409, -319.9864689768909898 ) ) ;
#34889 = ORIENTED_EDGE ( 'NONE', *, *, #34778, .T. ) ;
#34890 = CARTESIAN_POINT ( 'NONE',  ( 746.8695393053150156, -269.9073299311468190, 327.6429770376306010 ) ) ;
#34891 = CARTESIAN_POINT ( 'NONE',  ( 758.6633372737375112, -332.5328690171411381, 326.9102291470432533 ) ) ;
#34892 = PLANE ( 'NONE',  #21164 ) ;
#34893 = CARTESIAN_POINT ( 'NONE',  ( 755.1538015810308480, -110.1908817542440033, 343.0433043558613804 ) ) ;
#34894 = CARTESIAN_POINT ( 'NONE',  ( 801.9419747391806368, -18.45278447660230725, 351.9812246680014027 ) ) ;
#34895 = ORIENTED_EDGE ( 'NONE', *, *, #37612, .T. ) ;
#34896 = CARTESIAN_POINT ( 'NONE',  ( 748.6759233522253680, -376.3726999360614514, -324.3348316497537098 ) ) ;
#34897 = LINE ( 'NONE', #17356, #23949 ) ;
#34898 = CARTESIAN_POINT ( 'NONE',  ( 745.5313806188320314, -231.2817908451527558, 333.7943932421247268 ) ) ;
#34899 = CARTESIAN_POINT ( 'NONE',  ( 794.1144889064781864, -202.1692326535051905, 360.9840315886528401 ) ) ;
#34900 = CARTESIAN_POINT ( 'NONE',  ( 758.0580252608178853, -318.4527844766014368, -328.0187753319985404 ) ) ;
#34901 = AXIS2_PLACEMENT_3D ( 'NONE', #44716, #13077, #28060 ) ;
#34902 = ADVANCED_FACE ( 'NONE', ( #3984 ), #39573, .F. ) ;
#34903 = CARTESIAN_POINT ( 'NONE',  ( -66.63011601220125613, -365.3551492539851893, -8.132432514707076621 ) ) ;
#34904 = CARTESIAN_POINT ( 'NONE',  ( 802.9823548866075953, -217.0999726633345972, -330.0799878456151077 ) ) ;
#34905 = ADVANCED_FACE ( 'NONE', ( #22211 ), #32161, .F. ) ;
#34906 = CARTESIAN_POINT ( 'NONE',  ( 782.5225473063381969, 1.729033705215812011, 375.2698199232970637 ) ) ;
#34907 = CARTESIAN_POINT ( 'NONE',  ( 763.0537975583475827, -72.45278447660213317, 371.0346526505627480 ) ) ;
#34908 = CARTESIAN_POINT ( 'NONE',  ( 808.4681505782122031, -452.9681489794450613, 336.7690310503822388 ) ) ;
#34909 = CARTESIAN_POINT ( 'NONE',  ( 747.2067596250078623, -411.1800572038738437, -352.2312462859687230 ) ) ;
#34910 = CARTESIAN_POINT ( 'NONE',  ( 999.9999999999992042, 478.9999999999999432, 199.9999999999999716 ) ) ;
#34911 = CARTESIAN_POINT ( 'NONE',  ( 760.0363995740630116, -346.9181544815160123, 368.7758568127991907 ) ) ;
#34912 = DIRECTION ( 'NONE',  ( -1.000000000000000000, -0.000000000000000000, -0.000000000000000000 ) ) ;
#34913 = CARTESIAN_POINT ( 'NONE',  ( 787.4397851343537695, -285.7255117493286889, 374.2001403089903988 ) ) ;
#34914 = CARTESIAN_POINT ( 'NONE',  ( 772.4837098697144029, -71.36187538569302546, -374.5518280994205611 ) ) ;
#34915 = CARTESIAN_POINT ( 'NONE',  ( 759.9864689768902508, -290.0891481129650629, -354.9819416627836404 ) ) ;
#34916 = FACE_BOUND ( 'NONE', #3035, .T. ) ;
#34917 = APPLICATION_CONTEXT ( 'automotive_design' ) ;
#34918 = CARTESIAN_POINT ( 'NONE',  ( 755.3201227861273992, -411.7255117493282910, 345.3687786644892981 ) ) ;
#34919 = CIRCLE ( 'NONE', #15020, 2.749999999999835687 ) ;
#34920 = CARTESIAN_POINT ( 'NONE',  ( 763.8424801807145741, -162.0090635724256742, 320.5453621957614700 ) ) ;
#34921 = CARTESIAN_POINT ( 'NONE',  ( 814.8207195650702488, -26.19088175424427334, -336.2433038121456548 ) ) ;
#34922 = CARTESIAN_POINT ( 'NONE',  ( 795.9930595647434757, -75.07832356259649487, -320.7433823573372820 ) ) ;
#34923 = CARTESIAN_POINT ( 'NONE',  ( 800.1688906516307043, -82.16923265350558836, 369.0717654672308186 ) ) ;
#34924 = CARTESIAN_POINT ( 'NONE',  ( 797.8594530101009923, -397.5436935675101040, 322.1405469898982119 ) ) ;
#34925 = AXIS2_PLACEMENT_3D ( 'NONE', #31657, #39532, #21964 ) ;
#34926 = LINE ( 'NONE', #34226, #24712 ) ;
#34927 = CARTESIAN_POINT ( 'NONE',  ( 797.6776695296629214, -427.5436935675101040, 357.6776695296636603 ) ) ;
#34928 = ORIENTED_EDGE ( 'NONE', *, *, #18974, .T. ) ;
#34929 = CARTESIAN_POINT ( 'NONE',  ( 755.0636971347428243, -52.27096629478401724, -341.7834795799807353 ) ) ;
#34930 = CARTESIAN_POINT ( 'NONE',  ( 798.7617431975189675, -363.6237781080502032, -323.0428371773161871 ) ) ;
#34932 = CARTESIAN_POINT ( 'NONE',  ( 764.8639956371174549, -200.0891481129653471, 319.7806653035542581 ) ) ;
#34931 = CARTESIAN_POINT ( 'NONE',  ( 792.1044303154645831, -228.4527844766015789, 317.8323909638837677 ) ) ;
#34933 = EDGE_LOOP ( 'NONE', ( #37714, #12654, #31365, #25821 ) ) ;
#34934 = CARTESIAN_POINT ( 'NONE',  ( 764.3348316497523456, -382.7146871989591546, -308.6759233522265617 ) ) ;
#34935 = FACE_BOUND ( 'NONE', #30238, .T. ) ;
#34936 = EDGE_LOOP ( 'NONE', ( #17654, #16772, #15366, #9899 ) ) ;
#34937 = CARTESIAN_POINT ( 'NONE',  ( 805.1927285166397041, -376.8164208402375834, 341.8018195045277707 ) ) ;
#34938 = VECTOR ( 'NONE', #24328, 1000.000000000000000 ) ;
#34939 = VERTEX_POINT ( 'NONE', #14632 ) ;
#34940 = CARTESIAN_POINT ( 'NONE',  ( 811.0346526505616112, -254.6346026584196238, -323.0537975583477532 ) ) ;
#34941 = CARTESIAN_POINT ( 'NONE',  ( 749.2812353651451076, -150.4527844766018916, 323.2262854647983090 ) ) ;
#34942 = VERTEX_POINT ( 'NONE', #526 ) ;
#34943 = CARTESIAN_POINT ( 'NONE',  ( 774.6312213355098493, -215.3618753856925707, -364.6798772138717482 ) ) ;
#34944 = ORIENTED_EDGE ( 'NONE', *, *, #1890, .F. ) ;
#34945 = CARTESIAN_POINT ( 'NONE',  ( 759.7806653035534055, -366.9982390220556567, -324.8639956371180801 ) ) ;
#34946 = CARTESIAN_POINT ( 'NONE',  ( 803.6646147819161570, -17.90732993114776406, -348.8264449731210561 ) ) ;
#34947 = CARTESIAN_POINT ( 'NONE',  ( 795.9930595647434757, -219.0783235625960401, 320.7433823573372820 ) ) ;
#34948 = DIRECTION ( 'NONE',  ( -0.000000000000000000, 1.000000000000000000, -0.000000000000000000 ) ) ;
#34949 = DIRECTION ( 'NONE',  ( 0.000000000000000000, 0.000000000000000000, 1.000000000000000000 ) ) ;
#34950 = VERTEX_POINT ( 'NONE', #35387 ) ;
#34951 = CARTESIAN_POINT ( 'NONE',  ( 802.5472867521000353, -460.3726999360611103, -350.8726784830461156 ) ) ;
#34952 = CARTESIAN_POINT ( 'NONE',  ( -786.4999999999993179, 323.4107432173689176, 352.9408934102648345 ) ) ;
#34953 = CARTESIAN_POINT ( 'NONE',  ( 787.4999999999992042, -462.9681489794447202, -270.0000000000000568 ) ) ;
#34954 = VECTOR ( 'NONE', #1504, 1000.000000000000000 ) ;
#34955 = ORIENTED_EDGE ( 'NONE', *, *, #8497, .F. ) ;
#34956 = CARTESIAN_POINT ( 'NONE',  ( 766.4474001241216001, -259.0999726633343698, -307.3154664389482491 ) ) ;
#34957 = CARTESIAN_POINT ( 'NONE',  ( 778.7629533639073998, -128.7363362996984790, 375.0009284576466371 ) ) ;
#34959 = CARTESIAN_POINT ( 'NONE',  ( 800.0135310231082713, -206.0891481129653471, -325.0180583372163028 ) ) ;
#34958 = DIRECTION ( 'NONE',  ( -0.000000000000000000, -0.6438296778008192334, -0.7651688349527135946 ) ) ;
#34960 = CARTESIAN_POINT ( 'NONE',  ( 796.7845633553578182, -393.6237781080500326, -358.5707757039688204 ) ) ;
#34961 = CARTESIAN_POINT ( 'NONE',  ( -598.8365100919716042, 260.0000000000001705, -191.9749999999900183 ) ) ;
#34962 = DIRECTION ( 'NONE',  ( 0.000000000000000000, 0.000000000000000000, -1.000000000000000000 ) ) ;
#34963 = CARTESIAN_POINT ( 'NONE',  ( 761.4292242960306112, -113.4636090269712554, -323.2154366446414429 ) ) ;
#34964 = CARTESIAN_POINT ( 'NONE',  ( 786.2694204179717872, -381.2817908451523294, 305.1769319972829067 ) ) ;
#34965 = LINE ( 'NONE', #20645, #29950 ) ;
#34966 = CARTESIAN_POINT ( 'NONE',  ( 791.1614460488616487, 12.73985825558503926, -373.5763878283158874 ) ) ;
#34967 = CARTESIAN_POINT ( 'NONE',  ( 811.0346526505617248, -302.6346026584195670, -323.0537975583478101 ) ) ;
#34968 = CARTESIAN_POINT ( 'NONE',  ( 949.5497976682736407, 120.6654763175833693, -209.9999999999999716 ) ) ;
#34969 = DIRECTION ( 'NONE',  ( 1.000000000000000000, -0.000000000000000000, -0.000000000000000000 ) ) ;
#34970 = CARTESIAN_POINT ( 'NONE',  ( 781.7834795799800531, -82.81642084023846451, -315.0636971347436202 ) ) ;
#34971 = CARTESIAN_POINT ( 'NONE',  ( 793.5525998758768083, -247.0999726633344835, 372.6845335610516941 ) ) ;
#34972 = CARTESIAN_POINT ( 'NONE',  ( 783.7566961878529810, -216.8965053807778816, -305.1792804349288417 ) ) ;
#34973 = CARTESIAN_POINT ( 'NONE',  ( 748.9653473494363425, -194.6346026584198796, 356.9462024416521331 ) ) ;
#34974 = CARTESIAN_POINT ( 'NONE',  ( 747.2067596250078623, -435.1800572038737869, -352.2312462859687230 ) ) ;
#34975 = DIRECTION ( 'NONE',  ( 0.000000000000000000, 0.000000000000000000, 1.000000000000000000 ) ) ;
#34976 = CARTESIAN_POINT ( 'NONE',  ( 802.1676090361156639, -278.6346026584196807, 327.8955696845344505 ) ) ;
#34977 = CARTESIAN_POINT ( 'NONE',  ( 773.4516893846965786, -91.64542720878951343, 315.8398074228977066 ) ) ;
#34978 = DIRECTION ( 'NONE',  ( -1.000000000000000000, 0.000000000000000000, 0.000000000000000000 ) ) ;
#34979 = CARTESIAN_POINT ( 'NONE',  ( 879.9999999999992042, 99.99999999999984368, 360.0000000000000000 ) ) ;
#34981 = CARTESIAN_POINT ( 'NONE',  ( 756.5762568750052424, -315.1800572038740711, 348.7366044899774238 ) ) ;
#34980 = CARTESIAN_POINT ( 'NONE',  ( 805.1016975059191054, -126.8965053807781516, 343.0745993439771837 ) ) ;
#34982 = ORIENTED_EDGE ( 'NONE', *, *, #24620, .F. ) ;
#34983 = VECTOR ( 'NONE', #8382, 1000.000000000000000 ) ;
#34984 = CARTESIAN_POINT ( 'NONE',  ( 800.7704444035546203, -268.1692326535049347, -326.0291762391768771 ) ) ;
#34985 = AXIS2_PLACEMENT_3D ( 'NONE', #19256, #37262, #2616 ) ;
#34986 = CARTESIAN_POINT ( 'NONE',  ( 802.1676090361156639, -86.63460265842023489, 327.8955696845344505 ) ) ;
#34987 = MECHANICAL_DESIGN_GEOMETRIC_PRESENTATION_REPRESENTATION (  '', ( #28356 ), #35718 ) ;
#34988 = CARTESIAN_POINT ( 'NONE',  ( 761.9338519418445230, -278.5328690171412518, -370.4231160770881957 ) ) ;
#34989 = DIRECTION ( 'NONE',  ( 1.000000000000000000, 0.000000000000000000, -0.000000000000000000 ) ) ;
#34990 = CARTESIAN_POINT ( 'NONE',  ( 748.3538107759620743, -424.7146871989589840, 355.8262568251490165 ) ) ;
#34991 = EDGE_LOOP ( 'NONE', ( #30655, #36824, #44655, #36727 ) ) ;
#34992 = CARTESIAN_POINT ( 'NONE',  ( 764.8639956371174549, -296.0891481129650629, 319.7806653035542013 ) ) ;
#34993 = CARTESIAN_POINT ( 'NONE',  ( 765.8855110935204493, -46.16923265350568784, -319.0159684113471599 ) ) ;
#34994 = CARTESIAN_POINT ( 'NONE',  ( 768.0187753319979720, -176.6346026584199933, -318.0580252608186242 ) ) ;
#34995 = CARTESIAN_POINT ( 'NONE',  ( 762.3223304703356007, -199.5436935675108430, -322.3223304703362828 ) ) ;
#34996 = CARTESIAN_POINT ( 'NONE',  ( 788.7366044899766848, -395.9073299311465348, 316.5762568750059813 ) ) ;
#34997 = CARTESIAN_POINT ( 'NONE',  ( 782.4968714119720516, -106.8164208402383935, -305.0891759886411023 ) ) ;
#34998 = CARTESIAN_POINT ( 'NONE',  ( 781.7834795799800531, -106.8164208402383935, -315.0636971347436202 ) ) ;
#34999 = ORIENTED_EDGE ( 'NONE', *, *, #39673, .F. ) ;
#35000 = CARTESIAN_POINT ( 'NONE',  ( 757.4527132478984868, -400.3726999360612808, -329.1273215169538844 ) ) ;
#35001 = VECTOR ( 'NONE', #44786, 1000.000000000000000 ) ;
#35002 = CARTESIAN_POINT ( 'NONE',  ( 796.1575198192839480, -438.0090635724247932, 359.4546378042384163 ) ) ;
#35003 = CARTESIAN_POINT ( 'NONE',  ( 803.2186876482843445, -127.9874144716872308, 350.0220218866286928 ) ) ;
#35006 = CARTESIAN_POINT ( 'NONE',  ( 808.7758568127978833, -364.1692326535046504, 320.0363995740631822 ) ) ;
#35005 = DIRECTION ( 'NONE',  ( -0.000000000000000000, -0.000000000000000000, 1.000000000000000000 ) ) ;
#35004 = DIRECTION ( 'NONE',  ( 0.000000000000000000, 0.3826834323650836756, 0.9238795325112892920 ) ) ;
#35007 = AXIS2_PLACEMENT_3D ( 'NONE', #3586, #10491, #35211 ) ;
#35008 = ORIENTED_EDGE ( 'NONE', *, *, #33417, .F. ) ;
#35009 = CARTESIAN_POINT ( 'NONE',  ( 761.4292242960306112, -353.4636090269705733, -323.2154366446414429 ) ) ;
#35010 = CARTESIAN_POINT ( 'NONE',  ( 758.0580252608178853, -342.4527844766013231, -328.0187753319985404 ) ) ;
#35011 = CARTESIAN_POINT ( 'NONE',  ( 776.2046728542105711, -164.1908817542438612, -304.8212110874238761 ) ) ;
#35012 = CARTESIAN_POINT ( 'NONE',  ( 809.0717654672305343, -28.91815448151699286, 360.1688906516309885 ) ) ;
#35014 = CARTESIAN_POINT ( 'NONE',  ( -728.8365100919714905, 260.0000000000001705, -191.9749999999891372 ) ) ;
#35013 = LINE ( 'NONE', #42402, #19675 ) ;
#35015 = CARTESIAN_POINT ( 'NONE',  ( 760.5453621957607311, -285.0783235625958127, -323.8424801807151425 ) ) ;
#35016 = LINE ( 'NONE', #35470, #10709 ) ;
#35017 = CARTESIAN_POINT ( 'NONE',  ( 791.0478386215596629, -141.8272453906075157, -306.7653713866226326 ) ) ;
#35018 = DIRECTION ( 'NONE',  ( 0.000000000000000000, 1.000000000000000000, 0.000000000000000000 ) ) ;
#35019 = CYLINDRICAL_SURFACE ( 'NONE', #35609, 10.00000000000000888 ) ;
#35020 = CARTESIAN_POINT ( 'NONE',  ( 793.9708237608222134, -382.9181544815159555, 319.2295555964448681 ) ) ;
#35021 = CARTESIAN_POINT ( 'NONE',  ( 781.2370466360911223, -332.7363362996979390, 304.9990715423533629 ) ) ;
#35022 = EDGE_CURVE ( 'NONE', #27330, #9635, #24769, .T. ) ;
#35023 = CARTESIAN_POINT ( 'NONE',  ( 751.6929314249750860, -222.9982390220561683, -318.8095938919659034 ) ) ;
#35024 = CARTESIAN_POINT ( 'NONE',  ( 799.9999999999993179, 205.0000000000000568, 360.0000000000000000 ) ) ;
#35025 = AXIS2_PLACEMENT_3D ( 'NONE', #9298, #23367, #37469 ) ;
#35026 = CARTESIAN_POINT ( 'NONE',  ( 773.7305795820266212, -153.2817908451529831, 374.8230680027170365 ) ) ;
#35027 = CARTESIAN_POINT ( 'NONE',  ( 749.2812353651451076, -342.4527844766013231, -323.2262854647983090 ) ) ;
#35028 = CARTESIAN_POINT ( 'NONE',  ( 769.9999999999992042, 205.0000000000000568, -319.9999999999999432 ) ) ;
#35029 = CYLINDRICAL_SURFACE ( 'NONE', #19054, 9.999999999999980460 ) ;
#35030 = CARTESIAN_POINT ( 'NONE',  ( 791.9812246680005501, -188.6346026584199365, 361.9419747391813189 ) ) ;
#35031 = VERTEX_POINT ( 'NONE', #39800 ) ;
#35032 = CARTESIAN_POINT ( 'NONE',  ( 745.7194118038753459, -421.6454272087885329, 348.7631598425976449 ) ) ;
#35033 = CARTESIAN_POINT ( 'NONE',  ( 808.7758568127978833, -388.1692326535045936, -320.0363995740631822 ) ) ;
#35034 = CARTESIAN_POINT ( 'NONE',  ( 811.0346526505616112, -110.6346026584201638, -323.0537975583477532 ) ) ;
#35035 = CIRCLE ( 'NONE', #16587, 19.99999999999990763 ) ;
#35036 = CARTESIAN_POINT ( 'NONE',  ( 755.2512626584698410, -415.5436935675102177, -315.2512626584710915 ) ) ;
#35037 = DIRECTION ( 'NONE',  ( 0.000000000000000000, 0.000000000000000000, -1.000000000000000000 ) ) ;
#35038 = CARTESIAN_POINT ( 'NONE',  ( 811.6461892240364477, 19.28531280103956647, 324.1737431748509835 ) ) ;
#35039 = EDGE_LOOP ( 'NONE', ( #15240, #42572, #16362, #45658 ) ) ;
#35040 = AXIS2_PLACEMENT_3D ( 'NONE', #17673, #24566, #31735 ) ;
#35041 = CARTESIAN_POINT ( 'NONE',  ( 746.0683387631852383, -163.4419599262325846, -331.3260364891676204 ) ) ;
#35042 = PLANE ( 'NONE',  #37137 ) ;
#35043 = CARTESIAN_POINT ( 'NONE',  ( 746.0683387631852383, -307.4419599262320730, 331.3260364891676204 ) ) ;
#35044 = CARTESIAN_POINT ( 'NONE',  ( 797.6776695296629214, -115.5436935675110988, 357.6776695296636603 ) ) ;
#35045 = ORIENTED_EDGE ( 'NONE', *, *, #1009, .F. ) ;
#35046 = CARTESIAN_POINT ( 'NONE',  ( 771.2633955100217236, -143.9073299311473590, -363.4237431249939618 ) ) ;
#35047 = CARTESIAN_POINT ( 'NONE',  ( 767.8955696845333705, -288.4527844766014937, 362.1676090361162323 ) ) ;
#35048 = CIRCLE ( 'NONE', #28390, 20.00000000000004619 ) ;
#35049 = CARTESIAN_POINT ( 'NONE',  ( 754.9967657858570647, -25.54369356751136877, -365.0032342141425374 ) ) ;
#35050 = CARTESIAN_POINT ( 'NONE',  ( 793.3174859505621725, -452.3943253718131245, 372.3673656294391776 ) ) ;
#35051 = AXIS2_PLACEMENT_3D ( 'NONE', #29815, #43895, #8807 ) ;
#35052 = EDGE_LOOP ( 'NONE', ( #10005, #20616, #35180, #8036, #39735, #29713, #22221, #34316 ) ) ;
#35053 = CARTESIAN_POINT ( 'NONE',  ( 814.2805881961230625, -409.6454272087884760, -331.2368401574024119 ) ) ;
#35054 = VECTOR ( 'NONE', #20760, 1000.000000000000000 ) ;
#35055 = VERTEX_POINT ( 'NONE', #28227 ) ;
#35056 = CARTESIAN_POINT ( 'NONE',  ( 805.1927285166397041, -256.8164208402379245, -341.8018195045277707 ) ) ;
#35058 = CARTESIAN_POINT ( 'NONE',  ( 793.4146539503750546, -265.9874144716867477, 307.6481478633938877 ) ) ;
#35057 = CARTESIAN_POINT ( 'NONE',  ( 792.2312462859673587, -347.9073299311467053, 307.2067596250082602 ) ) ;
#35059 = CARTESIAN_POINT ( 'NONE',  ( 812.6845335610512393, -79.98741447168740137, 353.5525998758768651 ) ) ;
#35060 = CARTESIAN_POINT ( 'NONE',  ( 755.1538015810308480, -254.1908817542435770, -343.0433043558613804 ) ) ;
#35061 = CARTESIAN_POINT ( 'NONE',  ( 791.9812246680005501, -236.6346026584198228, -361.9419747391813189 ) ) ;
#35062 = CARTESIAN_POINT ( 'NONE',  ( 755.5713283507202505, -437.3618753856919170, -334.6858677611754729 ) ) ;
#35063 = CARTESIAN_POINT ( 'NONE',  ( 755.5713283507202505, -125.3618753856928834, -334.6858677611754729 ) ) ;
#35064 = EDGE_CURVE ( 'NONE', #30163, #17451, #3760, .T. ) ;
#35065 = CARTESIAN_POINT ( 'NONE',  ( 785.3141322388236176, -237.7255117493289163, 364.4286716492789537 ) ) ;
#35066 = VECTOR ( 'NONE', #3592, 1000.000000000000000 ) ;
#35067 = DIRECTION ( 'NONE',  ( -0.000000000000000000, 1.000000000000000000, -0.000000000000000000 ) ) ;
#35068 = CARTESIAN_POINT ( 'NONE',  ( 778.7629533639073998, -32.73633629969879877, -375.0009284576466371 ) ) ;
#35069 = DIRECTION ( 'NONE',  ( 0.000000000000000000, 0.7517448203044204691, -0.6594541114781790059 ) ) ;
#35070 = DIRECTION ( 'NONE',  ( -0.000000000000000000, -0.6755902076156505842, -0.7372773368101328550 ) ) ;
#35071 = ADVANCED_FACE ( 'NONE', ( #42321 ), #28704, .F. ) ;
#35072 = VECTOR ( 'NONE', #43722, 1000.000000000000000 ) ;
#35073 = CARTESIAN_POINT ( 'NONE',  ( 783.0745993439762742, -248.1908817542435202, 365.1016975059196739 ) ) ;
#35074 = CARTESIAN_POINT ( 'NONE',  ( 762.1405469898971887, -121.5436935675110419, 357.8594530101015607 ) ) ;
#35075 = VERTEX_POINT ( 'NONE', #38885 ) ;
#35076 = CARTESIAN_POINT ( 'NONE',  ( 763.8424801807145741, -18.00906357242611477, -320.5453621957614700 ) ) ;
#35077 = CARTESIAN_POINT ( 'NONE',  ( 745.4481719005789273, -75.72551174932938522, -347.5162901302853697 ) ) ;
#35078 = CARTESIAN_POINT ( 'NONE',  ( 780.5290396650775619, -300.3510508353230080, 365.2837595273619513 ) ) ;
#35079 = DIRECTION ( 'NONE',  ( 0.000000000000000000, -0.000000000000000000, 1.000000000000000000 ) ) ;
#35080 = CARTESIAN_POINT ( 'NONE',  ( 745.7194118038753459, -13.64542720878976390, 348.7631598425976449 ) ) ;
#35081 = CARTESIAN_POINT ( 'NONE',  ( 815.2698199232961542, -184.8164208402380950, -342.5225473063383106 ) ) ;
#35082 = CARTESIAN_POINT ( 'NONE',  ( 754.9967657858570647, -169.5436935675108430, 365.0032342141425374 ) ) ;
#35083 = CARTESIAN_POINT ( 'NONE',  ( 797.6776695296629214, -67.54369356751125508, 357.6776695296636603 ) ) ;
#35084 = AXIS2_PLACEMENT_3D ( 'NONE', #10026, #41438, #24092 ) ;
#35085 = DIRECTION ( 'NONE',  ( -0.000000000000000000, -0.000000000000000000, 1.000000000000000000 ) ) ;
#35086 = CARTESIAN_POINT ( 'NONE',  ( 786.2056067578752163, -275.8055962898685038, -374.4686193811670023 ) ) ;
#35087 = CARTESIAN_POINT ( 'NONE',  ( 776.9254006560222479, 3.809118245755632959, 314.8983024940802125 ) ) ;
#35088 = CARTESIAN_POINT ( 'NONE',  ( 763.2262854647970016, -296.6346026584195670, -309.2812353651462445 ) ) ;
#35089 = CARTESIAN_POINT ( 'NONE',  ( -746.4999999999993179, -355.4967352946684969, -16.45562775363632113 ) ) ;
#35090 = CARTESIAN_POINT ( 'NONE',  ( 780.5290396650775619, -372.3510508353228374, 365.2837595273619513 ) ) ;
#35091 = CARTESIAN_POINT ( 'NONE',  ( 772.5602148656447525, -33.72551174932952733, 305.7998596910095443 ) ) ;
#35092 = CARTESIAN_POINT ( 'NONE',  ( 791.9812246680005501, -380.6346026584192828, -361.9419747391813189 ) ) ;
#35093 = CARTESIAN_POINT ( 'NONE',  ( 755.0488828828309806, -65.80559628986925702, 344.1219089521771934 ) ) ;
#35094 = CARTESIAN_POINT ( 'NONE',  ( 756.5762568750052424, -195.1800572038744974, -348.7366044899774238 ) ) ;
#35095 = CARTESIAN_POINT ( 'NONE',  ( 793.4146539503750546, -49.98741447168749374, -307.6481478633938877 ) ) ;
#35096 = CARTESIAN_POINT ( 'NONE',  ( 802.7791456095903868, -196.7146871989598083, -329.0155153010375102 ) ) ;
#35097 = CARTESIAN_POINT ( 'NONE',  ( 795.6651683502461765, -202.7146871989597514, 371.3240766477733814 ) ) ;
#35098 = CARTESIAN_POINT ( 'NONE',  ( 757.8323909638828582, -2.634602658420536425, 352.1044303154654358 ) ) ;
#35099 = ORIENTED_EDGE ( 'NONE', *, *, #19367, .T. ) ;
#35100 = CARTESIAN_POINT ( 'NONE',  ( 801.3366627262608972, -200.5328690171415644, -353.0897708529566899 ) ) ;
#35101 = CARTESIAN_POINT ( 'NONE',  ( 755.0636971347428243, -196.2709662947835909, 341.7834795799807353 ) ) ;
#35102 = CIRCLE ( 'NONE', #18909, 19.99999999999990763 ) ;
#35103 = PRODUCT_DEFINITION_SHAPE ( 'NONE', 'NONE',  #9831 ) ;
#35104 = CARTESIAN_POINT ( 'NONE',  ( 764.3348316497523456, -46.71468719896022748, -308.6759233522265617 ) ) ;
#35105 = CARTESIAN_POINT ( 'NONE',  ( 788.7366044899766848, -323.9073299311468190, 316.5762568750059813 ) ) ;
#35106 = DIRECTION ( 'NONE',  ( 0.000000000000000000, 0.000000000000000000, 1.000000000000000000 ) ) ;
#35107 = ORIENTED_EDGE ( 'NONE', *, *, #28955, .F. ) ;
#35108 = CARTESIAN_POINT ( 'NONE',  ( 793.2243759319678702, -50.53286901714203339, 318.4439275373583200 ) ) ;
#35109 = CARTESIAN_POINT ( 'NONE',  ( 802.2119215644370342, -318.0090635724251911, -367.5423716828165084 ) ) ;
#35110 = ADVANCED_FACE ( 'NONE', ( #31917 ), #21990, .F. ) ;
#35111 = CARTESIAN_POINT ( 'NONE',  ( 777.4774526936600978, -250.2709662947833351, 304.7301800767028226 ) ) ;
#35112 = EDGE_CURVE ( 'NONE', #25018, #5395, #11371, .T. ) ;
#35113 = CARTESIAN_POINT ( 'NONE',  ( 794.1144889064781864, -442.1692326535044231, 360.9840315886528401 ) ) ;
#35114 = CARTESIAN_POINT ( 'NONE',  ( 799.2566176426618085, -144.0090635724257027, -324.0069404352559559 ) ) ;
#35115 = CARTESIAN_POINT ( 'NONE',  ( 762.1405469898971887, -145.5436935675109851, -357.8594530101015607 ) ) ;
#35116 = CARTESIAN_POINT ( 'NONE',  ( 785.3141322388236176, -357.7255117493285184, -364.4286716492789537 ) ) ;
#35117 = ORIENTED_EDGE ( 'NONE', *, *, #2078, .F. ) ;
#35118 = CIRCLE ( 'NONE', #27738, 10.00000000000000888 ) ;
#35119 = CARTESIAN_POINT ( 'NONE',  ( 814.2001403089898304, -305.3618753856922581, 347.4397851343538264 ) ) ;
#35120 = CARTESIAN_POINT ( 'NONE',  ( 759.2295555964440155, -328.1692326535048210, 353.9708237608231229 ) ) ;
#35121 = LINE ( 'NONE', #39069, #1001 ) ;
#35122 = EDGE_CURVE ( 'NONE', #32688, #35282, #44840, .T. ) ;
#35123 = CARTESIAN_POINT ( 'NONE',  ( 790.9844846989617508, -166.3726999360620198, 317.2208543904092721 ) ) ;
#35124 = CARTESIAN_POINT ( 'NONE',  ( 778.2165204200184689, -22.81642084023865280, 364.9363028652563230 ) ) ;
#35125 = VERTEX_POINT ( 'NONE', #25215 ) ;
#35126 = CARTESIAN_POINT ( 'NONE',  ( 771.3260364891663130, -379.6454272087886466, -306.0683387631859773 ) ) ;
#35127 = CARTESIAN_POINT ( 'NONE',  ( 799.9999999999993179, -512.9681489794448908, 309.9999999999998863 ) ) ;
#35128 = CARTESIAN_POINT ( 'NONE',  ( 811.3240766477731540, -244.3726999360617924, 355.6651683502462902 ) ) ;
#35129 = CARTESIAN_POINT ( 'NONE',  ( 761.2382568024794409, -183.6237781080507148, 356.9571628226838129 ) ) ;
#35130 = CARTESIAN_POINT ( 'NONE',  ( 792.1044303154645831, -348.4527844766012663, -317.8323909638837677 ) ) ;
#35131 = CARTESIAN_POINT ( 'NONE',  ( -728.8365100919714905, 256.5000000000001705, -199.9999999999890861 ) ) ;
#35132 = CARTESIAN_POINT ( 'NONE',  ( 758.4439275373578084, -228.5545181178799794, -353.2243759319684386 ) ) ;
#35133 = VECTOR ( 'NONE', #26759, 1000.000000000000000 ) ;
#35134 = CARTESIAN_POINT ( 'NONE',  ( 810.7187646348534145, -18.45278447660230725, 356.7737145352016341 ) ) ;
#35135 = CARTESIAN_POINT ( 'NONE',  ( 805.0032342141412300, -85.54369356751118403, 314.9967657858571783 ) ) ;
#35136 = DIRECTION ( 'NONE',  ( -0.000000000000000000, -4.857225732735055920E-15, 1.000000000000000000 ) ) ;
#35137 = CARTESIAN_POINT ( 'NONE',  ( 813.1304606946831655, -401.9073299311464211, -352.3570229623691716 ) ) ;
#35138 = LINE ( 'NONE', #7213, #21704 ) ;
#35139 = ADVANCED_FACE ( 'NONE', ( #43008 ), #4453, .F. ) ;
#35140 = CARTESIAN_POINT ( 'NONE',  ( 812.3518521366052028, -361.0999726633341425, 326.5853460496235243 ) ) ;
#35141 = ADVANCED_FACE ( 'NONE', ( #12283, #5563 ), #29824, .F. ) ;
#35142 = CARTESIAN_POINT ( 'NONE',  ( 809.6099558218720631, -452.9681489794449476, -335.1781210895659342 ) ) ;
#35143 = CARTESIAN_POINT ( 'NONE',  ( 758.8095938919642549, -320.0891481129648355, 311.6929314249763365 ) ) ;
#35144 = CARTESIAN_POINT ( 'NONE',  ( 748.9653473494363425, -50.63460265842036989, -356.9462024416521331 ) ) ;
#35145 = CARTESIAN_POINT ( 'NONE',  ( 771.1735550268778070, -297.1800572038740711, -316.3353852180827630 ) ) ;
#35146 = FACE_BOUND ( 'NONE', #23224, .T. ) ;
#35147 = CARTESIAN_POINT ( 'NONE',  ( 762.3223304703356007, -391.5436935675101608, 322.3223304703362828 ) ) ;
#35148 = CARTESIAN_POINT ( 'NONE',  ( 766.9102291470427417, -138.5545181178802636, 318.6633372737382501 ) ) ;
#35149 = CARTESIAN_POINT ( 'NONE',  ( 762.1177392798416577, -18.55451811788065797, -309.8865473780659272 ) ) ;
#35150 = CARTESIAN_POINT ( 'NONE',  ( 803.8651313633788504, -101.2601417444146250, -332.4468031744301015 ) ) ;
#35151 = CARTESIAN_POINT ( 'NONE',  ( 744.8212110874229666, -90.89650538077827946, 336.2046728542121627 ) ) ;
#35152 = CARTESIAN_POINT ( 'NONE',  ( 797.6776695296629214, -403.5436935675101608, 357.6776695296636603 ) ) ;
#35153 = CARTESIAN_POINT ( 'NONE',  ( 814.2001403089898304, 6.638124614306706306, 347.4397851343538264 ) ) ;
#35154 = CYLINDRICAL_SURFACE ( 'NONE', #15951, 2.749999999999835687 ) ;
#35155 = CARTESIAN_POINT ( 'NONE',  ( 755.0636971347428243, -4.270966294784170003, -341.7834795799807353 ) ) ;
#35157 = EDGE_LOOP ( 'NONE', ( #31873, #15840 ) ) ;
#35156 = CARTESIAN_POINT ( 'NONE',  ( 798.7617431975189675, -99.62377810805098477, -323.0428371773161871 ) ) ;
#35158 = CARTESIAN_POINT ( 'NONE',  ( 804.9363028652555840, -64.27096629478397460, -338.2165204200192079 ) ) ;
#35159 = VECTOR ( 'NONE', #82, 1000.000000000000000 ) ;
#35160 = CARTESIAN_POINT ( 'NONE',  ( 769.1273215169530886, -406.7146871989590409, -317.4527132478988847 ) ) ;
#35162 = CARTESIAN_POINT ( 'NONE',  ( 788.8264449731201466, -213.1800572038743837, 363.6646147819170665 ) ) ;
#35161 = CARTESIAN_POINT ( 'NONE',  ( 788.7366044899766848, -227.9073299311471033, 316.5762568750059813 ) ) ;
#35163 = VECTOR ( 'NONE', #33982, 1000.000000000000000 ) ;
#35164 = VERTEX_POINT ( 'NONE', #8815 ) ;
#35165 = CARTESIAN_POINT ( 'NONE',  ( 749.8865473780648472, -404.5328690171409107, -322.1177392798429082 ) ) ;
#35167 = EDGE_CURVE ( 'NONE', #21532, #66, #36534, .T. ) ;
#35166 = FACE_OUTER_BOUND ( 'NONE', #25568, .T. ) ;
#35168 = ORIENTED_EDGE ( 'NONE', *, *, #22408, .T. ) ;
#35169 = CARTESIAN_POINT ( 'NONE',  ( 785.3687786644884454, -443.3618753856917465, 315.3201227861279676 ) ) ;
#35170 = CIRCLE ( 'NONE', #45505, 6.119000000000013095 ) ;
#35171 = EDGE_CURVE ( 'NONE', #10285, #39064, #7229, .T. ) ;
#35172 = ORIENTED_EDGE ( 'NONE', *, *, #3488, .F. ) ;
#35173 =( NAMED_UNIT ( * ) SI_UNIT ( $, .STERADIAN. ) SOLID_ANGLE_UNIT ( ) );
#35174 = AXIS2_PLACEMENT_3D ( 'NONE', #24901, #10588, #35518 ) ;
#35175 = CARTESIAN_POINT ( 'NONE',  ( 782.5225473063381969, -238.2709662947833920, -375.2698199232970637 ) ) ;
#35176 = CARTESIAN_POINT ( 'NONE',  ( 792.2312462859673587, -155.9073299311473306, 307.2067596250082602 ) ) ;
#35177 = EDGE_CURVE ( 'NONE', #34117, #41429, #15524, .T. ) ;
#35178 = ORIENTED_EDGE ( 'NONE', *, *, #41944, .T. ) ;
#35179 = CARTESIAN_POINT ( 'NONE',  ( 759.9864689768902508, -242.0891481129652618, -354.9819416627836404 ) ) ;
#35180 = ORIENTED_EDGE ( 'NONE', *, *, #38840, .F. ) ;
#35181 = CARTESIAN_POINT ( 'NONE',  ( 771.1735550268778070, -345.1800572038739006, -316.3353852180827630 ) ) ;
#35182 = CARTESIAN_POINT ( 'NONE',  ( 755.5713283507202505, -5.361875385693257279, -334.6858677611754729 ) ) ;
#35183 = CARTESIAN_POINT ( 'NONE',  ( 754.8983024940795303, -234.8965053807777963, 336.9254006560228163 ) ) ;
#35184 = CARTESIAN_POINT ( 'NONE',  ( 181.1634899080285948, 230.0000000000000000, -202.7499999999952536 ) ) ;
#35185 = DIRECTION ( 'NONE',  ( 0.000000000000000000, 0.000000000000000000, 1.000000000000000000 ) ) ;
#35186 = EDGE_LOOP ( 'NONE', ( #33663, #33979 ) ) ;
#35187 = CARTESIAN_POINT ( 'NONE',  ( 762.1405469898971887, -25.54369356751136877, -357.8594530101015607 ) ) ;
#35188 = CARTESIAN_POINT ( 'NONE',  ( 755.2512626584698410, 16.45630643248849267, -315.2512626584710915 ) ) ;
#35189 = FACE_BOUND ( 'NONE', #17458, .T. ) ;
#35190 = EDGE_LOOP ( 'NONE', ( #22352, #7122, #19909, #14275 ) ) ;
#35191 = CARTESIAN_POINT ( 'NONE',  ( 814.4686193811664907, -267.2817908451526137, -346.2056067578752732 ) ) ;
#35192 = CARTESIAN_POINT ( 'NONE',  ( 815.3608509340175488, -122.7363362996985074, 341.2497674668889545 ) ) ;
#35194 = CARTESIAN_POINT ( 'NONE',  ( 785.3141322388236176, -213.7255117493289731, -364.4286716492789537 ) ) ;
#35193 = FACE_OUTER_BOUND ( 'NONE', #2318, .T. ) ;
#35195 = CARTESIAN_POINT ( 'NONE',  ( 790.8726784830453198, -394.7146871989591546, -362.5472867521010585 ) ) ;
#35196 = CARTESIAN_POINT ( 'NONE',  ( -728.8365100919714905, 260.0000000000001705, -208.0249999999890349 ) ) ;
#35197 = CARTESIAN_POINT ( 'NONE',  ( 759.0159684113467620, -112.9181544815167229, -325.8855110935213020 ) ) ;
#35198 = VECTOR ( 'NONE', #32062, 1000.000000000000000 ) ;
#35199 = CARTESIAN_POINT ( 'NONE',  ( 760.0363995740630116, -394.9181544815158418, 368.7758568127991907 ) ) ;
#35200 = LINE ( 'NONE', #34737, #8464 ) ;
#35201 = CARTESIAN_POINT ( 'NONE',  ( 813.9316612368132837, 16.55804007376685050, -348.6739635108323228 ) ) ;
#35202 = CARTESIAN_POINT ( 'NONE',  ( 749.2812353651451076, -318.4527844766014368, -323.2262854647983090 ) ) ;
#35203 = DIRECTION ( 'NONE',  ( -1.058954862565134068E-16, 0.6438296778008191223, -0.7651688349527137056 ) ) ;
#35204 = CARTESIAN_POINT ( 'NONE',  ( 803.6646147819161570, -89.90732993114750116, -348.8264449731210561 ) ) ;
#35205 = AXIS2_PLACEMENT_3D ( 'NONE', #31069, #24134, #44947 ) ;
#35206 = CARTESIAN_POINT ( 'NONE',  ( 745.7194118038753459, -253.6454272087889876, 348.7631598425976449 ) ) ;
#35207 = CARTESIAN_POINT ( 'NONE',  ( 786.2056067578752163, -203.8055962898688449, -374.4686193811670023 ) ) ;
#35208 = CARTESIAN_POINT ( 'NONE',  ( 782.4968714119720516, -226.8164208402380098, 305.0891759886411023 ) ) ;
#35209 = CARTESIAN_POINT ( 'NONE',  ( 744.7301800767019131, -436.8164208402372992, -337.4774526936615757 ) ) ;
#35210 = CIRCLE ( 'NONE', #43329, 30.00000000000008171 ) ;
#35211 = DIRECTION ( 'NONE',  ( 0.000000000000000000, 0.000000000000000000, 1.000000000000000000 ) ) ;
#35212 = CARTESIAN_POINT ( 'NONE',  ( 801.9419747391806368, -306.4527844766013800, 351.9812246680014027 ) ) ;
#35213 = CARTESIAN_POINT ( 'NONE',  ( 804.8461984189677878, -98.19088175424404596, 336.9566956441385628 ) ) ;
#35214 = CARTESIAN_POINT ( 'NONE',  ( 798.7617431975189675, 20.37622189194865285, -323.0428371773161871 ) ) ;
#35215 = CARTESIAN_POINT ( 'NONE',  ( 799.9999999999993179, -365.3551492539851893, 1.867567485292990437 ) ) ;
#35216 = CARTESIAN_POINT ( 'NONE',  ( 1238.921997096861332, 579.9999999999998863, -360.0000000000000000 ) ) ;
#35218 = CARTESIAN_POINT ( 'NONE',  ( 764.8639956371174549, -368.0891481129647786, 319.7806653035542013 ) ) ;
#35217 = CARTESIAN_POINT ( 'NONE',  ( 802.7791456095903868, -124.7146871989599930, 329.0155153010375102 ) ) ;
#35219 = VERTEX_POINT ( 'NONE', #33748 ) ;
#35220 = CARTESIAN_POINT ( 'NONE',  ( 803.2186876482843445, -247.9874144716867761, -350.0220218866286928 ) ) ;
#35221 = CARTESIAN_POINT ( 'NONE',  ( 756.5762568750052424, -99.18005720387478164, 348.7366044899774238 ) ) ;
#35222 = CARTESIAN_POINT ( 'NONE',  ( 791.1614460488616487, -299.2601417444139997, -373.5763878283158874 ) ) ;
#35223 = CARTESIAN_POINT ( 'NONE',  ( -265.7583438952257779, 430.0000000000002842, -320.0000000000000568 ) ) ;
#35224 = CARTESIAN_POINT ( 'NONE',  ( 751.2241431872005251, -424.1692326535044799, 359.9636004259367610 ) ) ;
#35225 = ORIENTED_EDGE ( 'NONE', *, *, #34333, .T. ) ;
#35226 = CARTESIAN_POINT ( 'NONE',  ( 758.0580252608178853, -318.4527844766014368, 328.0187753319985404 ) ) ;
#35227 = CARTESIAN_POINT ( 'NONE',  ( 801.3366627262608972, -32.53286901714208312, -353.0897708529566899 ) ) ;
#35228 = CARTESIAN_POINT ( 'NONE',  ( 785.3141322388236176, -213.7255117493289731, -364.4286716492789537 ) ) ;
#35229 = CARTESIAN_POINT ( 'NONE',  ( 801.9419747391806368, -402.4527844766010389, 351.9812246680014027 ) ) ;
#35230 = CARTESIAN_POINT ( 'NONE',  ( 787.5162901302840055, -155.3618753856927128, -305.4481719005792684 ) ) ;
#35231 = CARTESIAN_POINT ( 'NONE',  ( 765.0180583372156207, -144.9982390220564525, -360.0135310231089534 ) ) ;
#35232 = ORIENTED_EDGE ( 'NONE', *, *, #28077, .F. ) ;
#35233 = AXIS2_PLACEMENT_3D ( 'NONE', #6246, #24018, #2317 ) ;
#35234 = CARTESIAN_POINT ( 'NONE',  ( 761.4292242960306112, -377.4636090269704596, -323.2154366446414429 ) ) ;
#35236 = CARTESIAN_POINT ( 'NONE',  ( 790.9844846989617508, -430.3726999360611671, 317.2208543904092721 ) ) ;
#35235 = CARTESIAN_POINT ( 'NONE',  ( 771.1735550268778070, -129.1800572038746111, 316.3353852180827630 ) ) ;
#35237 = CARTESIAN_POINT ( 'NONE',  ( 773.3843516231979720, -133.4419599262326699, 364.4086373105754433 ) ) ;
#35240 = CARTESIAN_POINT ( 'NONE',  ( 783.7566961878529810, -384.8965053807772847, 305.1792804349288417 ) ) ;
#35239 = CARTESIAN_POINT ( 'NONE',  ( 799.9999999999993179, -512.9681489794448908, 339.9999999999999432 ) ) ;
#35238 = DIRECTION ( 'NONE',  ( -1.000000000000000000, 0.000000000000000000, 0.000000000000000000 ) ) ;
#35241 = ORIENTED_EDGE ( 'NONE', *, *, #17279, .T. ) ;
#35242 = CARTESIAN_POINT ( 'NONE',  ( 763.8424801807145741, -378.0090635724250774, -320.5453621957614700 ) ) ;
#35243 = CARTESIAN_POINT ( 'NONE',  ( 765.0180583372156207, -360.9982390220557704, -360.0135310231089534 ) ) ;
#35244 = CARTESIAN_POINT ( 'NONE',  ( 754.3581564841646241, -161.4636090269711133, -316.1443688327762516 ) ) ;
#35245 = CARTESIAN_POINT ( 'NONE',  ( 748.6759233522253680, -40.37269993606240348, 324.3348316497537098 ) ) ;
#35247 = LINE ( 'NONE', #20693, #26950 ) ;
#35246 = DIRECTION ( 'NONE',  ( -0.000000000000000000, 1.000000000000000000, -0.000000000000000000 ) ) ;
#35248 = CARTESIAN_POINT ( 'NONE',  ( 764.0069404352550464, -279.0783235625958127, -359.2566176426627180 ) ) ;
#35249 = CARTESIAN_POINT ( 'NONE',  ( 756.3353852180819104, -437.9073299311463074, -331.1735550268788302 ) ) ;
#35250 = CARTESIAN_POINT ( 'NONE',  ( 748.6759233522253680, -160.3726999360620482, -324.3348316497537098 ) ) ;
#35251 = CARTESIAN_POINT ( 'NONE',  ( 181.1634899080285948, 240.0000000000000284, -199.9999999999953957 ) ) ;
#35252 = PLANE ( 'NONE',  #43007 ) ;
#35253 = CARTESIAN_POINT ( 'NONE',  ( 766.9102291470427417, -354.5545181178796383, 318.6633372737382501 ) ) ;
#35254 = CARTESIAN_POINT ( 'NONE',  ( 809.0717654672305343, -340.9181544815160123, 360.1688906516309885 ) ) ;
#35255 = CARTESIAN_POINT ( 'NONE',  ( 792.3570229623691148, -213.1800572038743837, -373.1304606946836770 ) ) ;
#35256 = DIRECTION ( 'NONE',  ( 1.000000000000000000, 0.000000000000000000, 0.000000000000000000 ) ) ;
#35257 = DIRECTION ( 'NONE',  ( -1.000000000000000000, 0.000000000000000000, 0.000000000000000000 ) ) ;
#35258 = CARTESIAN_POINT ( 'NONE',  ( 809.0717654672305343, -148.9181544815166092, 360.1688906516309885 ) ) ;
#35259 = CARTESIAN_POINT ( 'NONE',  ( 791.1614460488616487, -107.2601417444145824, -373.5763878283158874 ) ) ;
#35260 = CARTESIAN_POINT ( 'NONE',  ( 804.7487373415286811, -67.54369356751125508, 364.7487373415288516 ) ) ;
#35261 = CARTESIAN_POINT ( 'NONE',  ( 772.4837098697144029, -335.3618753856920307, -374.5518280994205611 ) ) ;
#35262 = CYLINDRICAL_SURFACE ( 'NONE', #15266, 9.999999999999980460 ) ;
#35263 = CARTESIAN_POINT ( 'NONE',  ( -78.83651009197140525, 260.0000000000000568, -199.9999999999936051 ) ) ;
#35264 = CARTESIAN_POINT ( 'NONE',  ( 762.3223304703356007, -199.5436935675108430, 322.3223304703362828 ) ) ;
#35265 = CARTESIAN_POINT ( 'NONE',  ( 804.1009440267234822, -455.4636090269701754, 314.0944755984392600 ) ) ;
#35266 = CARTESIAN_POINT ( 'NONE',  ( 764.3348316497523456, -406.7146871989590409, -308.6759233522265617 ) ) ;
#35267 = AXIS2_PLACEMENT_3D ( 'NONE', #45680, #44761, #20495 ) ;
#35268 = CARTESIAN_POINT ( 'NONE',  ( 754.9967657858570647, -145.5436935675109851, -365.0032342141425374 ) ) ;
#35269 = CARTESIAN_POINT ( 'NONE',  ( 748.9653473494363425, -434.6346026584190554, -356.9462024416521331 ) ) ;
#35270 = CARTESIAN_POINT ( 'NONE',  ( 799.9999999999993179, 205.0000000000000568, -339.9999999999999432 ) ) ;
#35271 = CARTESIAN_POINT ( 'NONE',  ( 805.9055244015594326, 20.37622189194865285, 315.8990559732753240 ) ) ;
#35272 = ORIENTED_EDGE ( 'NONE', *, *, #15065, .T. ) ;
#35273 = CARTESIAN_POINT ( 'NONE',  ( 807.5423716828161105, -201.0783235625961254, -362.2119215644372048 ) ) ;
#35274 =( NAMED_UNIT ( * ) PLANE_ANGLE_UNIT ( ) SI_UNIT ( $, .RADIAN. ) );
#35275 = CARTESIAN_POINT ( 'NONE',  ( 744.9990715423526808, -306.3510508353230648, 341.2370466360926002 ) ) ;
#35276 = CARTESIAN_POINT ( 'NONE',  ( 759.7806653035535192, -126.9982390220565094, 324.8639956371181370 ) ) ;
#35277 = ORIENTED_EDGE ( 'NONE', *, *, #15930, .F. ) ;
#35278 = CARTESIAN_POINT ( 'NONE',  ( 804.9363028652555840, -304.2709662947832499, 338.2165204200192079 ) ) ;
#35279 = CARTESIAN_POINT ( 'NONE',  ( 755.2512626584698410, -31.54369356751135456, -315.2512626584710915 ) ) ;
#35280 = ADVANCED_FACE ( 'NONE', ( #2098, #23338 ), #1198, .F. ) ;
#35281 = CARTESIAN_POINT ( 'NONE',  ( 758.8095938919644823, -80.08914811296574499, 311.6929314249762797 ) ) ;
#35282 = VERTEX_POINT ( 'NONE', #37197 ) ;
#35283 = CARTESIAN_POINT ( 'NONE',  ( 764.1737431748507561, -442.3726999360611103, -371.6461892240376415 ) ) ;
#35284 = ORIENTED_EDGE ( 'NONE', *, *, #8056, .T. ) ;
#35285 = ITEM_DEFINED_TRANSFORMATION ( 'NONE', 'NONE', #18686,  #26858 ) ;
#35286 = CARTESIAN_POINT ( 'NONE',  ( 778.1981804954714335, -10.27096629478414691, 314.8072714833589885 ) ) ;
#35287 = CARTESIAN_POINT ( 'NONE',  ( 802.1676090361156639, -254.6346026584196238, -327.8955696845344505 ) ) ;
#35289 = CARTESIAN_POINT ( 'NONE',  ( 771.2368401574024119, -277.4419599262322436, 374.2805881961240857 ) ) ;
#35288 = CARTESIAN_POINT ( 'NONE',  ( 767.7687537140311633, -359.9073299311467053, 372.7932403749916830 ) ) ;
#35290 = CARTESIAN_POINT ( 'NONE',  ( 771.2368401574024119, -61.44195992623291147, 374.2805881961240857 ) ) ;
#35291 = CARTESIAN_POINT ( 'NONE',  ( 783.0745993439762742, -248.1908817542435202, -365.1016975059196739 ) ) ;
#35292 = CARTESIAN_POINT ( 'NONE',  ( 771.2633955100217236, -263.9073299311469327, -363.4237431249939618 ) ) ;
#35293 = CARTESIAN_POINT ( 'NONE',  ( 790.0183182880230106, -452.9681489794449476, -362.9048749981275250 ) ) ;
#35294 = CARTESIAN_POINT ( 'NONE',  ( 756.5762568750052424, -123.1800572038747106, -348.7366044899774238 ) ) ;
#35295 = CARTESIAN_POINT ( 'NONE',  ( 785.3141322388236176, -261.7255117493288026, 364.4286716492789537 ) ) ;
#35296 = CIRCLE ( 'NONE', #21287, 12.00000000000001066 ) ;
#35297 = CARTESIAN_POINT ( 'NONE',  ( 808.0189434323515343, -398.0891481129647218, 319.0252816721025511 ) ) ;
#35299 = CARTESIAN_POINT ( 'NONE',  ( -786.4999999999993179, -110.5936016518799221, 750.6326042729449455 ) ) ;
#35298 = CARTESIAN_POINT ( 'NONE',  ( -468.8365100919714337, 240.0000000000001421, -199.9999999999908766 ) ) ;
#35300 = CARTESIAN_POINT ( 'NONE',  ( 755.8990559732751535, -59.46360902697142592, -365.9055244015606831 ) ) ;
#35301 = DIRECTION ( 'NONE',  ( 1.000000000000000000, 0.000000000000000000, 0.000000000000000000 ) ) ;
#35302 = CARTESIAN_POINT ( 'NONE',  ( 914.9999999999992042, 74.99999999999984368, -350.0000000000000000 ) ) ;
#35303 = CARTESIAN_POINT ( 'NONE',  ( 769.0155153010367712, -274.3726999360617356, 362.7791456095907279 ) ) ;
#35304 = CARTESIAN_POINT ( 'NONE',  ( 774.6858677611749044, -105.7255117493293000, 315.5713283507209894 ) ) ;
#35305 = ORIENTED_EDGE ( 'NONE', *, *, #32866, .F. ) ;
#35306 = CARTESIAN_POINT ( 'NONE',  ( 757.4527132478984868, -16.37269993606248519, -329.1273215169538844 ) ) ;
#35307 = CARTESIAN_POINT ( 'NONE',  ( 746.8695393053151292, -101.9073299311474869, -327.6429770376306578 ) ) ;
#35308 = CARTESIAN_POINT ( 'NONE',  ( 769.1273215169530886, -286.7146871989594388, 317.4527132478988847 ) ) ;
#35309 = CARTESIAN_POINT ( 'NONE',  ( 795.1360043628807261, -452.0891481129646650, -360.2193346964456282 ) ) ;
#35310 = CARTESIAN_POINT ( 'NONE',  ( 791.0478386215596629, -45.82724539060783542, 306.7653713866226326 ) ) ;
#35311 = CARTESIAN_POINT ( 'NONE',  ( 763.2262854647970016, -224.6346026584198228, -309.2812353651462445 ) ) ;
#35312 = CARTESIAN_POINT ( 'NONE',  ( 792.2312462859673587, -179.9073299311472454, 307.2067596250082602 ) ) ;
#35313 = CARTESIAN_POINT ( 'NONE',  ( 785.3687786644884454, -83.36187538569296862, 315.3201227861279676 ) ) ;
#35314 = CARTESIAN_POINT ( 'NONE',  ( 744.9990715423526808, -282.3510508353230080, -341.2370466360926002 ) ) ;
#35315 = CARTESIAN_POINT ( 'NONE',  ( 813.5763878283155464, -459.8272453906066062, 351.1614460488615350 ) ) ;
#35316 = CARTESIAN_POINT ( 'NONE',  ( 813.1304606946830518, -305.9073299311467622, -352.3570229623690580 ) ) ;
#35317 = FACE_BOUND ( 'NONE', #20393, .T. ) ;
#35318 = CARTESIAN_POINT ( 'NONE',  ( 796.7845633553578182, -369.6237781080500895, 358.5707757039688204 ) ) ;
#35319 = CARTESIAN_POINT ( 'NONE',  ( 751.9810565676468741, -50.08914811296584446, 360.9747183278973921 ) ) ;
#35320 = CARTESIAN_POINT ( 'NONE',  ( 771.1735550268778070, -393.1800572038737300, -316.3353852180827630 ) ) ;
#35321 = CARTESIAN_POINT ( 'NONE',  ( 779.4709603349208464, -48.35105083532386061, 314.7162404726379918 ) ) ;
#35323 = EDGE_CURVE ( 'NONE', #44845, #44771, #36760, .T. ) ;
#35322 = CARTESIAN_POINT ( 'NONE',  ( 807.5423716828161105, -81.07832356259649487, -362.2119215644372048 ) ) ;
#35324 = CARTESIAN_POINT ( 'NONE',  ( 793.4146539503750546, -217.9874144716870035, 307.6481478633938877 ) ) ;
#35325 = CARTESIAN_POINT ( 'NONE',  ( 758.0580252608178853, -30.45278447660226817, 328.0187753319985404 ) ) ;
#35326 = AXIS2_PLACEMENT_3D ( 'NONE', #6916, #42033, #21462 ) ;
#35327 = ORIENTED_EDGE ( 'NONE', *, *, #37858, .T. ) ;
#35328 = CARTESIAN_POINT ( 'NONE',  ( 760.5453621957607311, -213.0783235625960401, -323.8424801807151425 ) ) ;
#35329 = CARTESIAN_POINT ( 'NONE',  ( 803.4237431249931660, -207.1800572038744406, 331.2633955100225194 ) ) ;
#35330 = EDGE_CURVE ( 'NONE', #1374, #40310, #43682, .T. ) ;
#35331 = CARTESIAN_POINT ( 'NONE',  ( 747.3154664389472828, -19.98741447168758256, -326.4474001241230781 ) ) ;
#35332 = CARTESIAN_POINT ( 'NONE',  ( 768.0187753319979720, -320.6346026584195670, 318.0580252608186242 ) ) ;
#35333 = CARTESIAN_POINT ( 'NONE',  ( 939.9999999999992042, 56.73212367640090292, -362.5753187112032947 ) ) ;
#35334 = ORIENTED_EDGE ( 'NONE', *, *, #41924, .T. ) ;
#35335 = CARTESIAN_POINT ( 'NONE',  ( 779.4709603349208464, -48.35105083532386061, 314.7162404726379918 ) ) ;
#35336 = CARTESIAN_POINT ( 'NONE',  ( 748.6759233522253680, -304.3726999360615082, -324.3348316497537098 ) ) ;
#35337 =( BOUNDED_CURVE ( )  B_SPLINE_CURVE ( 3, ( #15816, #40543, #40331, #19502 ),
 .UNSPECIFIED., .F., .T. ) 
 B_SPLINE_CURVE_WITH_KNOTS ( ( 4, 4 ),
 ( 4.691336726374857768, 4.712707788662813257 ),
 .UNSPECIFIED. ) 
 CURVE ( )  GEOMETRIC_REPRESENTATION_ITEM ( )  RATIONAL_B_SPLINE_CURVE ( ( 1.000000000000000000, 0.9999619401702002364, 0.9999619401702002364, 1.000000000000000000 ) ) 
 REPRESENTATION_ITEM ( '' )  );
#35338 = CARTESIAN_POINT ( 'NONE',  ( 787.4397851343537695, -261.7255117493288026, 374.2001403089903988 ) ) ;
#35339 = CARTESIAN_POINT ( 'NONE',  ( 815.1787889125755555, 17.10349461922139369, 343.7953271457877804 ) ) ;
#35340 = CARTESIAN_POINT ( 'NONE',  ( 761.4292242960306112, -161.4636090269711133, -323.2154366446414429 ) ) ;
#35341 = CARTESIAN_POINT ( 'NONE',  ( 788.8264449731200330, -141.1800572038746395, -363.6646147819171233 ) ) ;
#35342 = CARTESIAN_POINT ( 'NONE',  ( 755.5713283507202505, -341.3618753856922012, -334.6858677611754729 ) ) ;
#35343 = ORIENTED_EDGE ( 'NONE', *, *, #17738, .F. ) ;
#35344 = CARTESIAN_POINT ( 'NONE',  ( 800.9747183278959710, -276.9982390220559978, 311.9810565676471583 ) ) ;
#35345 = CARTESIAN_POINT ( 'NONE',  ( -598.8365100919716042, 260.0000000000001705, -202.7499999999898250 ) ) ;
#35346 = CARTESIAN_POINT ( 'NONE',  ( 773.3843516231979720, -325.4419599262320162, 364.4086373105754433 ) ) ;
#35347 = CARTESIAN_POINT ( 'NONE',  ( -809.9999999999993179, -512.9681489794448908, -339.9999999999999432 ) ) ;
#35348 = CARTESIAN_POINT ( 'NONE',  ( 757.4527132478984868, -160.3726999360620482, 329.1273215169538844 ) ) ;
#35349 = CARTESIAN_POINT ( 'NONE',  ( 797.8594530101008786, -13.54369356751140785, 322.1405469898980982 ) ) ;
#35350 = EDGE_CURVE ( 'NONE', #29032, #17994, #13123, .T. ) ;
#35351 = ORIENTED_EDGE ( 'NONE', *, *, #10512, .F. ) ;
#35352 = CARTESIAN_POINT ( 'NONE',  ( 768.9521613784389729, -393.8272453906067199, -373.2346286133773106 ) ) ;
#35353 = CARTESIAN_POINT ( 'NONE',  ( 777.4774526936600978, -10.27096629478415046, -304.7301800767028226 ) ) ;
#35354 = CARTESIAN_POINT ( 'NONE',  ( 778.7629533639073998, -224.7363362996982232, 375.0009284576466371 ) ) ;
#35355 = VECTOR ( 'NONE', #36104, 1000.000000000000000 ) ;
#35356 = CARTESIAN_POINT ( 'NONE',  ( 805.0264073115434940, -174.3510508353234627, 339.4763451958999099 ) ) ;
#35357 = CARTESIAN_POINT ( 'NONE',  ( 759.7806653035534055, -366.9982390220556567, -324.8639956371180801 ) ) ;
#35358 = CARTESIAN_POINT ( 'NONE',  ( 796.9571628226829034, -455.4636090269701754, 321.2382568024804641 ) ) ;
#35359 = CARTESIAN_POINT ( 'NONE',  ( 776.9254006560222479, -236.1908817542436338, -314.8983024940802125 ) ) ;
#35360 = CARTESIAN_POINT ( 'NONE',  ( 751.9810565676468741, -2.089148112965993231, 360.9747183278973921 ) ) ;
#35361 = CARTESIAN_POINT ( 'NONE',  ( 745.4481719005789273, -75.72551174932937101, 347.5162901302853129 ) ) ;
#35362 = DIRECTION ( 'NONE',  ( 1.000000000000000000, -1.892425610156518354E-16, 0.000000000000000000 ) ) ;
#35363 = CARTESIAN_POINT ( 'NONE',  ( 745.4481719005789273, -411.7255117493282910, -347.5162901302853697 ) ) ;
#35364 = LINE ( 'NONE', #37924, #45314 ) ;
#35365 = CARTESIAN_POINT ( 'NONE',  ( 805.6418435158337843, -365.4636090269705164, 363.8556311672236916 ) ) ;
#35366 = CARTESIAN_POINT ( 'NONE',  ( 180.7583438952261474, 1.505115564641941601E-13, -244.9999999999999716 ) ) ;
#35367 = CARTESIAN_POINT ( 'NONE',  ( 772.5602148656447525, -321.7255117493286320, 305.7998596910095443 ) ) ;
#35368 = CARTESIAN_POINT ( 'NONE',  ( 782.5225473063381969, -46.27096629478404566, -375.2698199232970637 ) ) ;
#35369 = CARTESIAN_POINT ( 'NONE',  ( 764.8639956371174549, -272.0891481129651197, -319.7806653035542013 ) ) ;
#35370 = ADVANCED_FACE ( 'NONE', ( #9027 ), #33514, .F. ) ;
#35371 = CARTESIAN_POINT ( 'NONE',  ( 4.541821464375645154E-14, 240.0000000000000568, 0.000000000000000000 ) ) ;
#35372 = CARTESIAN_POINT ( 'NONE',  ( 804.4286716492782716, -425.3618753856919170, 345.3141322388244703 ) ) ;
#35373 = CARTESIAN_POINT ( 'NONE',  ( 766.0291762391763086, -202.9181544815164386, 360.7704444035551319 ) ) ;
#35374 = CARTESIAN_POINT ( 'NONE',  ( 749.5768839229115201, -36.55451811788061178, -358.0661480581553064 ) ) ;
#35375 = CARTESIAN_POINT ( 'NONE',  ( 764.0069404352550464, -87.07832356259646645, -359.2566176426627180 ) ) ;
#35376 = CARTESIAN_POINT ( 'NONE',  ( 776.2433038121456548, -84.89650538077830788, 374.8207195650711014 ) ) ;
#35377 = CARTESIAN_POINT ( 'NONE',  ( 754.8072714833583632, -388.8164208402374129, 338.1981804954721156 ) ) ;
#35378 = CARTESIAN_POINT ( 'NONE',  ( 795.1360043628807261, -452.0891481129646650, 360.2193346964456282 ) ) ;
#35379 = ORIENTED_EDGE ( 'NONE', *, *, #16508, .F. ) ;
#35380 = CARTESIAN_POINT ( 'NONE',  ( 759.9864689768902508, -98.08914811296568814, -354.9819416627836404 ) ) ;
#35381 = ADVANCED_FACE ( 'NONE', ( #16188 ), #5116, .T. ) ;
#35382 = ADVANCED_FACE ( 'NONE', ( #26125 ), #40240, .T. ) ;
#35383 = CARTESIAN_POINT ( 'NONE',  ( 793.2243759319678702, -410.5328690171408539, -318.4439275373583200 ) ) ;
#35385 = CARTESIAN_POINT ( 'NONE',  ( 801.9419747391806368, -234.4527844766016358, 351.9812246680014027 ) ) ;
#35384 = CARTESIAN_POINT ( 'NONE',  ( 805.1927285166397041, -232.8164208402379245, 341.8018195045277707 ) ) ;
#35386 = CARTESIAN_POINT ( 'NONE',  ( 748.3538107759620743, -400.7146871989590977, -355.8262568251490165 ) ) ;
#35387 = CARTESIAN_POINT ( 'NONE',  ( 989.9999999999992042, 46.15097736693707020, 350.0000000000000000 ) ) ;
#35388 = ORIENTED_EDGE ( 'NONE', *, *, #5139, .T. ) ;
#35389 = CARTESIAN_POINT ( 'NONE',  ( 755.5713283507202505, -413.3618753856920307, 334.6858677611754729 ) ) ;
#35390 = VERTEX_POINT ( 'NONE', #44362 ) ;
#35391 =( LENGTH_UNIT ( ) NAMED_UNIT ( * ) SI_UNIT ( .MILLI., .METRE. ) );
#35392 = CARTESIAN_POINT ( 'NONE',  ( 796.7737145352015204, -236.6346026584198228, -370.7187646348536987 ) ) ;
#35393 = CARTESIAN_POINT ( 'NONE',  ( 801.1904061080338124, -164.0891481129654892, 368.3070685750236066 ) ) ;
#35394 = CARTESIAN_POINT ( 'NONE',  ( 757.4527132478984868, -280.3726999360616787, 329.1273215169538844 ) ) ;
#35395 = ORIENTED_EDGE ( 'NONE', *, *, #32872, .F. ) ;
#35396 = CARTESIAN_POINT ( 'NONE',  ( 781.7834795799800531, -250.8164208402379245, -315.0636971347436202 ) ) ;
#35397 = ORIENTED_EDGE ( 'NONE', *, *, #13311, .T. ) ;
#35398 = EDGE_CURVE ( 'NONE', #38320, #45077, #33291, .T. ) ;
#35399 = CARTESIAN_POINT ( 'NONE',  ( 754.8072714833581358, -364.8164208402374697, -338.1981804954720587 ) ) ;
#35400 = CARTESIAN_POINT ( 'NONE',  ( 756.3353852180819104, -29.90732993114771787, -331.1735550268788302 ) ) ;
#35401 = ADVANCED_FACE ( 'NONE', ( #15969 ), #30051, .T. ) ;
#35402 = CARTESIAN_POINT ( 'NONE',  ( 786.6156483768007774, -241.4419599262322720, 315.5913626894246136 ) ) ;
#35403 = DIRECTION ( 'NONE',  ( -0.000000000000000000, 1.000000000000000000, -0.000000000000000000 ) ) ;
#35404 = FACE_OUTER_BOUND ( 'NONE', #45214, .T. ) ;
#35405 = ORIENTED_EDGE ( 'NONE', *, *, #17918, .F. ) ;
#35406 = CARTESIAN_POINT ( 'NONE',  ( 762.3223304703356007, -7.543693567511430942, -322.3223304703362828 ) ) ;
#35407 = DIRECTION ( 'NONE',  ( 0.000000000000000000, 0.7372773368101421809, -0.6755902076156404812 ) ) ;
#35408 = DIRECTION ( 'NONE',  ( 0.000000000000000000, 0.000000000000000000, 1.000000000000000000 ) ) ;
#35409 = EDGE_CURVE ( 'NONE', #4454, #22319, #26575, .T. ) ;
#35410 = EDGE_LOOP ( 'NONE', ( #1425, #17509, #25957, #27278 ) ) ;
#35411 = CARTESIAN_POINT ( 'NONE',  ( 793.5525998758768083, -271.0999726633344267, -372.6845335610516941 ) ) ;
#35412 = CARTESIAN_POINT ( 'NONE',  ( 786.2694204179717872, -141.2817908451530400, 305.1769319972829067 ) ) ;
#35414 = CARTESIAN_POINT ( 'NONE',  ( 778.1981804954714335, -274.2709662947833067, -314.8072714833589885 ) ) ;
#35413 = CARTESIAN_POINT ( 'NONE',  ( 911.9999999999993179, 154.9999999999998863, -360.0000000000000000 ) ) ;
#35415 = CARTESIAN_POINT ( 'NONE',  ( 795.9930595647434757, -411.0783235625954717, -320.7433823573372820 ) ) ;
#35416 = LINE ( 'NONE', #16740, #7558 ) ;
#35417 = CARTESIAN_POINT ( 'NONE',  ( 757.0176451133909268, -133.0999726633348246, -349.9200121543848354 ) ) ;
#35418 = DIRECTION ( 'NONE',  ( -0.000000000000000000, 1.000000000000000000, -0.000000000000000000 ) ) ;
#35419 = CARTESIAN_POINT ( 'NONE',  ( 798.0661480581538854, -2.532869017142183932, -309.5768839229118043 ) ) ;
#35420 = CARTESIAN_POINT ( 'NONE',  ( 746.8695393053151292, -317.9073299311467622, -327.6429770376306578 ) ) ;
#35421 = CARTESIAN_POINT ( 'NONE',  ( 772.4999999999993179, -462.9681489794448339, 370.0000000000000568 ) ) ;
#35422 = CARTESIAN_POINT ( 'NONE',  ( 795.1360043628807261, -20.08914811296592973, 360.2193346964456282 ) ) ;
#35423 = EDGE_CURVE ( 'NONE', #30052, #14449, #19655, .T. ) ;
#35424 = CARTESIAN_POINT ( 'NONE',  ( 812.3518521366052028, -265.0999726633344267, 326.5853460496235243 ) ) ;
#35425 = CARTESIAN_POINT ( 'NONE',  ( 756.1443688327750579, -189.6237781080507148, -314.3581564841659315 ) ) ;
#35426 = CARTESIAN_POINT ( 'NONE',  ( 814.5518280994195948, -207.7255117493289447, 332.4837098697145734 ) ) ;
#35427 = CARTESIAN_POINT ( 'NONE',  ( 762.1177392798416577, 5.445481882119263872, -309.8865473780659272 ) ) ;
#35428 = DIRECTION ( 'NONE',  ( 0.000000000000000000, 0.000000000000000000, 1.000000000000000000 ) ) ;
#35429 = EDGE_CURVE ( 'NONE', #11840, #3483, #3021, .T. ) ;
#35430 = CARTESIAN_POINT ( 'NONE',  ( 771.1735550268778070, -321.1800572038740142, 316.3353852180827630 ) ) ;
#35431 = CARTESIAN_POINT ( 'NONE',  ( 786.5483106153019435, -79.64542720878957027, 364.1601925771022366 ) ) ;
#35432 = CARTESIAN_POINT ( 'NONE',  ( 763.8424801807145741, -42.00906357242603661, 320.5453621957614700 ) ) ;
#35433 = CARTESIAN_POINT ( 'NONE',  ( 755.0488828828309806, 6.194403710130517382, -344.1219089521771934 ) ) ;
#35434 = PLANE ( 'NONE',  #32881 ) ;
#35435 = DIRECTION ( 'NONE',  ( -0.000000000000000000, 1.000000000000000000, -0.000000000000000000 ) ) ;
#35437 = CARTESIAN_POINT ( 'NONE',  ( 781.7834795799800531, -346.8164208402376971, 315.0636971347436202 ) ) ;
#35436 = CARTESIAN_POINT ( 'NONE',  ( 775.9200461376533440, -119.8055962898690865, 315.3028492785443291 ) ) ;
#35438 = ORIENTED_EDGE ( 'NONE', *, *, #35122, .T. ) ;
#35439 = ADVANCED_FACE ( 'NONE', ( #41145 ), #17330, .F. ) ;
#35440 = ADVANCED_FACE ( 'NONE', ( #41589 ), #2551, .T. ) ;
#35441 = CARTESIAN_POINT ( 'NONE',  ( 754.9735926884551418, -306.3510508353230648, -340.5236548041000333 ) ) ;
#35442 = CARTESIAN_POINT ( 'NONE',  ( 754.8072714833581358, -100.8164208402383792, 338.1981804954720587 ) ) ;
#35443 = CARTESIAN_POINT ( 'NONE',  ( 807.5423716828161105, -297.0783235625957559, -362.2119215644372048 ) ) ;
#35444 = CARTESIAN_POINT ( 'NONE',  ( 999.9999999999992042, 248.9999999999998863, -359.0000000000000000 ) ) ;
#35445 = CARTESIAN_POINT ( 'NONE',  ( 745.1769319972822814, -425.8055962898680491, 346.2694204179732083 ) ) ;
#35446 = ORIENTED_EDGE ( 'NONE', *, *, #26959, .F. ) ;
#35447 = CARTESIAN_POINT ( 'NONE',  ( 754.8072714833581358, -316.8164208402377540, 338.1981804954720587 ) ) ;
#35448 = CARTESIAN_POINT ( 'NONE',  ( 787.6308680596127942, -59.26014174441473870, -364.1105419155492768 ) ) ;
#35449 = CARTESIAN_POINT ( 'NONE',  ( 781.8018195045266339, -166.2709662947835909, -365.1927285166406705 ) ) ;
#35450 = CARTESIAN_POINT ( 'NONE',  ( 764.8639956371174549, -224.0891481129653187, -319.7806653035542013 ) ) ;
#35451 = CARTESIAN_POINT ( 'NONE',  ( 797.8594530101008786, -421.5436935675101040, 322.1405469898980982 ) ) ;
#35452 = CARTESIAN_POINT ( 'NONE',  ( 812.7932403749906598, -159.1800572038746111, -327.7687537140311633 ) ) ;
#35453 = EDGE_LOOP ( 'NONE', ( #38636, #21837, #28230, #23663 ) ) ;
#35454 = CARTESIAN_POINT ( 'NONE',  ( 771.2633955100217236, -143.9073299311473590, -363.4237431249939618 ) ) ;
#35455 = VERTEX_POINT ( 'NONE', #24473 ) ;
#35456 = CARTESIAN_POINT ( 'NONE',  ( 766.9102291470427417, -402.5545181178795247, -318.6633372737382501 ) ) ;
#35457 = CARTESIAN_POINT ( 'NONE',  ( 805.1927285166397041, -136.8164208402382371, 341.8018195045277707 ) ) ;
#35458 = CARTESIAN_POINT ( 'NONE',  ( 787.6308680596127942, -131.2601417444144829, 364.1105419155492768 ) ) ;
#35461 = CARTESIAN_POINT ( 'NONE',  ( 773.7943932421234194, -407.8055962898681628, 305.5313806188329409 ) ) ;
#35460 = CARTESIAN_POINT ( 'NONE',  ( 701.1634899080286232, 259.9999999999999432, -191.9749999999990848 ) ) ;
#35459 = CARTESIAN_POINT ( 'NONE',  ( 939.9999999999993179, -414.5899773927343404, -210.0000000000000000 ) ) ;
#35462 = EDGE_LOOP ( 'NONE', ( #29201, #25283, #16247, #39047 ) ) ;
#35463 = CARTESIAN_POINT ( 'NONE',  ( 805.2837595273609850, -410.7363362996976548, -340.5290396650784714 ) ) ;
#35464 = CARTESIAN_POINT ( 'NONE',  ( 911.9749999999993406, 154.9999999999998863, 339.9999999999999432 ) ) ;
#35465 = CARTESIAN_POINT ( 'NONE',  ( 750.9282345327678740, -160.9181544815165807, -319.8311093483690115 ) ) ;
#35466 = CARTESIAN_POINT ( 'NONE',  ( 757.7880784355613741, -42.00906357242603661, 312.4576283171834916 ) ) ;
#35468 = CARTESIAN_POINT ( 'NONE',  ( 939.9999999999992042, 74.99999999999984368, 350.0000000000000000 ) ) ;
#35467 = DIRECTION ( 'NONE',  ( 0.000000000000000000, 0.000000000000000000, -1.000000000000000000 ) ) ;
#35469 = CARTESIAN_POINT ( 'NONE',  ( 756.7813123517142913, -283.9874144716867477, -329.9779781133712504 ) ) ;
#35470 = CARTESIAN_POINT ( 'NONE',  ( 799.9999999999993179, -512.9681489794448908, 309.9999999999998863 ) ) ;
#35471 = CARTESIAN_POINT ( 'NONE',  ( 747.6481478633932056, -205.0999726633346256, -353.4146539503763620 ) ) ;
#35472 = DIRECTION ( 'NONE',  ( 0.000000000000000000, 1.000000000000000000, 0.000000000000000000 ) ) ;
#35473 = CARTESIAN_POINT ( 'NONE',  ( -26.63011601220122060, -512.9681489794448908, -339.9999999999999432 ) ) ;
#35474 = CARTESIAN_POINT ( 'NONE',  ( 802.9823548866075953, -361.0999726633341425, 330.0799878456151077 ) ) ;
#35475 = CARTESIAN_POINT ( 'NONE',  ( 749.5768839229115201, -348.5545181178796383, 358.0661480581553064 ) ) ;
#35476 = CARTESIAN_POINT ( 'NONE',  ( 812.7932403749906598, -207.1800572038744406, -327.7687537140311633 ) ) ;
#35477 = DIRECTION ( 'NONE',  ( 1.000000000000000000, -0.000000000000000000, -0.000000000000000000 ) ) ;
#35478 = CARTESIAN_POINT ( 'NONE',  ( 786.4999999999993179, -295.7697417039441916, 122.5118383533586837 ) ) ;
#35479 = ADVANCED_FACE ( 'NONE', ( #37664 ), #13199, .T. ) ;
#35480 = CARTESIAN_POINT ( 'NONE',  ( 762.1177392798416577, -162.5545181178802352, 309.8865473780659272 ) ) ;
#35481 = CARTESIAN_POINT ( 'NONE',  ( 795.6651683502461765, -106.7146871989600498, -371.3240766477733814 ) ) ;
#35482 = CARTESIAN_POINT ( 'NONE',  ( 751.9810565676468741, -122.0891481129656171, 360.9747183278973921 ) ) ;
#35483 = CARTESIAN_POINT ( 'NONE',  ( 777.4774526936600978, -322.2709662947830225, -304.7301800767027657 ) ) ;
#35484 = DIRECTION ( 'NONE',  ( -1.000000000000000000, 0.000000000000000000, 0.000000000000000000 ) ) ;
#35485 = PRODUCT_DEFINITION_SHAPE ( 'NONE', 'NONE',  #36333 ) ;
#35486 = FACE_OUTER_BOUND ( 'NONE', #2391, .T. ) ;
#35487 = CARTESIAN_POINT ( 'NONE',  ( 771.1735550268778070, -177.1800572038744690, 316.3353852180827630 ) ) ;
#35488 = CARTESIAN_POINT ( 'NONE',  ( 809.0717654672305343, -460.9181544815156713, 360.1688906516309885 ) ) ;
#35489 = CARTESIAN_POINT ( 'NONE',  ( 746.7653713866222915, -401.2601417444137155, -351.0478386215610271 ) ) ;
#35490 = CARTESIAN_POINT ( 'NONE',  ( 746.8695393053150156, -437.9073299311463074, -327.6429770376306010 ) ) ;
#35491 = CARTESIAN_POINT ( 'NONE',  ( 181.1634899080285948, 260.0000000000000000, -199.9999999999953957 ) ) ;
#35492 = CARTESIAN_POINT ( 'NONE',  ( 812.6845335610512393, -7.987414471687621642, 353.5525998758768651 ) ) ;
#35493 = ORIENTED_EDGE ( 'NONE', *, *, #8337, .T. ) ;
#35494 = ADVANCED_FACE ( 'NONE', ( #30742 ), #27277, .F. ) ;
#35495 = CARTESIAN_POINT ( 'NONE',  ( 810.1134526219336749, -200.5328690171415644, -357.8822607201570349 ) ) ;
#35496 = DIRECTION ( 'NONE',  ( 0.000000000000000000, 0.000000000000000000, -1.000000000000000000 ) ) ;
#35497 = CARTESIAN_POINT ( 'NONE',  ( 793.4146539503750546, -313.9874144716866908, 307.6481478633938877 ) ) ;
#35498 = CARTESIAN_POINT ( 'NONE',  ( 797.8594530101009923, -133.5436935675110419, 322.1405469898982119 ) ) ;
#35499 = EDGE_LOOP ( 'NONE', ( #41941, #44184 ) ) ;
#35500 = CARTESIAN_POINT ( 'NONE',  ( 764.8639956371174549, -296.0891481129650629, 319.7806653035542013 ) ) ;
#35501 = CARTESIAN_POINT ( 'NONE',  ( 813.1304606946830518, -41.90732993114767169, -352.3570229623690580 ) ) ;
#35502 = CARTESIAN_POINT ( 'NONE',  ( 767.7687537140311633, -71.90732993114760063, 372.7932403749916830 ) ) ;
#35503 = VERTEX_POINT ( 'NONE', #41370 ) ;
#35504 = CARTESIAN_POINT ( 'NONE',  ( 810.4231160770870019, -432.5545181178793541, -321.9338519418446936 ) ) ;
#35505 = EDGE_LOOP ( 'NONE', ( #19109, #9682, #1201, #28468 ) ) ;
#35506 = APPLICATION_PROTOCOL_DEFINITION ( 'draft international standard', 'automotive_design', 1998, #7222 ) ;
#35507 = CARTESIAN_POINT ( 'NONE',  ( 781.7834795799800531, -34.81642084023861372, 315.0636971347436202 ) ) ;
#35508 = CARTESIAN_POINT ( 'NONE',  ( 759.9864689768902508, -290.0891481129650629, -354.9819416627836404 ) ) ;
#35510 = CARTESIAN_POINT ( 'NONE',  ( 810.1134526219336749, -272.5328690171413086, 357.8822607201570349 ) ) ;
#35509 = CARTESIAN_POINT ( 'NONE',  ( 747.2067596250078623, -387.1800572038738437, 352.2312462859687230 ) ) ;
#35511 = CARTESIAN_POINT ( 'NONE',  ( 744.9990715423526808, -66.35105083532378956, 341.2370466360926002 ) ) ;
#35512 = CARTESIAN_POINT ( 'NONE',  ( 780.5236548040995785, -284.7363362996979390, -314.9735926884559944 ) ) ;
#35513 = CARTESIAN_POINT ( 'NONE',  ( 803.6646147819161570, -257.9073299311469896, -348.8264449731210561 ) ) ;
#35514 = DIRECTION ( 'NONE',  ( 1.000000000000000000, 0.000000000000000000, 0.000000000000000000 ) ) ;
#35515 = CARTESIAN_POINT ( 'NONE',  ( 767.8955696845333705, -120.4527844766019484, -362.1676090361162323 ) ) ;
#35516 = DIRECTION ( 'NONE',  ( -1.000000000000000000, -0.000000000000000000, 0.000000000000000000 ) ) ;
#35517 = CARTESIAN_POINT ( 'NONE',  ( 792.3570229623688874, -405.1800572038737300, 373.1304606946836202 ) ) ;
#35519 = CARTESIAN_POINT ( 'NONE',  ( 187.1337867209877857, 62.79977829742938411, 207.3621835540872951 ) ) ;
#35518 = DIRECTION ( 'NONE',  ( 0.000000000000000000, 0.000000000000000000, -1.000000000000000000 ) ) ;
#35520 = CARTESIAN_POINT ( 'NONE',  ( 754.3581564841646241, -65.46360902697142592, -316.1443688327762516 ) ) ;
#35521 = FACE_OUTER_BOUND ( 'NONE', #6586, .T. ) ;
#35522 = DIRECTION ( 'NONE',  ( -1.000000000000000000, 0.000000000000000000, 0.000000000000000000 ) ) ;
#35523 = CARTESIAN_POINT ( 'NONE',  ( 757.0176451133909268, -253.0999726633345119, 349.9200121543848354 ) ) ;
#35524 = CARTESIAN_POINT ( 'NONE',  ( 768.0187753319979720, -152.6346026584200786, 318.0580252608186242 ) ) ;
#35525 = ORIENTED_EDGE ( 'NONE', *, *, #1802, .T. ) ;
#35526 = CARTESIAN_POINT ( 'NONE',  ( 780.5236548040995785, -44.73633629969875614, -314.9735926884559944 ) ) ;
#35527 = AXIS2_PLACEMENT_3D ( 'NONE', #27513, #3041, #13671 ) ;
#35528 = CARTESIAN_POINT ( 'NONE',  ( 747.2067596250078623, -99.18005720387478164, -352.2312462859687230 ) ) ;
#35529 = CARTESIAN_POINT ( 'NONE',  ( 760.5453621957607311, -309.0783235625957559, 323.8424801807151425 ) ) ;
#35530 = CARTESIAN_POINT ( 'NONE',  ( 799.9999999999993179, 205.0000000000000568, -339.9999999999999432 ) ) ;
#35531 = CARTESIAN_POINT ( 'NONE',  ( 747.6481478633932056, -37.09997266333514432, 353.4146539503763620 ) ) ;
#35532 = VECTOR ( 'NONE', #6632, 1000.000000000000000 ) ;
#35533 = CARTESIAN_POINT ( 'NONE',  ( 745.4481719005789273, -219.7255117493289447, -347.5162901302853129 ) ) ;
#35534 = CARTESIAN_POINT ( 'NONE',  ( 792.3570229623688874, -213.1800572038743553, 373.1304606946836202 ) ) ;
#35535 = CARTESIAN_POINT ( 'NONE',  ( 804.4286716492782716, -89.36187538569299704, 345.3141322388244703 ) ) ;
#35536 = DIRECTION ( 'NONE',  ( -1.000000000000000000, -0.000000000000000000, 0.000000000000000000 ) ) ;
#35537 = CARTESIAN_POINT ( 'NONE',  ( 793.4146539503750546, -313.9874144716866908, -307.6481478633938877 ) ) ;
#35538 = CARTESIAN_POINT ( 'NONE',  ( 757.7880784355613741, -450.0090635724248500, 312.4576283171834916 ) ) ;
#35539 = CARTESIAN_POINT ( 'NONE',  ( 796.9462024416508257, -300.4527844766012663, -308.9653473494370246 ) ) ;
#35540 = DIRECTION ( 'NONE',  ( -0.000000000000000000, -1.000000000000000000, -0.000000000000000000 ) ) ;
#35541 = CARTESIAN_POINT ( 'NONE',  ( 755.0488828828309806, -353.8055962898683333, 344.1219089521771934 ) ) ;
#35542 = CARTESIAN_POINT ( 'NONE',  ( 772.5602148656447525, -57.72551174932945628, 305.7998596910095443 ) ) ;
#35543 = CARTESIAN_POINT ( 'NONE',  ( 795.1360043628807261, -380.0891481129646650, -360.2193346964456282 ) ) ;
#35544 = CARTESIAN_POINT ( 'NONE',  ( 756.7813123517142913, -67.98741447168742980, 329.9779781133712504 ) ) ;
#35545 = CARTESIAN_POINT ( 'NONE',  ( 745.1769319972822814, -89.80559628986918597, -346.2694204179732083 ) ) ;
#35546 = CARTESIAN_POINT ( 'NONE',  ( 778.7502325331095108, -192.3510508353233774, 304.6391490659818828 ) ) ;
#35547 = CARTESIAN_POINT ( 'NONE',  ( 768.0187753319979720, -32.63460265842044095, 318.0580252608186242 ) ) ;
#35548 = VERTEX_POINT ( 'NONE', #24252 ) ;
#35549 = CARTESIAN_POINT ( 'NONE',  ( 755.8398074228967971, -187.4419599262325278, -333.4516893846970333 ) ) ;
#35550 = CARTESIAN_POINT ( 'NONE',  ( 800.2193346964447755, -210.9982390220561967, 355.1360043628815788 ) ) ;
#35551 = CARTESIAN_POINT ( 'NONE',  ( 746.0683387631852383, -19.44195992623303937, -331.3260364891676204 ) ) ;
#35552 = CARTESIAN_POINT ( 'NONE',  ( 774.6858677611749044, -321.7255117493286320, 315.5713283507209894 ) ) ;
#35553 = CIRCLE ( 'NONE', #17134, 10.00000000000000888 ) ;
#35554 = CARTESIAN_POINT ( 'NONE',  ( 786.4999999999993179, -494.6608068873671300, -357.6536686473015720 ) ) ;
#35555 = LINE ( 'NONE', #18272, #21257 ) ;
#35556 = VERTEX_POINT ( 'NONE', #30969 ) ;
#35557 = CARTESIAN_POINT ( 'NONE',  ( 755.0488828828309806, -65.80559628986925702, 344.1219089521771934 ) ) ;
#35558 = CARTESIAN_POINT ( 'NONE',  ( 745.7194118038753459, -349.6454272087887603, -348.7631598425976449 ) ) ;
#35559 = CARTESIAN_POINT ( 'NONE',  ( 745.4481719005789273, -291.7255117493286320, 347.5162901302853697 ) ) ;
#35560 = CARTESIAN_POINT ( 'NONE',  ( 814.8230680027162407, -5.805596289869448867, 333.7305795820267917 ) ) ;
#35561 = CARTESIAN_POINT ( 'NONE',  ( 759.0159684113467620, -184.9181544815165239, -325.8855110935213020 ) ) ;
#35562 = CARTESIAN_POINT ( 'NONE',  ( 768.0187753319979720, -152.6346026584200786, -318.0580252608186242 ) ) ;
#35563 = CARTESIAN_POINT ( 'NONE',  ( 757.8323909638828582, -362.6346026584193964, -352.1044303154654358 ) ) ;
#35564 = EDGE_LOOP ( 'NONE', ( #10176, #13725, #45002, #12828 ) ) ;
#35565 = CARTESIAN_POINT ( 'NONE',  ( 814.9108240113580450, -280.2709662947833067, 337.5031285880265273 ) ) ;
#35566 = CYLINDRICAL_SURFACE ( 'NONE', #44712, 1.000000000000000888 ) ;
#35567 = CARTESIAN_POINT ( 'NONE',  ( 772.3691319403857278, -335.2601417444137724, 315.8894580844506663 ) ) ;
#35568 = CARTESIAN_POINT ( 'NONE',  ( 190.7583438952259485, 394.6698570112193920, -224.9999999999999716 ) ) ;
#35569 = CARTESIAN_POINT ( 'NONE',  ( 805.2837595273609850, -170.7363362996983938, 340.5290396650784714 ) ) ;
#35570 = CARTESIAN_POINT ( 'NONE',  ( 755.3201227861273992, -3.725511749329622813, 345.3687786644892981 ) ) ;
#35571 = ORIENTED_EDGE ( 'NONE', *, *, #27299, .T. ) ;
#35572 = CARTESIAN_POINT ( 'NONE',  ( 776.2046728542105711, -380.1908817542431507, -304.8212110874238761 ) ) ;
#35573 = AXIS2_PLACEMENT_3D ( 'NONE', #13108, #34097, #9633 ) ;
#35574 = CARTESIAN_POINT ( 'NONE',  ( 758.8095938919644823, 15.91085188703394593, -311.6929314249762797 ) ) ;
#35575 = CARTESIAN_POINT ( 'NONE',  ( 791.0478386215596629, -285.8272453906071178, 306.7653713866226326 ) ) ;
#35576 = CARTESIAN_POINT ( 'NONE',  ( 804.1601925771018387, -199.4419599262324709, 346.5483106153029098 ) ) ;
#35577 = CARTESIAN_POINT ( 'NONE',  ( 765.0180583372156207, -360.9982390220557704, -360.0135310231089534 ) ) ;
#35578 = CARTESIAN_POINT ( 'NONE',  ( 767.8955696845333705, -0.4527844766023628176, 362.1676090361162323 ) ) ;
#35579 = CARTESIAN_POINT ( 'NONE',  ( 786.4999999999993179, -494.6608068873671300, -357.6536686473015720 ) ) ;
#35580 = CARTESIAN_POINT ( 'NONE',  ( 804.1105419155481968, -219.8272453906073167, -347.6308680596136469 ) ) ;
#35581 = CARTESIAN_POINT ( 'NONE',  ( 777.5031285880264704, -22.81642084023865280, 374.9108240113588408 ) ) ;
#35582 = CARTESIAN_POINT ( 'NONE',  ( 812.7932403749906598, -87.18005720387481006, 327.7687537140311633 ) ) ;
#35583 = AXIS2_PLACEMENT_3D ( 'NONE', #41909, #6786, #20862 ) ;
#35584 = CARTESIAN_POINT ( 'NONE',  ( -199.6009925648704098, 290.0000000000001137, -274.9999999999999432 ) ) ;
#35585 = CARTESIAN_POINT ( 'NONE',  ( 767.7687537140311633, -431.9073299311464211, -372.7932403749916830 ) ) ;
#35586 = EDGE_CURVE ( 'NONE', #45239, #27745, #6014, .T. ) ;
#35587 = DIRECTION ( 'NONE',  ( 0.000000000000000000, 0.000000000000000000, 1.000000000000000000 ) ) ;
#35588 = CARTESIAN_POINT ( 'NONE',  ( 752.7379699480933368, -372.0090635724250205, 361.9858362298580232 ) ) ;
#35589 = LINE ( 'NONE', #3965, #33106 ) ;
#35590 = CARTESIAN_POINT ( 'NONE',  ( 805.0032342141412300, -325.5436935675105019, 314.9967657858571783 ) ) ;
#35591 = CARTESIAN_POINT ( 'NONE',  ( 804.7487373415286811, -67.54369356751125508, -364.7487373415288516 ) ) ;
#35592 = CARTESIAN_POINT ( 'NONE',  ( 757.8323909638827445, -290.6346026584195101, -352.1044303154654358 ) ) ;
#35593 = CARTESIAN_POINT ( 'NONE',  ( 9.202092513630239068E-14, 199.9999999999999147, 0.000000000000000000 ) ) ;
#35594 = CARTESIAN_POINT ( 'NONE',  ( 755.0636971347428243, -436.2709662947827951, 341.7834795799807353 ) ) ;
#35595 = CARTESIAN_POINT ( 'NONE',  ( 772.4468031744293057, -201.8272453906073451, 363.8651313633793620 ) ) ;
#35596 = CARTESIAN_POINT ( 'NONE',  ( 781.2370466360911223, -68.73633629969867798, -304.9990715423533629 ) ) ;
#35597 = CARTESIAN_POINT ( 'NONE',  ( 775.9200461376533440, -71.80559628986922860, -315.3028492785443291 ) ) ;
#35598 = CARTESIAN_POINT ( 'NONE',  ( 786.2056067578752163, -83.80559628986920018, 374.4686193811670023 ) ) ;
#35599 = CARTESIAN_POINT ( 'NONE',  ( 758.0580252608178853, -414.4527844766010389, 328.0187753319985404 ) ) ;
#35600 =( BOUNDED_CURVE ( )  B_SPLINE_CURVE ( 3, ( #30828, #44921, #24108, #27356 ),
 .UNSPECIFIED., .F., .T. ) 
 B_SPLINE_CURVE_WITH_KNOTS ( ( 4, 4 ),
 ( 0.000000000000000000, 1.570796326794896558 ),
 .UNSPECIFIED. ) 
 CURVE ( )  GEOMETRIC_REPRESENTATION_ITEM ( )  RATIONAL_B_SPLINE_CURVE ( ( 1.000000000000000000, 0.8047378541243649375, 0.8047378541243649375, 1.000000000000000000 ) ) 
 REPRESENTATION_ITEM ( '' )  );
#35601 = CARTESIAN_POINT ( 'NONE',  ( 759.9864689768902508, -2.089148112965993231, -354.9819416627836404 ) ) ;
#35603 = ORIENTED_EDGE ( 'NONE', *, *, #13412, .F. ) ;
#35602 = CARTESIAN_POINT ( 'NONE',  ( 786.6156483768007774, -97.44195992623281199, -315.5913626894246136 ) ) ;
#35604 = CARTESIAN_POINT ( 'NONE',  ( 754.8072714833581358, -100.8164208402383792, -338.1981804954720587 ) ) ;
#35605 = CARTESIAN_POINT ( 'NONE',  ( 790.8726784830453198, -394.7146871989591546, -362.5472867521010585 ) ) ;
#35606 = EDGE_CURVE ( 'NONE', #37078, #22109, #36038, .T. ) ;
#35608 = CARTESIAN_POINT ( 'NONE',  ( 767.8955696845334842, -240.4527844766015789, 362.1676090361161755 ) ) ;
#35607 = CARTESIAN_POINT ( 'NONE',  ( 762.1405469898971887, -217.5436935675107293, 357.8594530101015607 ) ) ;
#35609 = AXIS2_PLACEMENT_3D ( 'NONE', #35473, #3152, #27876 ) ;
#35610 = CARTESIAN_POINT ( 'NONE',  ( 813.9316612368132837, -415.4419599262318457, -348.6739635108323228 ) ) ;
#35611 = CARTESIAN_POINT ( 'NONE',  ( 51.16348990802859475, 260.0000000000000568, -202.7499999999943441 ) ) ;
#35612 = ORIENTED_EDGE ( 'NONE', *, *, #19626, .F. ) ;
#35613 = CARTESIAN_POINT ( 'NONE',  ( 774.6858677611749044, -417.7255117493283478, 315.5713283507209894 ) ) ;
#35614 = AXIS2_PLACEMENT_3D ( 'NONE', #26365, #9502, #12058 ) ;
#35615 = VERTEX_POINT ( 'NONE', #34877 ) ;
#35616 =( NAMED_UNIT ( * ) SI_UNIT ( $, .STERADIAN. ) SOLID_ANGLE_UNIT ( ) );
#35617 = CARTESIAN_POINT ( 'NONE',  ( 763.0537975583475827, -240.4527844766015221, -371.0346526505627480 ) ) ;
#35618 = CARTESIAN_POINT ( 'NONE',  ( 782.4968714119720516, -154.8164208402382371, 305.0891759886411023 ) ) ;
#35619 = CARTESIAN_POINT ( 'NONE',  ( 758.4439275373578084, -276.5545181178798657, 353.2243759319684386 ) ) ;
#35620 = ORIENTED_EDGE ( 'NONE', *, *, #36196, .T. ) ;
#35621 = CARTESIAN_POINT ( 'NONE',  ( 783.0745993439762742, -56.19088175424417386, -365.1016975059196739 ) ) ;
#35622 = CARTESIAN_POINT ( 'NONE',  ( 771.2633955100217236, -263.9073299311469327, -363.4237431249939618 ) ) ;
#35623 = EDGE_LOOP ( 'NONE', ( #20622, #10334, #11092, #38764, #45206, #43076 ) ) ;
#35624 = CARTESIAN_POINT ( 'NONE',  ( 802.1676090361156639, -350.6346026584192828, -327.8955696845344505 ) ) ;
#35625 = CARTESIAN_POINT ( 'NONE',  ( 757.8323909638827445, -2.634602658420536869, -352.1044303154654358 ) ) ;
#35626 = CARTESIAN_POINT ( 'NONE',  ( 764.0069404352550464, -231.0783235625960401, 359.2566176426627180 ) ) ;
#35627 = CARTESIAN_POINT ( 'NONE',  ( 571.1634899080285095, 259.9999999999999432, -202.7499999999980105 ) ) ;
#35628 = DIRECTION ( 'NONE',  ( 0.000000000000000000, -1.000000000000000000, -4.857225732735055920E-15 ) ) ;
#35629 = EDGE_CURVE ( 'NONE', #19659, #12114, #38136, .T. ) ;
#35630 = ORIENTED_EDGE ( 'NONE', *, *, #45636, .F. ) ;
#35631 = CARTESIAN_POINT ( 'NONE',  ( 802.1676090361156639, -14.63460265842049424, -327.8955696845344505 ) ) ;
#35632 = DIRECTION ( 'NONE',  ( -0.000000000000000000, 1.000000000000000000, -0.000000000000000000 ) ) ;
#35633 = CARTESIAN_POINT ( 'NONE',  ( -78.83651009197140525, 240.0000000000000853, -199.9999999999936051 ) ) ;
#35634 = ORIENTED_EDGE ( 'NONE', *, *, #25229, .F. ) ;
#35635 = CARTESIAN_POINT ( 'NONE',  ( 781.2370466360911223, -284.7363362996979390, -304.9990715423533629 ) ) ;
#35636 = CARTESIAN_POINT ( 'NONE',  ( 793.5525998758768083, -127.0999726633348672, 372.6845335610516941 ) ) ;
#35638 = CARTESIAN_POINT ( 'NONE',  ( 762.1405469898971887, -241.5436935675106156, -357.8594530101015607 ) ) ;
#35637 = LINE ( 'NONE', #39823, #18731 ) ;
#35639 = CARTESIAN_POINT ( 'NONE',  ( 577.2824899080285377, 256.4999999999999432, -199.9999999999981526 ) ) ;
#35640 = CARTESIAN_POINT ( 'NONE',  ( 793.0897708529556667, -102.5545181178804057, -361.3366627262616362 ) ) ;
#35641 = EDGE_CURVE ( 'NONE', #13352, #28228, #34180, .T. ) ;
#35642 = CARTESIAN_POINT ( 'NONE',  ( 771.3260364891663130, -379.6454272087886466, 306.0683387631859773 ) ) ;
#35643 = VECTOR ( 'NONE', #41680, 1000.000000000000000 ) ;
#35644 = FACE_OUTER_BOUND ( 'NONE', #40847, .T. ) ;
#35645 = CARTESIAN_POINT ( 'NONE',  ( 811.6461892240364477, 19.28531280103956647, -324.1737431748509835 ) ) ;
#35646 = CARTESIAN_POINT ( 'NONE',  ( 777.4774526936600978, -298.2709662947831930, -304.7301800767028226 ) ) ;
#35647 = DIRECTION ( 'NONE',  ( -0.000000000000000000, 1.000000000000000000, -0.000000000000000000 ) ) ;
#35648 = CARTESIAN_POINT ( 'NONE',  ( 802.1676090361156639, -14.63460265842049424, 327.8955696845344505 ) ) ;
#35649 = VECTOR ( 'NONE', #28614, 1000.000000000000000 ) ;
#35650 = CARTESIAN_POINT ( 'NONE',  ( 799.9636004259356241, -238.9181544815163534, 311.2241431872006956 ) ) ;
#35651 = CARTESIAN_POINT ( 'NONE',  ( 751.2241431872005251, -208.1692326535051905, -359.9636004259367610 ) ) ;
#35652 = CARTESIAN_POINT ( 'NONE',  ( 804.7487373415286811, -235.5436935675107293, 364.7487373415288516 ) ) ;
#35653 = CARTESIAN_POINT ( 'NONE',  ( 777.5031285880264704, -430.8164208402374129, -374.9108240113588408 ) ) ;
#35654 = CARTESIAN_POINT ( 'NONE',  ( 799.9999999999993179, -512.9681489794448908, 339.9999999999999432 ) ) ;
#35655 = CARTESIAN_POINT ( 'NONE',  ( 804.6798772138708955, -327.7255117493285184, 334.6312213355107019 ) ) ;
#35656 = CARTESIAN_POINT ( 'NONE',  ( 786.5483106153019435, -103.6454272087894850, 364.1601925771022366 ) ) ;
#35657 = CARTESIAN_POINT ( 'NONE',  ( 783.0745993439762742, -80.19088175424411702, 365.1016975059196739 ) ) ;
#35658 = CARTESIAN_POINT ( 'NONE',  ( 769.1273215169530886, 25.28531280103955226, -317.4527132478988847 ) ) ;
#35659 = DIRECTION ( 'NONE',  ( -1.000000000000000000, 0.000000000000000000, 0.000000000000000000 ) ) ;
#35661 = ADVANCED_FACE ( 'NONE', ( #9497 ), #16658, .F. ) ;
#35660 = DIRECTION ( 'NONE',  ( -0.000000000000000000, 1.000000000000000000, -0.000000000000000000 ) ) ;
#35663 = CARTESIAN_POINT ( 'NONE',  ( 797.8594530101008786, -349.5436935675102745, 322.1405469898980982 ) ) ;
#35662 = CARTESIAN_POINT ( 'NONE',  ( 756.1348686366196716, -161.2601417444143976, 347.5531968255698416 ) ) ;
#35664 = ORIENTED_EDGE ( 'NONE', *, *, #9997, .F. ) ;
#35665 = CARTESIAN_POINT ( 'NONE',  ( 764.0069404352550464, -279.0783235625958127, -359.2566176426627180 ) ) ;
#35666 = CARTESIAN_POINT ( 'NONE',  ( 778.2165204200184689, -118.8164208402383508, 364.9363028652563230 ) ) ;
#35667 = CARTESIAN_POINT ( 'NONE',  ( 786.2056067578752163, -299.8055962898685038, -374.4686193811670023 ) ) ;
#35668 = CARTESIAN_POINT ( 'NONE',  ( -468.8365100919714337, 230.0000000000001421, -199.9999999999908766 ) ) ;
#35669 = CARTESIAN_POINT ( 'NONE',  ( 756.1443688327750579, -429.6237781080499190, 314.3581564841659315 ) ) ;
#35670 = ORIENTED_EDGE ( 'NONE', *, *, #1561, .T. ) ;
#35671 = CARTESIAN_POINT ( 'NONE',  ( 755.0636971347428243, -316.2709662947832499, 341.7834795799807353 ) ) ;
#35672 = CARTESIAN_POINT ( 'NONE',  ( 765.8855110935204493, -94.16923265350555994, -319.0159684113471599 ) ) ;
#35673 = CARTESIAN_POINT ( 'NONE',  ( 774.6858677611749044, -153.7255117493291721, -315.5713283507209894 ) ) ;
#35674 = CARTESIAN_POINT ( 'NONE',  ( 778.1981804954714335, -202.2709662947834772, -314.8072714833589885 ) ) ;
#35675 = CARTESIAN_POINT ( 'NONE',  ( 778.2165204200184689, -430.8164208402374129, 364.9363028652563230 ) ) ;
#35676 = CARTESIAN_POINT ( 'NONE',  ( 792.3570229623688874, -141.1800572038746395, -373.1304606946836202 ) ) ;
#35677 = ORIENTED_EDGE ( 'NONE', *, *, #42760, .T. ) ;
#35678 = CIRCLE ( 'NONE', #36444, 20.00000000000001776 ) ;
#35679 = CARTESIAN_POINT ( 'NONE',  ( 764.8639956371174549, -152.0891481129655460, -319.7806653035542581 ) ) ;
#35680 = AXIS2_PLACEMENT_3D ( 'NONE', #7492, #35647, #12318 ) ;
#35681 = ORIENTED_EDGE ( 'NONE', *, *, #29360, .F. ) ;
#35682 = CARTESIAN_POINT ( 'NONE',  ( 793.9708237608222134, -382.9181544815159555, -319.2295555964448681 ) ) ;
#35683 = EDGE_CURVE ( 'NONE', #22016, #7575, #45525, .T. ) ;
#35684 = CARTESIAN_POINT ( 'NONE',  ( 784.1219089521767955, -453.2817908451519315, 315.0488828828318333 ) ) ;
#35685 = CARTESIAN_POINT ( 'NONE',  ( 764.0069404352550464, -111.0783235625964096, 359.2566176426627180 ) ) ;
#35688 = CARTESIAN_POINT ( 'NONE',  ( 810.1134526219336749, -392.5328690171409107, 357.8822607201570349 ) ) ;
#35687 = CARTESIAN_POINT ( 'NONE',  ( -190.7583438952259485, 394.6698570112193920, -274.9999999999999432 ) ) ;
#35686 = DIRECTION ( 'NONE',  ( -0.000000000000000000, 1.000000000000000000, -0.000000000000000000 ) ) ;
#35689 = EDGE_CURVE ( 'NONE', #21525, #8915, #45066, .T. ) ;
#35690 = ORIENTED_EDGE ( 'NONE', *, *, #37965, .F. ) ;
#35691 = CARTESIAN_POINT ( 'NONE',  ( 798.5707757039680246, -389.4636090269704027, -356.7845633553585003 ) ) ;
#35692 = CARTESIAN_POINT ( 'NONE',  ( 928.0249999999991815, 219.9999999999998863, 360.0000000000000000 ) ) ;
#35693 = CARTESIAN_POINT ( 'NONE',  ( 768.9521613784389729, -177.8272453906074304, -373.2346286133773106 ) ) ;
#35694 = CARTESIAN_POINT ( 'NONE',  ( 814.8207195650702488, -26.19088175424427334, 336.2433038121456548 ) ) ;
#35695 = VECTOR ( 'NONE', #31941, 1000.000000000000114 ) ;
#35697 = DIRECTION ( 'NONE',  ( -0.000000000000000000, -0.000000000000000000, 1.000000000000000000 ) ) ;
#35696 = CYLINDRICAL_SURFACE ( 'NONE', #14561, 2.749999999999835687 ) ;
#35698 = CARTESIAN_POINT ( 'NONE',  ( 755.8398074228967971, -283.4419599262321867, -333.4516893846970333 ) ) ;
#35699 = DIRECTION ( 'NONE',  ( 0.000000000000000000, 0.7651688349527167032, 0.6438296778008156807 ) ) ;
#35700 = CARTESIAN_POINT ( 'NONE',  ( 807.2620300519052989, -192.0090635724255606, -318.0141637701419768 ) ) ;
#35701 = DIRECTION ( 'NONE',  ( 1.000000000000000000, 0.000000000000000000, 0.000000000000000000 ) ) ;
#35703 = ADVANCED_FACE ( 'NONE', ( #33965 ), #13421, .F. ) ;
#35702 = CARTESIAN_POINT ( 'NONE',  ( 939.9999999999993179, -190.2822455671962985, -69.00746428064724114 ) ) ;
#35704 = EDGE_CURVE ( 'NONE', #41166, #30229, #14655, .T. ) ;
#35705 = CARTESIAN_POINT ( 'NONE',  ( 773.4516893846965786, -379.6454272087886466, 315.8398074228977066 ) ) ;
#35706 = CARTESIAN_POINT ( 'NONE',  ( 748.6759233522253680, -328.3726999360615650, 324.3348316497537098 ) ) ;
#35707 = CARTESIAN_POINT ( 'NONE',  ( 758.8095938919644823, -224.0891481129652902, -311.6929314249762797 ) ) ;
#35708 = DIRECTION ( 'NONE',  ( 0.000000000000000000, -1.000000000000000000, 0.000000000000000000 ) ) ;
#35709 = CARTESIAN_POINT ( 'NONE',  ( 802.1676090361156639, 9.365397341579420498, -327.8955696845344505 ) ) ;
#35710 = CARTESIAN_POINT ( 'NONE',  ( 750.9282345327678740, -136.9181544815166376, 319.8311093483690115 ) ) ;
#35711 = CARTESIAN_POINT ( 'NONE',  ( 786.2056067578752163, -83.80559628986920018, -374.4686193811670023 ) ) ;
#35712 = CARTESIAN_POINT ( 'NONE',  ( 792.2312462859673587, -107.9073299311474727, 307.2067596250082602 ) ) ;
#35713 = CARTESIAN_POINT ( 'NONE',  ( 787.5162901302840055, -323.3618753856923149, -305.4481719005792684 ) ) ;
#35714 = LINE ( 'NONE', #14031, #41269 ) ;
#35715 = CARTESIAN_POINT ( 'NONE',  ( 8.295132257852724189E-14, 199.9999999999999147, 350.0000000000000000 ) ) ;
#35716 = CARTESIAN_POINT ( 'NONE',  ( 795.1360043628807261, -212.0891481129652902, 360.2193346964456282 ) ) ;
#35717 = CIRCLE ( 'NONE', #8425, 2.749999999999835687 ) ;
#35718 =( GEOMETRIC_REPRESENTATION_CONTEXT ( 3 ) GLOBAL_UNCERTAINTY_ASSIGNED_CONTEXT ( ( #24248 ) ) GLOBAL_UNIT_ASSIGNED_CONTEXT ( ( #37231, #33321, #19454 ) ) REPRESENTATION_CONTEXT ( 'NONE', 'WORKASPACE' ) );
#35719 = CARTESIAN_POINT ( 'NONE',  ( 761.4292242960306112, 6.536390973028352924, 323.2154366446414429 ) ) ;
#35720 = ADVANCED_FACE ( 'NONE', ( #38360 ), #6706, .F. ) ;
#35721 = CARTESIAN_POINT ( 'NONE',  ( 773.7943932421234194, -407.8055962898681628, -305.5313806188329409 ) ) ;
#35722 = CARTESIAN_POINT ( 'NONE',  ( 804.7487373415286811, -427.5436935675101040, -364.7487373415288516 ) ) ;
#35724 = EDGE_CURVE ( 'NONE', #11197, #36800, #36563, .T. ) ;
#35723 = CARTESIAN_POINT ( 'NONE',  ( 919.9999999999993179, 219.9999999999998863, -350.0000000000000000 ) ) ;
#35725 = CARTESIAN_POINT ( 'NONE',  ( 746.7653713866222915, 6.739858255585061464, 351.0478386215610271 ) ) ;
#35726 = VERTEX_POINT ( 'NONE', #18025 ) ;
#35727 = CARTESIAN_POINT ( 'NONE',  ( 764.8639956371174549, -8.089148112965974136, 319.7806653035542013 ) ) ;
#35728 = CARTESIAN_POINT ( 'NONE',  ( 808.7758568127978833, -196.1692326535052473, -320.0363995740631822 ) ) ;
#35729 = CARTESIAN_POINT ( 'NONE',  ( 999.9999999999992042, 248.9999999999998863, 359.0000000000000000 ) ) ;
#35730 = CARTESIAN_POINT ( 'NONE',  ( 756.1443688327750579, -309.6237781080502600, 314.3581564841659315 ) ) ;
#35731 = CARTESIAN_POINT ( 'NONE',  ( 755.3201227861273992, -147.7255117493291721, 345.3687786644892981 ) ) ;
#35732 = ORIENTED_EDGE ( 'NONE', *, *, #34285, .T. ) ;
#35733 = VECTOR ( 'NONE', #13586, 1000.000000000000000 ) ;
#35734 = CARTESIAN_POINT ( 'NONE',  ( 788.8264449731200330, -309.1800572038740711, 363.6646147819171233 ) ) ;
#35735 = AXIS2_PLACEMENT_3D ( 'NONE', #16980, #41694, #31285 ) ;
#35736 = CARTESIAN_POINT ( 'NONE',  ( 801.1904061080336987, -44.08914811296584446, -368.3070685750235498 ) ) ;
#35737 = CARTESIAN_POINT ( 'NONE',  ( 782.4968714119720516, -82.81642084023846451, 305.0891759886411023 ) ) ;
#35738 = VERTEX_POINT ( 'NONE', #21016 ) ;
#35739 = CARTESIAN_POINT ( 'NONE',  ( 797.8822607201568644, -462.5545181178792973, -370.1134526219340160 ) ) ;
#35740 = ORIENTED_EDGE ( 'NONE', *, *, #24640, .F. ) ;
#35741 = PRODUCT_CONTEXT ( 'NONE', #23707, 'mechanical' ) ;
#35742 = EDGE_CURVE ( 'NONE', #19577, #2495, #11, .T. ) ;
#35744 = CARTESIAN_POINT ( 'NONE',  ( 760.7433823573367135, -324.0090635724251911, 355.9930595647440441 ) ) ;
#35743 = CARTESIAN_POINT ( 'NONE',  ( 803.6646147819161570, -65.90732993114758642, 348.8264449731210561 ) ) ;
#35745 = CARTESIAN_POINT ( 'NONE',  ( 804.6798772138708955, -303.7255117493287457, -334.6312213355107019 ) ) ;
#35747 = CARTESIAN_POINT ( 'NONE',  ( 800.1688906516307043, -298.1692326535049347, 369.0717654672308186 ) ) ;
#35746 = CARTESIAN_POINT ( 'NONE',  ( 745.4481719005789273, -387.7255117493284047, 347.5162901302853697 ) ) ;
#35748 = EDGE_CURVE ( 'NONE', #19255, #28334, #42268, .T. ) ;
#35749 = AXIS2_PLACEMENT_3D ( 'NONE', #16454, #26400, #6053 ) ;
#35750 = CARTESIAN_POINT ( 'NONE',  ( 786.2056067578752163, -59.80559628986927834, 374.4686193811670023 ) ) ;
#35751 = CARTESIAN_POINT ( 'NONE',  ( 790.0220218866281812, -295.0999726633343698, -363.2186876482849129 ) ) ;
#35752 = CARTESIAN_POINT ( 'NONE',  ( 758.0580252608178853, -294.4527844766013800, -328.0187753319985404 ) ) ;
#35753 = CARTESIAN_POINT ( 'NONE',  ( 758.0580252608178853, -438.4527844766009821, -328.0187753319985404 ) ) ;
#35754 = CARTESIAN_POINT ( 'NONE',  ( 764.8639956371174549, -104.0891481129656881, -319.7806653035542013 ) ) ;
#35755 = CIRCLE ( 'NONE', #42411, 30.00000000000002842 ) ;
#35756 = DIRECTION ( 'NONE',  ( 0.000000000000000000, 1.000000000000000000, 0.000000000000000000 ) ) ;
#35757 = CARTESIAN_POINT ( 'NONE',  ( 759.0252816721024374, -384.9982390220556567, 368.0189434323527280 ) ) ;
#35759 = CARTESIAN_POINT ( 'NONE',  ( -190.7583438952258916, 294.6698570112193920, -274.9999999999999432 ) ) ;
#35758 = CARTESIAN_POINT ( 'NONE',  ( 187.1337867209877857, 62.79977829742938411, -207.3621835540872951 ) ) ;
#35760 = CARTESIAN_POINT ( 'NONE',  ( 755.8990559732751535, -83.46360902697136908, -365.9055244015606831 ) ) ;
#35761 = CARTESIAN_POINT ( 'NONE',  ( 959.5497976682736407, 120.6654763175833693, 350.0000000000000000 ) ) ;
#35762 = LINE ( 'NONE', #21670, #36414 ) ;
#35763 = CARTESIAN_POINT ( 'NONE',  ( 786.5483106153019435, -247.6454272087890160, 364.1601925771022366 ) ) ;
#35764 = CARTESIAN_POINT ( 'NONE',  ( 755.5713283507202505, -149.3618753856928265, 334.6858677611754729 ) ) ;
#35765 = PRODUCT_RELATED_PRODUCT_CATEGORY ( 'part', '', ( #26963 ) ) ;
#35766 = VERTEX_POINT ( 'NONE', #14329 ) ;
#35767 = CARTESIAN_POINT ( 'NONE',  ( 761.4292242960306112, -41.46360902697149697, -323.2154366446414429 ) ) ;
#35768 = CARTESIAN_POINT ( 'NONE',  ( 815.2698199232962679, -88.81642084023843609, -342.5225473063383674 ) ) ;
#35769 = CARTESIAN_POINT ( 'NONE',  ( 804.1601925771018387, -343.4419599262320162, 346.5483106153029098 ) ) ;
#35770 = CARTESIAN_POINT ( 'NONE',  ( 769.9999999999992042, 178.9475563372491251, -320.0000000000000000 ) ) ;
#35771 = CARTESIAN_POINT ( 'NONE',  ( 786.2694204179717872, -45.28179084515329578, 305.1769319972829067 ) ) ;
#35772 = CARTESIAN_POINT ( 'NONE',  ( 745.7998596910086917, -221.3618753856925707, -332.5602148656461168 ) ) ;
#35773 = VECTOR ( 'NONE', #43947, 1000.000000000000000 ) ;
#35774 = AXIS2_PLACEMENT_3D ( 'NONE', #2019, #7657, #25428 ) ;
#35775 = CARTESIAN_POINT ( 'NONE',  ( 767.6429770376289525, -201.1800572038744690, 306.8695393053162093 ) ) ;
#35776 = CARTESIAN_POINT ( 'NONE',  ( 795.1360043628807261, -116.0891481129656029, 360.2193346964456282 ) ) ;
#35777 = FACE_OUTER_BOUND ( 'NONE', #39710, .T. ) ;
#35778 = CARTESIAN_POINT ( 'NONE',  ( 812.6845335610512393, -319.9874144716866340, -353.5525998758768651 ) ) ;
#35779 = CARTESIAN_POINT ( 'NONE',  ( 766.4474001241216001, -451.0999726633339151, 307.3154664389482491 ) ) ;
#35780 = CARTESIAN_POINT ( 'NONE',  ( 792.2312462859673587, -299.9073299311468759, -307.2067596250082602 ) ) ;
#35781 = DIRECTION ( 'NONE',  ( -1.000000000000000000, -0.000000000000000000, 0.000000000000000000 ) ) ;
#35782 = CARTESIAN_POINT ( 'NONE',  ( 779.4709603349208464, -360.3510508353228374, 314.7162404726379918 ) ) ;
#35783 = CARTESIAN_POINT ( 'NONE',  ( 814.5518280994195948, -63.72551174932941365, 332.4837098697145166 ) ) ;
#35784 = CARTESIAN_POINT ( 'NONE',  ( 767.8955696845333705, -432.4527844766008684, -362.1676090361162323 ) ) ;
#35785 = CARTESIAN_POINT ( 'NONE',  ( 784.0799538623451781, -59.80559628986927834, 364.6971507214555572 ) ) ;
#35786 = CARTESIAN_POINT ( 'NONE',  ( 774.6312213355099630, -191.3618753856925991, -364.6798772138717482 ) ) ;
#35787 = AXIS2_PLACEMENT_3D ( 'NONE', #42911, #32056, #195 ) ;
#35788 = CARTESIAN_POINT ( 'NONE',  ( 815.0009284576459549, -78.35105083532376113, -338.7629533639073429 ) ) ;
#35789 = CARTESIAN_POINT ( 'NONE',  ( 747.3154664389472828, -211.9874144716869750, 326.4474001241230781 ) ) ;
#35790 = CARTESIAN_POINT ( 'NONE',  ( 800.2193346964446619, -42.99823902205676518, 355.1360043628816925 ) ) ;
#35791 = VECTOR ( 'NONE', #5991, 1000.000000000000000 ) ;
#35792 = ORIENTED_EDGE ( 'NONE', *, *, #34453, .F. ) ;
#35793 = CARTESIAN_POINT ( 'NONE',  ( 796.7845633553578182, -201.6237781080506863, -358.5707757039688204 ) ) ;
#35794 = CARTESIAN_POINT ( 'NONE',  ( 800.0135310231082713, -206.0891481129653471, 325.0180583372163028 ) ) ;
#35795 = CARTESIAN_POINT ( 'NONE',  ( 759.8311093483677041, -22.16923265350575889, -310.9282345327691814 ) ) ;
#35796 = CARTESIAN_POINT ( 'NONE',  ( 755.3201227861273992, -339.7255117493285184, 345.3687786644892981 ) ) ;
#35797 = AXIS2_PLACEMENT_3D ( 'NONE', #15713, #26095, #5531 ) ;
#35798 = DIRECTION ( 'NONE',  ( 1.000000000000000000, 0.000000000000000000, 0.000000000000000000 ) ) ;
#35799 = DIRECTION ( 'NONE',  ( 0.000000000000000000, 0.000000000000000000, 1.000000000000000000 ) ) ;
#35800 = EDGE_LOOP ( 'NONE', ( #11319, #11674 ) ) ;
#35801 = CARTESIAN_POINT ( 'NONE',  ( 790.8726784830453198, -58.71468719896019905, 362.5472867521010585 ) ) ;
#35802 = CARTESIAN_POINT ( 'NONE',  ( 744.6391490659812007, -350.7363362996978253, -338.7502325331110455 ) ) ;
#35803 = AXIS2_PLACEMENT_3D ( 'NONE', #796, #14201, #38935 ) ;
#35804 = PRODUCT_RELATED_PRODUCT_CATEGORY ( 'part', '', ( #2631 ) ) ;
#35805 = CARTESIAN_POINT ( 'NONE',  ( 787.5162901302840055, -275.3618753856924286, 305.4481719005793252 ) ) ;
#35806 = CARTESIAN_POINT ( 'NONE',  ( 778.7502325331095108, -0.3510508353240099355, 304.6391490659818828 ) ) ;
#35807 = CARTESIAN_POINT ( 'NONE',  ( 790.0220218866281812, -199.0999726633346825, -363.2186876482849129 ) ) ;
#35808 = CARTESIAN_POINT ( 'NONE',  ( 795.1360043628807261, -188.0891481129653187, -360.2193346964456282 ) ) ;
#35809 = CARTESIAN_POINT ( 'NONE',  ( 803.6646147819162707, -353.9073299311467053, -348.8264449731211130 ) ) ;
#35810 = ORIENTED_EDGE ( 'NONE', *, *, #38468, .T. ) ;
#35811 = CARTESIAN_POINT ( 'NONE',  ( 744.7301800767019131, -292.8164208402376971, 337.4774526936615757 ) ) ;
#35812 = FACE_BOUND ( 'NONE', #44138, .T. ) ;
#35813 = CARTESIAN_POINT ( 'NONE',  ( -66.63011601220125613, -365.3551492539851893, -28.13243251470704109 ) ) ;
#35814 = CARTESIAN_POINT ( 'NONE',  ( 769.0155153010367712, -154.3726999360620198, 362.7791456095907279 ) ) ;
#35815 = CARTESIAN_POINT ( 'NONE',  ( 803.6646147819161570, -41.90732993114767169, 348.8264449731210561 ) ) ;
#35816 = VERTEX_POINT ( 'NONE', #28649 ) ;
#35817 = CARTESIAN_POINT ( 'NONE',  ( 762.1177392798416577, -426.5545181178794678, -309.8865473780659272 ) ) ;
#35818 = CIRCLE ( 'NONE', #9172, 50.00000000000004263 ) ;
#35819 = CARTESIAN_POINT ( 'NONE',  ( 763.0537975583476964, -0.4527844766023629286, -371.0346526505628617 ) ) ;
#35820 = CARTESIAN_POINT ( 'NONE',  ( 793.5525998758768083, -271.0999726633344267, 372.6845335610516941 ) ) ;
#35821 = CARTESIAN_POINT ( 'NONE',  ( 769.1273215169530886, -214.7146871989597230, 317.4527132478988847 ) ) ;
#35822 = VECTOR ( 'NONE', #12936, 1000.000000000000114 ) ;
#35823 = CARTESIAN_POINT ( 'NONE',  ( 781.8018195045266339, -358.2709662947829088, -365.1927285166406705 ) ) ;
#35824 = DIRECTION ( 'NONE',  ( -0.000000000000000000, 1.000000000000000000, -0.000000000000000000 ) ) ;
#35825 = CARTESIAN_POINT ( 'NONE',  ( 790.7339360641449275, -462.9631818684622999, 362.6136660859752965 ) ) ;
#35826 =( NAMED_UNIT ( * ) SI_UNIT ( $, .STERADIAN. ) SOLID_ANGLE_UNIT ( ) );
#35827 = CARTESIAN_POINT ( 'NONE',  ( 796.1575198192839480, -270.0090635724253048, -359.4546378042384163 ) ) ;
#35828 = VECTOR ( 'NONE', #9851, 1000.000000000000000 ) ;
#35829 = CARTESIAN_POINT ( 'NONE',  ( 746.8695393053150156, -29.90732993114771787, 327.6429770376306010 ) ) ;
#35830 = CARTESIAN_POINT ( 'NONE',  ( 777.5031285880264704, -94.81642084023843609, 374.9108240113588408 ) ) ;
#35831 = DIRECTION ( 'NONE',  ( -0.000000000000000000, 1.000000000000000000, -0.000000000000000000 ) ) ;
#35832 = DIRECTION ( 'NONE',  ( 0.000000000000000000, 0.000000000000000000, 1.000000000000000000 ) ) ;
#35833 = LINE ( 'NONE', #29372, #37959 ) ;
#35834 = VECTOR ( 'NONE', #38181, 1000.000000000000000 ) ;
#35835 = CARTESIAN_POINT ( 'NONE',  ( 795.8262568251477660, -406.3726999360612808, 308.3538107759623585 ) ) ;
#35836 = DIRECTION ( 'NONE',  ( 0.000000000000000000, -0.9238795325112835188, 0.3826834323650978309 ) ) ;
#35837 = CARTESIAN_POINT ( 'NONE',  ( 751.6929314249748586, -342.9982390220557136, 318.8095938919659034 ) ) ;
#35838 = CARTESIAN_POINT ( 'NONE',  ( 763.2262854647970016, -104.6346026584202207, -309.2812353651462445 ) ) ;
#35839 = CARTESIAN_POINT ( 'NONE',  ( 757.8323909638827445, -266.6346026584197375, -352.1044303154654358 ) ) ;
#35840 = VECTOR ( 'NONE', #9622, 1000.000000000000000 ) ;
#35841 = FACE_BOUND ( 'NONE', #29872, .T. ) ;
#35842 = CARTESIAN_POINT ( 'NONE',  ( 765.0180583372156207, -432.9982390220555999, 360.0135310231089534 ) ) ;
#35843 = CARTESIAN_POINT ( 'NONE',  ( 755.5913626894240451, -181.6454272087892434, 346.6156483768012890 ) ) ;
#35844 = CARTESIAN_POINT ( 'NONE',  ( 773.7305795820266212, -57.28179084515326736, -374.8230680027170365 ) ) ;
#35845 = CARTESIAN_POINT ( 'NONE',  ( 772.3691319403857278, -95.26014174441461080, -315.8894580844506663 ) ) ;
#35846 = CARTESIAN_POINT ( 'NONE',  ( 776.2433038121456548, -108.8965053807782084, 374.8207195650711014 ) ) ;
#35847 = CARTESIAN_POINT ( 'NONE',  ( 774.6312213355098493, -407.3618753856920307, 364.6798772138717482 ) ) ;
#35848 = CARTESIAN_POINT ( 'NONE',  ( 778.1981804954714335, 13.72903370521577138, -314.8072714833589885 ) ) ;
#35850 = ORIENTED_EDGE ( 'NONE', *, *, #10607, .F. ) ;
#35849 = CARTESIAN_POINT ( 'NONE',  ( 773.3843516231979720, -109.4419599262327836, -364.4086373105754433 ) ) ;
#35851 = CARTESIAN_POINT ( 'NONE',  ( 805.1927285166397041, -88.81642084023842187, -341.8018195045277707 ) ) ;
#35852 = CARTESIAN_POINT ( 'NONE',  ( 772.3691319403857278, -407.2601417444137155, -315.8894580844506663 ) ) ;
#35854 = CARTESIAN_POINT ( 'NONE',  ( 792.1044303154646968, -228.4527844766016074, 317.8323909638837677 ) ) ;
#35853 = CARTESIAN_POINT ( 'NONE',  ( 755.0636971347428243, -220.2709662947834772, 341.7834795799807353 ) ) ;
#35855 = CARTESIAN_POINT ( 'NONE',  ( 766.5853460496234675, -397.9874144716864066, -372.3518521366060554 ) ) ;
#35856 = DIRECTION ( 'NONE',  ( 1.644774851296528363E-16, -1.000000000000000000, 0.000000000000000000 ) ) ;
#35857 = ORIENTED_EDGE ( 'NONE', *, *, #17371, .T. ) ;
#35858 = CARTESIAN_POINT ( 'NONE',  ( 756.5762568750052424, -435.1800572038737869, 348.7366044899774238 ) ) ;
#35859 = CIRCLE ( 'NONE', #21848, 6.118999999999985562 ) ;
#35860 = ORIENTED_EDGE ( 'NONE', *, *, #6919, .F. ) ;
#35861 = CARTESIAN_POINT ( 'NONE',  ( 751.6929314249748586, -246.9982390220560546, -318.8095938919659034 ) ) ;
#35862 = CARTESIAN_POINT ( 'NONE',  ( 782.5225473063383106, -190.2709662947835625, 375.2698199232970637 ) ) ;
#35863 = CARTESIAN_POINT ( 'NONE',  ( 757.4527132478984868, -256.3726999360617924, 329.1273215169538844 ) ) ;
#35864 = ORIENTED_EDGE ( 'NONE', *, *, #35975, .T. ) ;
#35865 = CARTESIAN_POINT ( 'NONE',  ( 804.8461984189677878, -74.19088175424410281, -336.9566956441385628 ) ) ;
#35866 = CARTESIAN_POINT ( 'NONE',  ( 776.2433038121456548, -228.8965053807778816, 374.8207195650711014 ) ) ;
#35867 = CARTESIAN_POINT ( 'NONE',  ( 803.4237431249931660, -231.1800572038743553, -331.2633955100225194 ) ) ;
#35868 = EDGE_LOOP ( 'NONE', ( #23847, #4857, #30395, #5381 ) ) ;
#35869 = CARTESIAN_POINT ( 'NONE',  ( 756.5762568750052424, -411.1800572038738437, -348.7366044899774238 ) ) ;
#35870 = CARTESIAN_POINT ( 'NONE',  ( 797.8594530101008786, -37.54369356751132614, -322.1405469898980982 ) ) ;
#35871 = VECTOR ( 'NONE', #901, 1000.000000000000000 ) ;
#35872 = CARTESIAN_POINT ( 'NONE',  ( 763.2154366446407039, -237.6237781080505442, 321.4292242960311228 ) ) ;
#35873 = DIRECTION ( 'NONE',  ( 0.000000000000000000, -0.9238795325112835188, 0.3826834323650978309 ) ) ;
#35874 = DIRECTION ( 'NONE',  ( 5.551115123125783688E-16, 1.000000000000000000, 0.000000000000000000 ) ) ;
#35875 = AXIS2_PLACEMENT_3D ( 'NONE', #9227, #19387, #12242 ) ;
#35876 = CARTESIAN_POINT ( 'NONE',  ( 800.2193346964447755, -18.99823902205683979, -355.1360043628815788 ) ) ;
#35877 = DIRECTION ( 'NONE',  ( -1.000000000000000000, 0.000000000000000000, 0.000000000000000000 ) ) ;
#35878 = LINE ( 'NONE', #5294, #6389 ) ;
#35879 = ORIENTED_EDGE ( 'NONE', *, *, #25526, .F. ) ;
#35880 = CARTESIAN_POINT ( 'NONE',  ( 812.3518521366052028, -313.0999726633342561, -326.5853460496235243 ) ) ;
#35881 = CARTESIAN_POINT ( 'NONE',  ( 814.2805881961230625, -169.6454272087892718, 331.2368401574024119 ) ) ;
#35883 = CARTESIAN_POINT ( 'NONE',  ( 781.8018195045266339, -262.2709662947831930, -365.1927285166406705 ) ) ;
#35882 = FACE_OUTER_BOUND ( 'NONE', #20279, .T. ) ;
#35884 = FACE_OUTER_BOUND ( 'NONE', #41421, .T. ) ;
#35885 = CARTESIAN_POINT ( 'NONE',  ( 799.2566176426618085, -120.0090635724258021, -324.0069404352559559 ) ) ;
#35886 = CARTESIAN_POINT ( 'NONE',  ( 811.0346526505616112, -14.63460265842049424, 323.0537975583477532 ) ) ;
#35887 = LINE ( 'NONE', #29417, #41770 ) ;
#35888 = CARTESIAN_POINT ( 'NONE',  ( 814.2001403089898304, -329.3618753856922581, -347.4397851343538264 ) ) ;
#35889 = PLANE ( 'NONE',  #12116 ) ;
#35890 = CARTESIAN_POINT ( 'NONE',  ( 767.8955696845333705, -0.4527844766023628176, 362.1676090361162323 ) ) ;
#35891 = CARTESIAN_POINT ( 'NONE',  ( 750.9282345327678740, -232.9181544815163249, 319.8311093483690115 ) ) ;
#35892 = CARTESIAN_POINT ( 'NONE',  ( 752.4576283171824116, -189.0783235625961822, -317.7880784355627952 ) ) ;
#35893 = CARTESIAN_POINT ( 'NONE',  ( 796.9462024416508257, -228.4527844766015789, 308.9653473494370246 ) ) ;
#35894 = CARTESIAN_POINT ( 'NONE',  ( 776.2046728542105711, 3.809118245755632959, -304.8212110874238761 ) ) ;
#35895 = VECTOR ( 'NONE', #30815, 1000.000000000000000 ) ;
#35896 = DIRECTION ( 'NONE',  ( 1.000000000000000000, 0.000000000000000000, 0.000000000000000000 ) ) ;
#35897 = ORIENTED_EDGE ( 'NONE', *, *, #9784, .T. ) ;
#35898 = CARTESIAN_POINT ( 'NONE',  ( 797.6776695296629214, -307.5436935675104451, 357.6776695296636603 ) ) ;
#35899 = VECTOR ( 'NONE', #4577, 1000.000000000000000 ) ;
#35900 = CARTESIAN_POINT ( 'NONE',  ( 802.9823548866075953, -73.09997266333502353, 330.0799878456151077 ) ) ;
#35901 = CARTESIAN_POINT ( 'NONE',  ( 805.1016975059191054, 17.10349461922139369, -343.0745993439771837 ) ) ;
#35902 = DIRECTION ( 'NONE',  ( -0.000000000000000000, 1.000000000000000000, 0.000000000000000000 ) ) ;
#35903 = DIRECTION ( 'NONE',  ( 1.000000000000000000, 0.000000000000000000, 0.000000000000000000 ) ) ;
#35905 = CARTESIAN_POINT ( 'NONE',  ( 778.1981804954714335, -370.2709662947831362, 314.8072714833589885 ) ) ;
#35904 = CARTESIAN_POINT ( 'NONE',  ( 804.1601925771018387, -151.4419599262326415, 346.5483106153029098 ) ) ;
#35906 = EDGE_LOOP ( 'NONE', ( #29541, #29983 ) ) ;
#35907 = VECTOR ( 'NONE', #2230, 999.9999999999998863 ) ;
#35908 = CARTESIAN_POINT ( 'NONE',  ( 798.7617431975189675, -291.6237781080503169, -323.0428371773161871 ) ) ;
#35909 = CARTESIAN_POINT ( 'NONE',  ( 754.0944755984390895, -303.6237781080503169, -364.1009440267246760 ) ) ;
#35910 = PLANE ( 'NONE',  #40398 ) ;
#35911 = CARTESIAN_POINT ( 'NONE',  ( 800.9747183278959710, 11.00176097794305541, 311.9810565676471583 ) ) ;
#35912 = EDGE_CURVE ( 'NONE', #966, #13695, #41943, .T. ) ;
#35913 = ORIENTED_EDGE ( 'NONE', *, *, #3573, .T. ) ;
#35914 = CARTESIAN_POINT ( 'NONE',  ( 756.5762568750052424, -339.1800572038740142, 348.7366044899774238 ) ) ;
#35915 = CARTESIAN_POINT ( 'NONE',  ( 754.9735926884551418, -90.35105083532373271, -340.5236548041000333 ) ) ;
#35916 = CARTESIAN_POINT ( 'NONE',  ( 790.8050863131179540, -452.8379544210779954, 362.5841948692291226 ) ) ;
#35917 = EDGE_CURVE ( 'NONE', #29534, #36366, #32103, .T. ) ;
#35918 = CARTESIAN_POINT ( 'NONE',  ( 812.7932403749906598, -135.1800572038746679, -327.7687537140311633 ) ) ;
#35919 = ORIENTED_EDGE ( 'NONE', *, *, #5793, .F. ) ;
#35920 = CARTESIAN_POINT ( 'NONE',  ( 800.2193346964446619, -138.9982390220564241, -355.1360043628816925 ) ) ;
#35921 = ORIENTED_EDGE ( 'NONE', *, *, #23535, .T. ) ;
#35922 = AXIS2_PLACEMENT_3D ( 'NONE', #35530, #24676, #32317 ) ;
#35923 = CARTESIAN_POINT ( 'NONE',  ( 763.8424801807145741, -426.0090635724247932, -320.5453621957614700 ) ) ;
#35924 = CARTESIAN_POINT ( 'NONE',  ( 774.6858677611749044, 14.27448825067031812, 315.5713283507209894 ) ) ;
#35925 = CARTESIAN_POINT ( 'NONE',  ( 760.5453621957607311, -141.0783235625962959, 323.8424801807151425 ) ) ;
#35926 = AXIS2_PLACEMENT_3D ( 'NONE', #43155, #25605, #12192 ) ;
#35929 = CARTESIAN_POINT ( 'NONE',  ( 786.2056067578752163, -395.8055962898682765, 374.4686193811670023 ) ) ;
#35928 = LINE ( 'NONE', #4298, #45462 ) ;
#35927 = DIRECTION ( 'NONE',  ( 0.000000000000000000, -0.3826834323650838421, -0.9238795325112891810 ) ) ;
#35930 = ORIENTED_EDGE ( 'NONE', *, *, #43865, .F. ) ;
#35931 = CARTESIAN_POINT ( 'NONE',  ( 773.4516893846965786, -379.6454272087886466, -315.8398074228977066 ) ) ;
#35932 = DIRECTION ( 'NONE',  ( -1.000000000000000000, -0.000000000000000000, -0.000000000000000000 ) ) ;
#35933 = CARTESIAN_POINT ( 'NONE',  ( 745.7194118038753459, -181.6454272087892434, -348.7631598425976449 ) ) ;
#35934 = CARTESIAN_POINT ( 'NONE',  ( 797.8822607201568644, -78.55451811788046257, 370.1134526219340160 ) ) ;
#35935 = VECTOR ( 'NONE', #28423, 1000.000000000000000 ) ;
#35937 = DIRECTION ( 'NONE',  ( 0.000000000000000000, 0.000000000000000000, -1.000000000000000000 ) ) ;
#35936 = LINE ( 'NONE', #4305, #40373 ) ;
#35938 = CARTESIAN_POINT ( 'NONE',  ( 780.5290396650775619, -324.3510508353229511, -365.2837595273619513 ) ) ;
#35939 = CARTESIAN_POINT ( 'NONE',  ( 791.7608162188021197, 205.0000000000000568, 319.9999999999999432 ) ) ;
#35940 = CARTESIAN_POINT ( 'NONE',  ( 745.5313806188320314, -183.2817908451528695, -333.7943932421247268 ) ) ;
#35941 = CARTESIAN_POINT ( 'NONE',  ( 441.1634899080286232, 259.9999999999999432, -202.7499999999971010 ) ) ;
#35942 = CARTESIAN_POINT ( 'NONE',  ( -598.8365100919716042, 256.5000000000001705, -199.9999999999899671 ) ) ;
#35943 = AXIS2_PLACEMENT_3D ( 'NONE', #372, #606, #32937 ) ;
#35944 = CARTESIAN_POINT ( 'NONE',  ( 798.5707757039680246, -389.4636090269704027, 356.7845633553585003 ) ) ;
#35945 = EDGE_CURVE ( 'NONE', #282, #928, #37473, .T. ) ;
#35946 = CARTESIAN_POINT ( 'NONE',  ( 757.7880784355613741, -354.0090635724250774, 312.4576283171834916 ) ) ;
#35947 = CARTESIAN_POINT ( 'NONE',  ( 745.4481719005789273, -195.7255117493290015, -347.5162901302853697 ) ) ;
#35948 = DIRECTION ( 'NONE',  ( 1.000000000000000000, 0.000000000000000000, 0.000000000000000000 ) ) ;
#35949 = CARTESIAN_POINT ( 'NONE',  ( 765.0180583372156207, -0.9982390220569063999, -360.0135310231089534 ) ) ;
#35950 = CARTESIAN_POINT ( 'NONE',  ( 793.5525998758768083, -151.0999726633347677, 372.6845335610516941 ) ) ;
#35951 = CARTESIAN_POINT ( 'NONE',  ( 768.8385539511368734, -95.26014174441461080, -306.4236121716840557 ) ) ;
#35952 = CARTESIAN_POINT ( 'NONE',  ( 814.5518280994195948, -111.7255117493293000, 332.4837098697145734 ) ) ;
#35953 = CARTESIAN_POINT ( 'NONE',  ( 808.0189434323515343, -350.0891481129648923, -319.0252816721025511 ) ) ;
#35954 = LINE ( 'NONE', #21409, #29117 ) ;
#35955 = DIRECTION ( 'NONE',  ( 0.000000000000000000, 0.000000000000000000, 1.000000000000000000 ) ) ;
#35956 = CARTESIAN_POINT ( 'NONE',  ( 765.0180583372156207, -216.9982390220562252, 360.0135310231089534 ) ) ;
#35957 = CARTESIAN_POINT ( 'NONE',  ( 745.5313806188320314, -447.2817908451521021, 333.7943932421247268 ) ) ;
#35958 = CARTESIAN_POINT ( 'NONE',  ( 810.1134526219336749, -416.5328690171409107, -357.8822607201570349 ) ) ;
#35959 = CARTESIAN_POINT ( 'NONE',  ( 808.0189434323515343, -422.0891481129647218, -319.0252816721025511 ) ) ;
#35960 = CARTESIAN_POINT ( 'NONE',  ( 799.9999999999993179, -462.9681489794448339, 317.6393202250019954 ) ) ;
#35961 = CARTESIAN_POINT ( 'NONE',  ( 761.9338519418445230, -14.53286901714214707, 370.4231160770881957 ) ) ;
#35962 = ORIENTED_EDGE ( 'NONE', *, *, #22429, .T. ) ;
#35963 = AXIS2_PLACEMENT_3D ( 'NONE', #20697, #24854, #28308 ) ;
#35964 = EDGE_CURVE ( 'NONE', #16303, #10930, #24706, .T. ) ;
#35965 = CARTESIAN_POINT ( 'NONE',  ( 800.7704444035546203, -196.1692326535052473, -326.0291762391768771 ) ) ;
#35966 = CARTESIAN_POINT ( 'NONE',  ( 759.7806653035534055, -30.99823902205680071, 324.8639956371180801 ) ) ;
#35967 = CARTESIAN_POINT ( 'NONE',  ( 812.6845335610512393, -175.9874144716871172, -353.5525998758768651 ) ) ;
#35968 = CARTESIAN_POINT ( 'NONE',  ( 744.9990715423526808, -354.3510508353228943, 341.2370466360926002 ) ) ;
#35969 = CARTESIAN_POINT ( 'NONE',  ( 774.6312213355098493, -143.3618753856927697, 364.6798772138717482 ) ) ;
#35970 = ORIENTED_EDGE ( 'NONE', *, *, #5113, .T. ) ;
#35971 = AXIS2_PLACEMENT_3D ( 'NONE', #43065, #32677, #21368 ) ;
#35972 = EDGE_CURVE ( 'NONE', #21525, #42633, #7872, .T. ) ;
#35973 = CARTESIAN_POINT ( 'NONE',  ( 781.8018195045266339, -142.2709662947837330, -365.1927285166406705 ) ) ;
#35974 = CARTESIAN_POINT ( 'NONE',  ( 800.2193346964447755, -330.9982390220558273, 355.1360043628815788 ) ) ;
#35975 = EDGE_CURVE ( 'NONE', #36814, #32576, #24938, .T. ) ;
#35976 = CARTESIAN_POINT ( 'NONE',  ( 745.4481719005789273, -51.72551174932946338, -347.5162901302853129 ) ) ;
#35977 = ORIENTED_EDGE ( 'NONE', *, *, #12855, .T. ) ;
#35978 = CARTESIAN_POINT ( 'NONE',  ( 805.6418435158337843, -461.4636090269701754, -363.8556311672236916 ) ) ;
#35979 = ORIENTED_EDGE ( 'NONE', *, *, #2646, .T. ) ;
#35980 = APPLICATION_PROTOCOL_DEFINITION ( 'draft international standard', 'automotive_design', 1998, #16367 ) ;
#35982 = CARTESIAN_POINT ( 'NONE',  ( 804.6971507214547046, -387.2817908451522726, 344.0799538623459739 ) ) ;
#35981 = CARTESIAN_POINT ( 'NONE',  ( 778.2165204200184689, -46.81642084023858530, 364.9363028652563230 ) ) ;
#35983 = CARTESIAN_POINT ( 'NONE',  ( 768.0187753319979720, -296.6346026584195670, -318.0580252608186242 ) ) ;
#35985 = CARTESIAN_POINT ( 'NONE',  ( 815.1787889125755555, -294.8965053807775689, 343.7953271457877804 ) ) ;
#35984 = CARTESIAN_POINT ( 'NONE',  ( 800.9747183278959710, -396.9982390220556567, 311.9810565676471583 ) ) ;
#35986 = CARTESIAN_POINT ( 'NONE',  ( 810.1134526219336749, -56.53286901714201917, 357.8822607201570349 ) ) ;
#35987 = CARTESIAN_POINT ( 'NONE',  ( 804.6971507214547046, -291.2817908451525000, -344.0799538623459739 ) ) ;
#35988 = CARTESIAN_POINT ( 'NONE',  ( 762.3223304703356007, -271.5436935675106156, -322.3223304703362828 ) ) ;
#35989 = CARTESIAN_POINT ( 'NONE',  ( -66.63011601220125613, -365.3551492539851893, -18.13243251470705886 ) ) ;
#35990 = CARTESIAN_POINT ( 'NONE',  ( 755.3201227861273992, -123.7255117493292147, -345.3687786644892981 ) ) ;
#35991 = EDGE_CURVE ( 'NONE', #24420, #19781, #33075, .T. ) ;
#35992 = DIRECTION ( 'NONE',  ( -1.000000000000000000, -5.551115123125783688E-16, 0.000000000000000000 ) ) ;
#35993 = ORIENTED_EDGE ( 'NONE', *, *, #24982, .F. ) ;
#35994 = CARTESIAN_POINT ( 'NONE',  ( 763.2262854647970016, -440.6346026584191122, 309.2812353651462445 ) ) ;
#35996 = LINE ( 'NONE', #4361, #39614 ) ;
#35995 = LINE ( 'NONE', #29064, #8617 ) ;
#35997 = EDGE_CURVE ( 'NONE', #601, #42149, #11318, .T. ) ;
#35998 = CARTESIAN_POINT ( 'NONE',  ( 791.0478386215596629, -93.82724539060770041, -306.7653713866226326 ) ) ;
#35999 = LINE ( 'NONE', #33001, #30747 ) ;
#36000 = DIRECTION ( 'NONE',  ( -1.000000000000000000, -0.000000000000000000, -0.000000000000000000 ) ) ;
#36001 = CARTESIAN_POINT ( 'NONE',  ( 799.2566176426618085, -264.0090635724253616, 324.0069404352559559 ) ) ;
#36002 = CARTESIAN_POINT ( 'NONE',  ( 757.8323909638827445, -170.6346026584199649, 352.1044303154654358 ) ) ;
#36003 = EDGE_CURVE ( 'NONE', #5266, #42952, #39722, .T. ) ;
#36004 = ORIENTED_EDGE ( 'NONE', *, *, #3388, .F. ) ;
#36005 = CARTESIAN_POINT ( 'NONE',  ( 782.5225473063383106, -118.2709662947838041, -375.2698199232970637 ) ) ;
#36006 = CARTESIAN_POINT ( 'NONE',  ( 795.9930595647434757, -315.0783235625957559, 320.7433823573372820 ) ) ;
#36007 = AXIS2_PLACEMENT_3D ( 'NONE', #18992, #33085, #1863 ) ;
#36008 = CYLINDRICAL_SURFACE ( 'NONE', #3486, 30.00000000000008171 ) ;
#36009 = CARTESIAN_POINT ( 'NONE',  ( 762.1177392798416577, -42.55451811788057626, 309.8865473780659272 ) ) ;
#36010 = CARTESIAN_POINT ( 'NONE',  ( 814.5518280994195948, -231.7255117493288310, -332.4837098697145734 ) ) ;
#36011 = CARTESIAN_POINT ( 'NONE',  ( 755.0636971347428243, -124.2709662947837899, 341.7834795799807353 ) ) ;
#36012 = CARTESIAN_POINT ( 'NONE',  ( 759.9999999999992042, -512.9681489794448908, -370.0000000000000000 ) ) ;
#36013 = CARTESIAN_POINT ( 'NONE',  ( 752.4576283171824116, -309.0783235625957559, -317.7880784355627952 ) ) ;
#36014 = EDGE_CURVE ( 'NONE', #30790, #18371, #38249, .T. ) ;
#36015 = CARTESIAN_POINT ( 'NONE',  ( 796.2681130854250569, -462.7578698805381237, 371.0719813302654870 ) ) ;
#36016 = CARTESIAN_POINT ( 'NONE',  ( 812.7932403749906598, -327.1800572038741279, -327.7687537140311633 ) ) ;
#36017 = CARTESIAN_POINT ( 'NONE',  ( 784.4999999999993179, -365.3551492539851893, -18.13243251470705886 ) ) ;
#36018 = CARTESIAN_POINT ( 'NONE',  ( 800.7704444035546203, -388.1692326535045936, 326.0291762391768771 ) ) ;
#36019 = ORIENTED_EDGE ( 'NONE', *, *, #30611, .T. ) ;
#36020 = FACE_BOUND ( 'NONE', #5075, .T. ) ;
#36021 = CARTESIAN_POINT ( 'NONE',  ( 755.5713283507202505, -413.3618753856920307, -334.6858677611754729 ) ) ;
#36022 = EDGE_CURVE ( 'NONE', #39264, #11556, #35555, .T. ) ;
#36023 = CARTESIAN_POINT ( 'NONE',  ( 754.8983024940795303, -66.89650538077835051, 336.9254006560228163 ) ) ;
#36024 = CARTESIAN_POINT ( 'NONE',  ( 805.9055244015594326, -75.62377810805104161, -315.8990559732753240 ) ) ;
#36025 = DIRECTION ( 'NONE',  ( 0.000000000000000000, 0.000000000000000000, 1.000000000000000000 ) ) ;
#36026 = CARTESIAN_POINT ( 'NONE',  ( 751.2241431872005251, -208.1692326535051905, 359.9636004259367610 ) ) ;
#36027 = CARTESIAN_POINT ( 'NONE',  ( 804.4286716492782716, -41.36187538569314626, 345.3141322388244703 ) ) ;
#36028 = VERTEX_POINT ( 'NONE', #6934 ) ;
#36029 = CARTESIAN_POINT ( 'NONE',  ( 794.1144889064781864, -250.1692326535050199, -360.9840315886528401 ) ) ;
#36030 = ADVANCED_FACE ( 'NONE', ( #14796 ), #3482, .F. ) ;
#36031 = CARTESIAN_POINT ( 'NONE',  ( 759.9864689768902508, -218.0891481129653187, 354.9819416627836404 ) ) ;
#36032 = EDGE_CURVE ( 'NONE', #22430, #25938, #34799, .T. ) ;
#36033 = CARTESIAN_POINT ( 'NONE',  ( 754.0944755984390895, -39.62377810805116951, -364.1009440267246760 ) ) ;
#36034 = CARTESIAN_POINT ( 'NONE',  ( 781.7834795799800531, -346.8164208402376971, 315.0636971347436202 ) ) ;
#36035 = LINE ( 'NONE', #32565, #42357 ) ;
#36036 = ORIENTED_EDGE ( 'NONE', *, *, #31506, .T. ) ;
#36037 = CARTESIAN_POINT ( 'NONE',  ( 762.1177392798416577, -330.5545181178796952, -309.8865473780659272 ) ) ;
#36038 = CIRCLE ( 'NONE', #15369, 10.00000000000000888 ) ;
#36039 = CARTESIAN_POINT ( 'NONE',  ( 814.2001403089898304, -281.3618753856923718, 347.4397851343538264 ) ) ;
#36040 = CARTESIAN_POINT ( 'NONE',  ( 788.7631598425961101, -1.441959926233096656, 305.7194118038759143 ) ) ;
#36041 = CARTESIAN_POINT ( 'NONE',  ( 766.0291762391763086, -178.9181544815165239, -360.7704444035551319 ) ) ;
#36042 = CARTESIAN_POINT ( 'NONE',  ( 765.0180583372156207, -192.9982390220562820, -360.0135310231089534 ) ) ;
#36043 = CARTESIAN_POINT ( 'NONE',  ( 764.8639956371174549, -368.0891481129647786, -319.7806653035542581 ) ) ;
#36044 = ORIENTED_EDGE ( 'NONE', *, *, #16217, .F. ) ;
#36045 = CARTESIAN_POINT ( 'NONE',  ( 790.8726784830453198, 13.28531280103958423, -362.5472867521010585 ) ) ;
#36046 = EDGE_LOOP ( 'NONE', ( #27545, #10707, #2157, #15008 ) ) ;
#36047 = CARTESIAN_POINT ( 'NONE',  ( 815.2698199232961542, -280.8164208402378677, 342.5225473063383106 ) ) ;
#36048 = CARTESIAN_POINT ( 'NONE',  ( -26.63011601220122060, 26.27639943461401018, 900.0000000000001137 ) ) ;
#36049 = CARTESIAN_POINT ( 'NONE',  ( 757.4527132478984868, -208.3726999360619061, 329.1273215169538844 ) ) ;
#36050 = CARTESIAN_POINT ( 'NONE',  ( -949.5497976682736407, 230.0000000000002274, -2132.806278688367456 ) ) ;
#36051 = CARTESIAN_POINT ( 'NONE',  ( 780.5236548040995785, -164.7363362996983938, 314.9735926884559944 ) ) ;
#36052 = CARTESIAN_POINT ( 'NONE',  ( 781.7834795799800531, -34.81642084023861372, 315.0636971347436202 ) ) ;
#36053 = ORIENTED_EDGE ( 'NONE', *, *, #26099, .T. ) ;
#36054 = CARTESIAN_POINT ( 'NONE',  ( 804.1009440267234822, -407.4636090269703459, -314.0944755984392600 ) ) ;
#36055 = CARTESIAN_POINT ( 'NONE',  ( 772.4837098697145166, 0.6381246143067237364, -374.5518280994205611 ) ) ;
#36056 = CARTESIAN_POINT ( 'NONE',  ( 811.3240766477731540, -268.3726999360616787, 355.6651683502462902 ) ) ;
#36057 = CARTESIAN_POINT ( 'NONE',  ( 756.7813123517142913, -211.9874144716869750, 329.9779781133712504 ) ) ;
#36058 = CARTESIAN_POINT ( 'NONE',  ( 792.1044303154645831, -372.4527844766010958, -317.8323909638837677 ) ) ;
#36059 = PLANE ( 'NONE',  #26796 ) ;
#36060 = CARTESIAN_POINT ( 'NONE',  ( 793.0897708529556667, -462.5545181178792973, 361.3366627262616362 ) ) ;
#36061 = CARTESIAN_POINT ( 'NONE',  ( 802.9823548866075953, -265.0999726633344267, -330.0799878456151077 ) ) ;
#36062 = CARTESIAN_POINT ( 'NONE',  ( 811.0346526505616112, -62.63460265842031305, 323.0537975583477532 ) ) ;
#36063 = CARTESIAN_POINT ( 'NONE',  ( 804.7487373415286811, -115.5436935675110988, 364.7487373415288516 ) ) ;
#36064 = DIRECTION ( 'NONE',  ( 0.000000000000000000, 0.000000000000000000, -1.000000000000000000 ) ) ;
#36065 =( NAMED_UNIT ( * ) PLANE_ANGLE_UNIT ( ) SI_UNIT ( $, .RADIAN. ) );
#36066 = CIRCLE ( 'NONE', #5792, 10.00000000000000888 ) ;
#36067 = CARTESIAN_POINT ( 'NONE',  ( 771.3260364891663130, -379.6454272087886466, 306.0683387631859773 ) ) ;
#36068 = ADVANCED_FACE ( 'NONE', ( #34584 ), #3162, .T. ) ;
#36069 = DIRECTION ( 'NONE',  ( 1.000000000000000000, 0.000000000000000000, -0.000000000000000000 ) ) ;
#36070 = CARTESIAN_POINT ( 'NONE',  ( 767.7687537140311633, -311.9073299311468759, 372.7932403749916830 ) ) ;
#36071 = CARTESIAN_POINT ( 'NONE',  ( 797.8594530101008786, -325.5436935675105019, -322.1405469898980982 ) ) ;
#36072 = DIRECTION ( 'NONE',  ( -0.000000000000000000, 1.000000000000000000, -0.000000000000000000 ) ) ;
#36073 = CARTESIAN_POINT ( 'NONE',  ( 771.1735550268778070, -417.1800572038736163, 316.3353852180827630 ) ) ;
#36074 = CARTESIAN_POINT ( 'NONE',  ( 804.8461984189677878, -194.1908817542437475, 336.9566956441385628 ) ) ;
#36075 = CARTESIAN_POINT ( 'NONE',  ( 813.5763878283155464, -51.82724539060782121, -351.1614460488615350 ) ) ;
#36076 = CARTESIAN_POINT ( 'NONE',  ( 804.1601925771018387, -103.4419599262327836, -346.5483106153029098 ) ) ;
#36077 = CARTESIAN_POINT ( 'NONE',  ( 749.8865473780648472, -116.5328690171418202, 322.1177392798429082 ) ) ;
#36078 = CARTESIAN_POINT ( 'NONE',  ( 755.5713283507202505, -437.3618753856919170, 334.6858677611754729 ) ) ;
#36079 = CARTESIAN_POINT ( 'NONE',  ( 762.3223304703356007, -7.543693567511430942, -322.3223304703362828 ) ) ;
#36081 = EDGE_LOOP ( 'NONE', ( #30914, #42003, #45123, #12 ) ) ;
#36080 = CARTESIAN_POINT ( 'NONE',  ( 779.4709603349208464, -144.3510508353235764, -314.7162404726379918 ) ) ;
#36082 = CARTESIAN_POINT ( 'NONE',  ( 781.8018195045266339, -94.27096629478386092, -365.1927285166406705 ) ) ;
#36083 = EDGE_CURVE ( 'NONE', #12726, #43693, #41514, .T. ) ;
#36084 = CARTESIAN_POINT ( 'NONE',  ( 761.2382568024794409, -399.6237781080500326, -356.9571628226838129 ) ) ;
#36086 = CARTESIAN_POINT ( 'NONE',  ( 774.6858677611749044, -225.7255117493289163, 315.5713283507209894 ) ) ;
#36085 = CARTESIAN_POINT ( 'NONE',  ( 771.1735550268778070, -249.1800572038742416, 316.3353852180827630 ) ) ;
#36087 = CARTESIAN_POINT ( 'NONE',  ( 51.16348990802859475, 260.0000000000000568, -202.7499999999943441 ) ) ;
#36088 = ORIENTED_EDGE ( 'NONE', *, *, #12264, .T. ) ;
#36089 = CARTESIAN_POINT ( 'NONE',  ( 771.2633955100217236, -431.9073299311464211, 363.4237431249939618 ) ) ;
#36090 = ORIENTED_EDGE ( 'NONE', *, *, #20725, .T. ) ;
#36091 =( LENGTH_UNIT ( ) NAMED_UNIT ( * ) SI_UNIT ( .MILLI., .METRE. ) );
#36092 = CARTESIAN_POINT ( 'NONE',  ( 745.7998596910086917, -197.3618753856926560, 332.5602148656461168 ) ) ;
#36093 = CARTESIAN_POINT ( 'NONE',  ( 755.5913626894240451, -253.6454272087889876, 346.6156483768012890 ) ) ;
#36094 = ORIENTED_EDGE ( 'NONE', *, *, #44162, .F. ) ;
#36095 = CARTESIAN_POINT ( 'NONE',  ( 760.7433823573367135, -84.00906357242590161, -355.9930595647440441 ) ) ;
#36096 = CARTESIAN_POINT ( 'NONE',  ( 805.9055244015594326, -219.6237781080506295, 315.8990559732753240 ) ) ;
#36097 = CARTESIAN_POINT ( 'NONE',  ( 795.1360043628808398, -260.0891481129650629, -360.2193346964456282 ) ) ;
#36098 = ORIENTED_EDGE ( 'NONE', *, *, #3514, .F. ) ;
#36099 = VECTOR ( 'NONE', #38119, 1000.000000000000000 ) ;
#36100 = CARTESIAN_POINT ( 'NONE',  ( 792.1044303154645831, -396.4527844766010389, -317.8323909638837677 ) ) ;
#36101 = CARTESIAN_POINT ( 'NONE',  ( 802.1676090361156639, -38.63460265842041252, -327.8955696845344505 ) ) ;
#36102 = CARTESIAN_POINT ( 'NONE',  ( 805.0264073115434940, -270.3510508353231216, 339.4763451958999099 ) ) ;
#36103 = DIRECTION ( 'NONE',  ( -0.000000000000000000, 1.000000000000000000, -0.000000000000000000 ) ) ;
#36104 = DIRECTION ( 'NONE',  ( -1.000000000000000000, -0.000000000000000000, -0.000000000000000000 ) ) ;
#36105 = CARTESIAN_POINT ( 'NONE',  ( 804.4286716492782716, -17.36187538569322086, -345.3141322388244703 ) ) ;
#36106 = DIRECTION ( 'NONE',  ( 1.000000000000000000, 0.000000000000000000, 0.000000000000000000 ) ) ;
#36107 = VERTEX_POINT ( 'NONE', #23706 ) ;
#36108 = CARTESIAN_POINT ( 'NONE',  ( 799.9636004259356241, -310.9181544815160123, -311.2241431872006956 ) ) ;
#36109 = CARTESIAN_POINT ( 'NONE',  ( 746.4236121716829757, -183.8272453906074020, 328.8385539511384650 ) ) ;
#36111 = CARTESIAN_POINT ( 'NONE',  ( 768.0187753319979720, -272.6346026584196807, -318.0580252608186242 ) ) ;
#36110 = DIRECTION ( 'NONE',  ( -1.880165489482579047E-16, -1.000000000000000000, -0.000000000000000000 ) ) ;
#36112 = CARTESIAN_POINT ( 'NONE',  ( 773.4516893846965786, -139.6454272087893571, -315.8398074228977066 ) ) ;
#36113 = CARTESIAN_POINT ( 'NONE',  ( 747.2067596250078623, -27.18005720387500901, 352.2312462859687230 ) ) ;
#36114 = FACE_OUTER_BOUND ( 'NONE', #5513, .T. ) ;
#36115 = CARTESIAN_POINT ( 'NONE',  ( 752.4576283171824116, -21.07832356259667250, -317.7880784355627952 ) ) ;
#36116 = CARTESIAN_POINT ( 'NONE',  ( 804.7487373415286811, -355.5436935675103882, -364.7487373415288516 ) ) ;
#36117 = CARTESIAN_POINT ( 'NONE',  ( 939.9999999999992042, 240.0000000000000568, -201.9999999999999716 ) ) ;
#36118 = CARTESIAN_POINT ( 'NONE',  ( 774.6312213355099630, 0.6381246143067236254, 364.6798772138717482 ) ) ;
#36119 = CARTESIAN_POINT ( 'NONE',  ( 773.7305795820266212, -273.2817908451526137, 374.8230680027170365 ) ) ;
#36120 = CARTESIAN_POINT ( 'NONE',  ( 812.6845335610512393, -223.9874144716869182, -353.5525998758768651 ) ) ;
#36121 = CARTESIAN_POINT ( 'NONE',  ( 772.4837098697144029, -239.3618753856924570, 374.5518280994205611 ) ) ;
#36122 = CARTESIAN_POINT ( 'NONE',  ( 782.4968714119720516, 13.18357915976123174, -305.0891759886411023 ) ) ;
#36123 = CARTESIAN_POINT ( 'NONE',  ( 831.1634899080286232, 256.4999999999998863, -199.9999999999999432 ) ) ;
#36124 = ORIENTED_EDGE ( 'NONE', *, *, #41125, .F. ) ;
#36125 = CARTESIAN_POINT ( 'NONE',  ( 765.0180583372156207, -312.9982390220559409, 360.0135310231089534 ) ) ;
#36126 = ADVANCED_FACE ( 'NONE', ( #27198 ), #17252, .F. ) ;
#36127 = EDGE_CURVE ( 'NONE', #9763, #29534, #3406, .T. ) ;
#36128 = CARTESIAN_POINT ( 'NONE',  ( 805.2837595273609850, -98.73633629969859271, 340.5290396650784714 ) ) ;
#36129 = CARTESIAN_POINT ( 'NONE',  ( 800.0135310231082713, -446.0891481129646081, -325.0180583372163028 ) ) ;
#36130 = AXIS2_PLACEMENT_3D ( 'NONE', #29514, #40977, #11511 ) ;
#36131 = CARTESIAN_POINT ( 'NONE',  ( -26.63011601220122060, -544.8427095258973623, -350.0000000000000000 ) ) ;
#36132 = CARTESIAN_POINT ( 'NONE',  ( -468.8365100919714337, 258.0940000000001646, -199.9999999999908766 ) ) ;
#36134 = CARTESIAN_POINT ( 'NONE',  ( 805.1927285166397041, -376.8164208402375834, 341.8018195045277707 ) ) ;
#36133 = CARTESIAN_POINT ( 'NONE',  ( 770.0799878456142551, -157.9874144716871456, 362.9823548866085616 ) ) ;
#36135 = ORIENTED_EDGE ( 'NONE', *, *, #4112, .T. ) ;
#36136 = CARTESIAN_POINT ( 'NONE',  ( 754.8983024940795303, -306.8965053807775689, -336.9254006560228163 ) ) ;
#36137 = CARTESIAN_POINT ( 'NONE',  ( 759.7806653035534055, -174.9982390220563673, 324.8639956371180801 ) ) ;
#36138 = CARTESIAN_POINT ( 'NONE',  ( 810.1134526219336749, -344.5328690171410813, -357.8822607201570349 ) ) ;
#36139 = CYLINDRICAL_SURFACE ( 'NONE', #39652, 19.99999999999990763 ) ;
#36140 = CARTESIAN_POINT ( 'NONE',  ( 796.9462024416508257, 11.54721552339760038, 308.9653473494370246 ) ) ;
#36141 = EDGE_LOOP ( 'NONE', ( #19038, #1138, #6130, #14759, #44556, #4382 ) ) ;
#36142 = CARTESIAN_POINT ( 'NONE',  ( 795.1360043628807261, -332.0891481129649492, 360.2193346964456282 ) ) ;
#36143 = CARTESIAN_POINT ( 'NONE',  ( 757.2208543904082489, -64.71468719896019195, -350.9844846989624330 ) ) ;
#36144 = CARTESIAN_POINT ( 'NONE',  ( 789.5670355615794733, -453.0432664090020012, 363.0970091259334822 ) ) ;
#36145 = CARTESIAN_POINT ( 'NONE',  ( 782.4968714119720516, -130.8164208402383224, -305.0891759886411023 ) ) ;
#36146 = EDGE_LOOP ( 'NONE', ( #20061, #21224, #33901, #14411 ) ) ;
#36147 = CARTESIAN_POINT ( 'NONE',  ( 802.1676090361155502, -158.6346026584200217, -327.8955696845344505 ) ) ;
#36148 = ORIENTED_EDGE ( 'NONE', *, *, #32371, .T. ) ;
#36149 = CARTESIAN_POINT ( 'NONE',  ( 801.5560724626406000, -432.5545181178793541, -326.7756240680316182 ) ) ;
#36150 = CARTESIAN_POINT ( 'NONE',  ( 804.6971507214547046, -459.2817908451519884, 344.0799538623459739 ) ) ;
#36151 = CARTESIAN_POINT ( 'NONE',  ( 751.6929314249748586, -222.9982390220561399, 318.8095938919659034 ) ) ;
#36152 = CARTESIAN_POINT ( 'NONE',  ( 772.3691319403857278, -143.2601417444144829, 315.8894580844506663 ) ) ;
#36155 = CARTESIAN_POINT ( 'NONE',  ( 746.7653713866222915, -401.2601417444137155, 351.0478386215610271 ) ) ;
#36154 = DIRECTION ( 'NONE',  ( 0.000000000000000000, -1.000000000000000000, 0.000000000000000000 ) ) ;
#36153 = CARTESIAN_POINT ( 'NONE',  ( 939.9999999999992042, 240.0000000000000568, -201.9999999999999716 ) ) ;
#36156 = VERTEX_POINT ( 'NONE', #20706 ) ;
#36157 = CARTESIAN_POINT ( 'NONE',  ( 793.9708237608222134, -406.9181544815157849, -319.2295555964448681 ) ) ;
#36158 = LINE ( 'NONE', #35692, #14482 ) ;
#36159 = CARTESIAN_POINT ( 'NONE',  ( 748.6759233522253680, -208.3726999360619061, -324.3348316497537098 ) ) ;
#36160 = CARTESIAN_POINT ( 'NONE',  ( 811.3240766477731540, -52.37269993606237506, 355.6651683502462902 ) ) ;
#36162 = DIRECTION ( 'NONE',  ( -0.000000000000000000, 1.000000000000000000, -0.000000000000000000 ) ) ;
#36161 = CARTESIAN_POINT ( 'NONE',  ( 779.9999999999992042, -452.9681489794448339, 339.9999999999999432 ) ) ;
#36163 = CARTESIAN_POINT ( 'NONE',  ( 779.4709603349208464, -312.3510508353230080, -314.7162404726379918 ) ) ;
#36164 =( BOUNDED_CURVE ( )  B_SPLINE_CURVE ( 2, ( #20325, #5791, #13188, #19880, #5553, #34171, #16407, #30487, #41137, #44592, #44124, #27038, #23089, #34653, #2787, #30043, #12952, #30962, #2544, #13411, #9019, #44829, #16648, #27270, #19647, #9709, #23772, #45056, #27482, #24007, #20557, #15960, #41822, #13871, #25153, #35098, #13634, #39263, #28396, #6926, #17565, #17321, #461, #42043, #10389, #6697, #14566, #34869, #32091, #7619, #227, #24464, #20776, #42496, #10167, #4, #28641, #24698, #14095, #31637, #3474, #28169, #27946, #31180, #42261, #24243, #21695, #7395, #17100, #21007, #21469, #10621, #42719, #45275, #17790, #3232, #38816, #3012, #39045, #38572, #14320, #38352, #31855, #7171, #10864, #21245, #35325, #27717, #3703, #24931, #35547, #3923, #18018, #11083, #15677, #29094, #8533, #903, #7863, #11991, #15470, #8758, #21941, #5058, #39741, #36242, #36027, #22597, #4390, #35790, #4167, #32337, #4602, #29548, #43834, #26297, #43624, #39507, #19150, #43179, #28862, #43408, #18481, #11774, #18696, #33236, #33029, #1577, #15006, #11548, #11311, #32559, #1366, #18263, #32786, #4831, #25631, #29757, #36700, #29336, #8091, #12218, #18934, #22153, #25844, #26057, #1136, #8300, #15247, #39956, #22364, #40168, #36469, #40409, #691, #14789, #42943, #25388, #30679, #16128, #26520, #40841, #5954, #5272, #44535, #2034, #13356, #30436, #12895, #27430, #30213, #37378, #16828, #44304, #23275, #40620, #26979, #5736, #41079, #5494, #9435, #19823, #12440, #12659, #36918, #37601, #1794, #27213, #19589, #23500, #20044, #22824, #33906, #8971, #2259, #37135, #34122, #44777, #2735, #2488, #9201, #16356, #45001, #33684, #30907, #26739, #19365, #6183, #16597, #13135, #41307, #41528, #20273, #9658, #29988, #23721, #37833, #34364, #33450, #15901, #44074, #6647, #7116, #24194, #27660, #31805, #3418, #24638, #6430, #38995, #406, #21196, #17266, #13581, #3654, #17044, #6867, #7345, #31591, #20947, #38515, #3176, #35044, #38301, #38071, #17513, #31123, #28587, #14265, #23952, #13820, #28333, #27899, #21422, #20511, #38759, #10118, #45694, #14509, #174, #41767, #31355, #45219, #35276, #14047, #17742, #2957, #20721, #32033, #41995, #34599, #9880, #42436, #10338, #24411, #35498, #45460, #10805, #34815, #28117, #24880, #42211, #3872, #10561, #17964, #39687, #43124, #25574, #9080, #11494, #42892, #11036, #1917, #35969, #26625, #19712, #5616, #4337, #2150, #18426, #23146, #35731, #7805, #33798, #29039, #7569, #16242, #22930, #855, #8035, #37253, #32506, #16024, #21880, #14738, #19471, #37023, #5378, #42673, #28812, #12550, #22101, #36191, #25102, #4553, #11258, #39217, #30103, #14955, #40723, #21645, #4109, #18644, #32733, #1079, #25334, #15192, #29277, #43354, #39448, #11721, #26412, #32280, #40513, #18204, #8863, #636, #44189, #33567, #6303, #45114, #30321, #27325, #2370, #41418, #34015, #41645, #6533, #10224, #13471, #16709, #9767, #6759, #16468, #24302, #34234, #26848, #13700, #2844, #27541, #20613, #38408, #27780, #16937, #37491, #24070, #20158, #19939, #2608, #10000, #12767, #27103, #38188, #44651, #30551, #34708, #23834, #3066, #40957, #41880, #20832, #17156, #37718, #13013, #31242, #5851, #37949, #34932, #20387, #34485, #13247, #9319, #41194, #9548, #31016, #44412, #6068, #45338, #3298, #23390, #23611, #30794, #44886, #3758, #7680, #32159, #17627, #7455, #21078, #24765, #13929, #35162, #28004, #31914, #42781, #25453, #7927, #11143, #3541, #32403, #10683, #10449, #17392, #38882, #7237, #39572, #17848, #6995, #21308, #31477, #524, #38635, #31693, #14630, #36086, #286, #28702, #28223, #753, #35854, #10926, #61, #21760, #18323, #4231, #14153, #28464, #21997, #42318, #43006, #35385, #14386, #14851, #18079, #45581, #21529, #42564, #25213, #24994, #39324, #39105, #35608, #3982, #28928, #11370, #42098, #24525, #1635, #18759, #22210, #26358, #11827, #18991, #44133, #5115, #40672, #40239, #22424, #40462, #8814, #36303, #15734, #15305, #39799, #22662, #4660, #43460, #29603, #32849, #32620, #15523, #25897, #22883, #1862, #19203, #43681, #963, #40008, #36533, #36974, #33290, #1197, #8596, #8147, #8358, #15068, #4890, #29388, #29823, #12052, #43905, #1421, #33513, #29155, #43238, #26124, #33084, #5327, #15968, #36759, #12282, #30050, #19421, #12498, #26574, #9026, #23095, #4452, #18540, #11609, #25687, #37663, #37440, #9944, #9269, #10174, #5562, #41587, #19654, #41144, #24016, #9496, #34660, #33747, #6245, #5800, #30741, #27726, #27489, #23337, #34428, #26795, #20335, #44835, #2795, #30268, #2315, #13642, #23559, #2097, #41828, #16887, #6012, #20104, #31188, #30494, #38135, #16414, #19886, #13419, #30968, #6486, #13198, #3020, #34178, #2550, #16657, #45282, #41369, #33964, #16187, #37196, #44598, #44360, #12716, #40900, #12960, #27046, #9715, #23781, #37894, #45065, #31642, #14101, #698, #24704, #13876, #10, #38359, #39052, #3239, #28647, #21015, #232, #7401, #24251, #21252, #42048, #35332, #27952, #35552, #14571, #25159, #11089, #35105, #3709, #14794, #10396, #4175, #28174, #20782, #7624, #42504, #21475, #469, #18270, #21700, #10870, #31418, #18023, #42267, #10627, #38826, #17796, #7178, #3481, #3928, #38579, #24471, #42725, #31861, #32100, #34876, #35796, #28868, #39268, #14327, #6932, #32342, #45524, #28404, #17571, #24936, #42948, #6705, #17329, #36034, #39513, #11316, #4396, #7870, #25393, #18487, #15012, #908, #21948, #32564, #29100, #34006, #2360, #30311, #5845, #30786, #23825, #9072, #6058, #26839, #20149, #12760, #20379, #31008, #34700, #37936, #41185, #2600, #6294, #37484, #27317, #16459, #23381, #44644, #9760, #17148, #13239, #19931, #34476, #9539, #16928, #30542, #40948, #27093, #23603, #34225, #37709, #13005, #2836, #16701, #9311, #45106, #44877, #13463, #3059, #27532, #45329, #41410, #41632, #9991, #24060, #38178, #6526, #20605, #44405, #31233, #13691, #27770, #23138, #37244, #5607, #19701, #16232, #33791, #2143, #10918, #35377, #38399, #3529, #28216, #32152, #24987, #42089, #31907, #45570, #17615, #6749, #31684, #31465, #39097, #3752, #7447, #34924, #6984, #20823, #3288, #17840, #21069, #18070, #7672, #42310, #10440, #39316, #35152, #51, #13922, #21750, #27994, #515, #279, #35847, #38873, #10674, #24758, #14623, #24515, #14844, #10216, #17383, #7228, #21522, #4222, #32394, #35599, #38624, #11134, #14145, #21299, #41872, #28695, #18315, #25206, #14376, #28457, #42556, #3976, #42774, #745, #24293, #29382, #25679, #26115, #43230, #954, #5108, #22418, #43674, #25443, #12274, #19415, #40229, #36296, #32613, #22652, #15060, #8588, #39792, #18531, #1413, #29146, #22204, #8350, #11601, #11364, #40002, #36078, #1853, #33283, #42998, #32839, #1628, #1190, #26349, #39564, #12045, #8140, #18984, #4654, #18751, #7919, #15298, #43454, #36750, #36521, #19196, #21989, #11821, #5320, #25889, #4445, #33505, #15727, #4882, #33074, #15516, #40453 ),
 .UNSPECIFIED., .F., .T. ) 
 B_SPLINE_CURVE_WITH_KNOTS ( ( 3, 2, 2, 2, 2, 2, 2, 2, 2, 2, 2, 2, 2, 2, 2, 2, 2, 2, 2, 2, 2, 2, 2, 2, 2, 2, 2, 2, 2, 2, 2, 2, 2, 2, 2, 2, 2, 2, 2, 2, 2, 2, 2, 2, 2, 2, 2, 2, 2, 2, 2, 2, 2, 2, 2, 2, 2, 2, 2, 2, 2, 2, 2, 2, 2, 2, 2, 2, 2, 2, 2, 2, 2, 2, 2, 2, 2, 2, 2, 2, 2, 2, 2, 2, 2, 2, 2, 2, 2, 2, 2, 2, 2, 2, 2, 2, 2, 2, 2, 2, 2, 2, 2, 2, 2, 2, 2, 2, 2, 2, 2, 2, 2, 2, 2, 2, 2, 2, 2, 2, 2, 2, 2, 2, 2, 2, 2, 2, 2, 2, 2, 2, 2, 2, 2, 2, 2, 2, 2, 2, 2, 2, 2, 2, 2, 2, 2, 2, 2, 2, 2, 2, 2, 2, 2, 2, 2, 2, 2, 2, 2, 2, 2, 2, 2, 2, 2, 2, 2, 2, 2, 2, 2, 2, 2, 2, 2, 2, 2, 2, 2, 2, 2, 2, 2, 2, 2, 2, 2, 2, 2, 2, 2, 2, 2, 2, 2, 2, 2, 2, 2, 2, 2, 2, 2, 2, 2, 2, 2, 2, 2, 2, 2, 2, 2, 2, 2, 2, 2, 2, 2, 2, 2, 2, 2, 2, 2, 2, 2, 2, 2, 2, 2, 2, 2, 2, 2, 2, 2, 2, 2, 2, 2, 2, 2, 2, 2, 2, 2, 2, 2, 2, 2, 2, 2, 2, 2, 2, 2, 2, 2, 2, 2, 2, 2, 2, 2, 2, 2, 2, 2, 2, 2, 2, 2, 2, 2, 2, 2, 2, 2, 2, 2, 2, 2, 2, 2, 2, 2, 2, 2, 2, 2, 2, 2, 2, 2, 2, 2, 2, 2, 2, 2, 2, 2, 2, 2, 2, 2, 2, 2, 2, 2, 2, 2, 2, 2, 2, 2, 2, 2, 2, 2, 2, 2, 2, 2, 2, 2, 2, 2, 2, 2, 2, 2, 2, 2, 2, 2, 2, 2, 2, 2, 2, 2, 2, 2, 2, 2, 2, 2, 2, 2, 2, 2, 2, 2, 2, 2, 2, 2, 2, 2, 2, 2, 2, 2, 2, 2, 2, 2, 2, 2, 2, 2, 2, 2, 2, 2, 2, 2, 2, 2, 2, 2, 2, 2, 2, 2, 2, 2, 2, 2, 2, 2, 2, 2, 2, 2, 2, 2, 2, 2, 2, 2, 2, 2, 2, 2, 2, 2, 2, 2, 2, 2, 2, 2, 2, 2, 2, 2, 2, 2, 2, 2, 2, 2, 2, 2, 2, 2, 3 ),
 ( 0.000000000000000000, 0.002272727272727272617, 0.004545454545454545234, 0.006818181818181817851, 0.009090909090909090468, 0.01136363636363636395, 0.01363636363636363570, 0.01590909090909090745, 0.01818181818181818094, 0.02045454545454545442, 0.02272727272727272790, 0.02500000000000000139, 0.02727272727272727140, 0.02954545454545454489, 0.03181818181818181490, 0.03409090909090908839, 0.03636363636363636187, 0.03863636363636363535, 0.04090909090909090884, 0.04318181818181818232, 0.04545454545454545581, 0.04772727272727272929, 0.05000000000000000278, 0.05227272727272727626, 0.05454545454545454281, 0.05681818181818181629, 0.05909090909090908977, 0.06136363636363636326, 0.06363636363636362980, 0.06590909090909090329, 0.06818181818181817677, 0.07045454545454545026, 0.07272727272727272374, 0.07499999999999999722, 0.07727272727272727071, 0.07954545454545454419, 0.08181818181818181768, 0.08409090909090909116, 0.08636363636363636465, 0.08863636363636363813, 0.09090909090909091161, 0.09318181818181818510, 0.09545454545454545858, 0.09772727272727273207, 0.1000000000000000056, 0.1022727272727272790, 0.1045454545454545525, 0.1068181818181818121, 0.1090909090909090856, 0.1113636363636363591, 0.1136363636363636326, 0.1159090909090909061, 0.1181818181818181795, 0.1204545454545454530, 0.1227272727272727265, 0.1250000000000000000, 0.1272727272727272596, 0.1295454545454545470, 0.1318181818181818066, 0.1340909090909090939, 0.1363636363636363535, 0.1386363636363636409, 0.1409090909090909005, 0.1431818181818181879, 0.1454545454545454475, 0.1477272727272727348, 0.1499999999999999944, 0.1522727272727272818, 0.1545454545454545414, 0.1568181818181818288, 0.1590909090909090884, 0.1613636363636363757, 0.1636363636363636354, 0.1659090909090909227, 0.1681818181818181823, 0.1704545454545454419, 0.1727272727272727293, 0.1749999999999999889, 0.1772727272727272763, 0.1795454545454545359, 0.1818181818181818232, 0.1840909090909090828, 0.1863636363636363702, 0.1886363636363636298, 0.1909090909090909172, 0.1931818181818181768, 0.1954545454545454641, 0.1977272727272727237, 0.2000000000000000111, 0.2022727272727272707, 0.2045454545454545581, 0.2068181818181818177, 0.2090909090909091050, 0.2113636363636363646, 0.2136363636363636243, 0.2159090909090909116, 0.2181818181818181712, 0.2204545454545454586, 0.2227272727272727182, 0.2250000000000000056, 0.2272727272727272652, 0.2295454545454545525, 0.2318181818181818121, 0.2340909090909090995, 0.2363636363636363591, 0.2386363636363636465, 0.2409090909090909061, 0.2431818181818181934, 0.2454545454545454530, 0.2477272727272727404, 0.2500000000000000000, 0.2522727272727272596, 0.2545454545454545192, 0.2568181818181818343, 0.2590909090909090939, 0.2613636363636363535, 0.2636363636363636131, 0.2659090909090909283, 0.2681818181818181879, 0.2704545454545454475, 0.2727272727272727071, 0.2750000000000000222, 0.2772727272727272818, 0.2795454545454545414, 0.2818181818181818010, 0.2840909090909091161, 0.2863636363636363757, 0.2886363636363636354, 0.2909090909090908950, 0.2931818181818181546, 0.2954545454545454697, 0.2977272727272727293, 0.2999999999999999889, 0.3022727272727272485, 0.3045454545454545636, 0.3068181818181818232, 0.3090909090909090828, 0.3113636363636363424, 0.3136363636363636576, 0.3159090909090909172, 0.3181818181818181768, 0.3204545454545454364, 0.3227272727272727515, 0.3250000000000000111, 0.3272727272727272707, 0.3295454545454545303, 0.3318181818181818454, 0.3340909090909090495, 0.3363636363636363646, 0.3386363636363636243, 0.3409090909090908839, 0.3431818181818181990, 0.3454545454545454586, 0.3477272727272727182, 0.3499999999999999778, 0.3522727272727272929, 0.3545454545454545525, 0.3568181818181818121, 0.3590909090909090717, 0.3613636363636363869, 0.3636363636363636465, 0.3659090909090909061, 0.3681818181818181657, 0.3704545454545454808, 0.3727272727272727404, 0.3750000000000000000, 0.3772727272727272596, 0.3795454545454545192, 0.3818181818181818343, 0.3840909090909090939, 0.3863636363636363535, 0.3886363636363636131, 0.3909090909090909283, 0.3931818181818181879, 0.3954545454545454475, 0.3977272727272727071, 0.4000000000000000222, 0.4022727272727272818, 0.4045454545454545414, 0.4068181818181818010, 0.4090909090909091161, 0.4113636363636363757, 0.4136363636363636354, 0.4159090909090908950, 0.4181818181818182101, 0.4204545454545454697, 0.4227272727272727293, 0.4249999999999999889, 0.4272727272727272485, 0.4295454545454545636, 0.4318181818181818232, 0.4340909090909090828, 0.4363636363636363424, 0.4386363636363636576, 0.4409090909090909172, 0.4431818181818181768, 0.4454545454545454364, 0.4477272727272727515, 0.4500000000000000111, 0.4522727272727272707, 0.4545454545454545303, 0.4568181818181818454, 0.4590909090909091050, 0.4613636363636363646, 0.4636363636363636243, 0.4659090909090908839, 0.4681818181818181990, 0.4704545454545454586, 0.4727272727272727182, 0.4749999999999999778, 0.4772727272727272929, 0.4795454545454545525, 0.4818181818181818121, 0.4840909090909090717, 0.4863636363636363869, 0.4886363636363636465, 0.4909090909090909061, 0.4931818181818181657, 0.4954545454545454808, 0.4977272727272727959, 0.5000000000000000000, 0.5022727272727273151, 0.5045454545454545192, 0.5068181818181818343, 0.5090909090909090384, 0.5113636363636363535, 0.5136363636363636687, 0.5159090909090908728, 0.5181818181818181879, 0.5204545454545455030, 0.5227272727272727071, 0.5250000000000000222, 0.5272727272727272263, 0.5295454545454545414, 0.5318181818181818565, 0.5340909090909090606, 0.5363636363636363757, 0.5386363636363636909, 0.5409090909090908950, 0.5431818181818182101, 0.5454545454545454142, 0.5477272727272727293, 0.5500000000000000444, 0.5522727272727272485, 0.5545454545454545636, 0.5568181818181817677, 0.5590909090909090828, 0.5613636363636363980, 0.5636363636363636020, 0.5659090909090909172, 0.5681818181818182323, 0.5704545454545454364, 0.5727272727272727515, 0.5749999999999999556, 0.5772727272727272707, 0.5795454545454545858, 0.5818181818181817899, 0.5840909090909089940, 0.5863636363636363091, 0.5886363636363636243, 0.5909090909090909394, 0.5931818181818181435, 0.5954545454545454586, 0.5977272727272727737, 0.5999999999999999778, 0.6022727272727272929, 0.6045454545454544970, 0.6068181818181818121, 0.6090909090909091272, 0.6113636363636363313, 0.6136363636363636465, 0.6159090909090909616, 0.6181818181818181657, 0.6204545454545454808, 0.6227272727272726849, 0.6250000000000000000, 0.6272727272727273151, 0.6295454545454545192, 0.6318181818181818343, 0.6340909090909090384, 0.6363636363636363535, 0.6386363636363636687, 0.6409090909090908728, 0.6431818181818181879, 0.6454545454545455030, 0.6477272727272727071, 0.6500000000000000222, 0.6522727272727272263, 0.6545454545454545414, 0.6568181818181818565, 0.6590909090909090606, 0.6613636363636363757, 0.6636363636363636909, 0.6659090909090908950, 0.6681818181818180991, 0.6704545454545454142, 0.6727272727272727293, 0.6750000000000000444, 0.6772727272727272485, 0.6795454545454545636, 0.6818181818181817677, 0.6840909090909090828, 0.6863636363636363980, 0.6886363636363636020, 0.6909090909090909172, 0.6931818181818182323, 0.6954545454545454364, 0.6977272727272727515, 0.6999999999999999556, 0.7022727272727272707, 0.7045454545454545858, 0.7068181818181817899, 0.7090909090909091050, 0.7113636363636363091, 0.7136363636363636243, 0.7159090909090909394, 0.7181818181818181435, 0.7204545454545454586, 0.7227272727272727737, 0.7249999999999999778, 0.7272727272727272929, 0.7295454545454544970, 0.7318181818181818121, 0.7340909090909091272, 0.7363636363636363313, 0.7386363636363636465, 0.7409090909090909616, 0.7431818181818181657, 0.7454545454545454808, 0.7477272727272726849, 0.7500000000000000000, 0.7522727272727273151, 0.7545454545454545192, 0.7568181818181818343, 0.7590909090909090384, 0.7613636363636363535, 0.7636363636363636687, 0.7659090909090908728, 0.7681818181818181879, 0.7704545454545455030, 0.7727272727272727071, 0.7750000000000000222, 0.7772727272727272263, 0.7795454545454545414, 0.7818181818181818565, 0.7840909090909090606, 0.7863636363636363757, 0.7886363636363636909, 0.7909090909090908950, 0.7931818181818182101, 0.7954545454545454142, 0.7977272727272727293, 0.8000000000000000444, 0.8022727272727272485, 0.8045454545454545636, 0.8068181818181817677, 0.8090909090909090828, 0.8113636363636363980, 0.8136363636363636020, 0.8159090909090909172, 0.8181818181818182323, 0.8204545454545454364, 0.8227272727272727515, 0.8249999999999999556, 0.8272727272727272707, 0.8295454545454545858, 0.8318181818181817899, 0.8340909090909091050, 0.8363636363636364202, 0.8386363636363636243, 0.8409090909090909394, 0.8431818181818181435, 0.8454545454545454586, 0.8477272727272727737, 0.8499999999999999778, 0.8522727272727272929, 0.8545454545454544970, 0.8568181818181818121, 0.8590909090909091272, 0.8613636363636363313, 0.8636363636363636465, 0.8659090909090909616, 0.8681818181818181657, 0.8704545454545454808, 0.8727272727272726849, 0.8750000000000000000, 0.8772727272727273151, 0.8795454545454545192, 0.8818181818181818343, 0.8840909090909090384, 0.8863636363636363535, 0.8886363636363636687, 0.8909090909090908728, 0.8931818181818181879, 0.8954545454545455030, 0.8977272727272727071, 0.9000000000000000222, 0.9022727272727272263, 0.9045454545454545414, 0.9068181818181818565, 0.9090909090909090606, 0.9113636363636363757, 0.9136363636363636909, 0.9159090909090908950, 0.9181818181818182101, 0.9204545454545453032, 0.9227272727272727293, 0.9250000000000000444, 0.9272727272727272485, 0.9295454545454545636, 0.9318181818181817677, 0.9340909090909090828, 0.9363636363636363980, 0.9386363636363636020, 0.9409090909090909172, 0.9431818181818182323, 0.9454545454545454364, 0.9477272727272727515, 0.9499999999999999556, 0.9522727272727272707, 0.9545454545454545858, 0.9568181818181817899, 0.9590909090909091050, 0.9613636363636363091, 0.9636363636363636243, 0.9659090909090909394, 0.9681818181818181435, 0.9704545454545454586, 0.9727272727272727737, 0.9749999999999999778, 0.9772727272727272929, 0.9779695260516495514 ),
 .UNSPECIFIED. ) 
 CURVE ( )  GEOMETRIC_REPRESENTATION_ITEM ( )  RATIONAL_B_SPLINE_CURVE ( ( 1.000000000000000000, 0.9898214418809326842, 1.000000000000000000, 0.9898214418809326842, 1.000000000000000000, 0.9898214418809326842, 1.000000000000000000, 0.9898214418809326842, 1.000000000000000000, 0.9898214418809326842, 1.000000000000000000, 0.9898214418809326842, 1.000000000000000000, 0.9898214418809326842, 1.000000000000000000, 0.9898214418809326842, 1.000000000000000000, 0.9898214418809326842, 1.000000000000000000, 0.9898214418809326842, 1.000000000000000000, 0.9898214418809326842, 1.000000000000000000, 0.9898214418809326842, 1.000000000000000000, 0.9898214418809326842, 1.000000000000000000, 0.9898214418809326842, 1.000000000000000000, 0.9898214418809326842, 1.000000000000000000, 0.9898214418809326842, 1.000000000000000000, 0.9898214418809326842, 1.000000000000000000, 0.9898214418809326842, 1.000000000000000000, 0.9898214418809326842, 1.000000000000000000, 0.9898214418809326842, 1.000000000000000000, 0.9898214418809326842, 1.000000000000000000, 0.9898214418809326842, 1.000000000000000000, 0.9898214418809326842, 1.000000000000000000, 0.9898214418809326842, 1.000000000000000000, 0.9898214418809326842, 1.000000000000000000, 0.9898214418809326842, 1.000000000000000000, 0.9898214418809326842, 1.000000000000000000, 0.9898214418809326842, 1.000000000000000000, 0.9898214418809326842, 1.000000000000000000, 0.9898214418809326842, 1.000000000000000000, 0.9898214418809326842, 1.000000000000000000, 0.9898214418809326842, 1.000000000000000000, 0.9898214418809326842, 1.000000000000000000, 0.9898214418809326842, 1.000000000000000000, 0.9898214418809326842, 1.000000000000000000, 0.9898214418809326842, 1.000000000000000000, 0.9898214418809326842, 1.000000000000000000, 0.9898214418809326842, 1.000000000000000000, 0.9898214418809326842, 1.000000000000000000, 0.9898214418809326842, 1.000000000000000000, 0.9898214418809326842, 1.000000000000000000, 0.9898214418809326842, 1.000000000000000000, 0.9898214418809326842, 1.000000000000000000, 0.9898214418809326842, 1.000000000000000000, 0.9898214418809326842, 1.000000000000000000, 0.9898214418809326842, 1.000000000000000000, 0.9898214418809326842, 1.000000000000000000, 0.9898214418809326842, 1.000000000000000000, 0.9898214418809326842, 1.000000000000000000, 0.9898214418809326842, 1.000000000000000000, 0.9898214418809326842, 1.000000000000000000, 0.9898214418809326842, 1.000000000000000000, 0.9898214418809326842, 1.000000000000000000, 0.9898214418809326842, 1.000000000000000000, 0.9898214418809326842, 1.000000000000000000, 0.9898214418809326842, 1.000000000000000000, 0.9898214418809326842, 1.000000000000000000, 0.9898214418809326842, 1.000000000000000000, 0.9898214418809326842, 1.000000000000000000, 0.9898214418809326842, 1.000000000000000000, 0.9898214418809326842, 1.000000000000000000, 0.9898214418809326842, 1.000000000000000000, 0.9898214418809326842, 1.000000000000000000, 0.9898214418809326842, 1.000000000000000000, 0.9898214418809326842, 1.000000000000000000, 0.9898214418809326842, 1.000000000000000000, 0.9898214418809326842, 1.000000000000000000, 0.9898214418809326842, 1.000000000000000000, 0.9898214418809326842, 1.000000000000000000, 0.9898214418809326842, 1.000000000000000000, 0.9898214418809326842, 1.000000000000000000, 0.9898214418809326842, 1.000000000000000000, 0.9898214418809326842, 1.000000000000000000, 0.9898214418809326842, 1.000000000000000000, 0.9898214418809326842, 1.000000000000000000, 0.9898214418809326842, 1.000000000000000000, 0.9898214418809326842, 1.000000000000000000, 0.9898214418809326842, 1.000000000000000000, 0.9898214418809326842, 1.000000000000000000, 0.9898214418809326842, 1.000000000000000000, 0.9898214418809326842, 1.000000000000000000, 0.9898214418809326842, 1.000000000000000000, 0.9898214418809326842, 1.000000000000000000, 0.9898214418809326842, 1.000000000000000000, 0.9898214418809326842, 1.000000000000000000, 0.9898214418809326842, 1.000000000000000000, 0.9898214418809326842, 1.000000000000000000, 0.9898214418809326842, 1.000000000000000000, 0.9898214418809326842, 1.000000000000000000, 0.9898214418809326842, 1.000000000000000000, 0.9898214418809326842, 1.000000000000000000, 0.9898214418809326842, 1.000000000000000000, 0.9898214418809326842, 1.000000000000000000, 0.9898214418809326842, 1.000000000000000000, 0.9898214418809326842, 1.000000000000000000, 0.9898214418809326842, 1.000000000000000000, 0.9898214418809326842, 1.000000000000000000, 0.9898214418809326842, 1.000000000000000000, 0.9898214418809326842, 1.000000000000000000, 0.9898214418809326842, 1.000000000000000000, 0.9898214418809326842, 1.000000000000000000, 0.9898214418809326842, 1.000000000000000000, 0.9898214418809326842, 1.000000000000000000, 0.9898214418809326842, 1.000000000000000000, 0.9898214418809326842, 1.000000000000000000, 0.9898214418809326842, 1.000000000000000000, 0.9898214418809326842, 1.000000000000000000, 0.9898214418809326842, 1.000000000000000000, 0.9898214418809326842, 1.000000000000000000, 0.9898214418809326842, 1.000000000000000000, 0.9898214418809326842, 1.000000000000000000, 0.9898214418809326842, 1.000000000000000000, 0.9898214418809326842, 1.000000000000000000, 0.9898214418809326842, 1.000000000000000000, 0.9898214418809326842, 1.000000000000000000, 0.9898214418809326842, 1.000000000000000000, 0.9898214418809326842, 1.000000000000000000, 0.9898214418809326842, 1.000000000000000000, 0.9898214418809326842, 1.000000000000000000, 0.9898214418809326842, 1.000000000000000000, 0.9898214418809326842, 1.000000000000000000, 0.9898214418809326842, 1.000000000000000000, 0.9898214418809326842, 1.000000000000000000, 0.9898214418809326842, 1.000000000000000000, 0.9898214418809326842, 1.000000000000000000, 0.9898214418809326842, 1.000000000000000000, 0.9898214418809326842, 1.000000000000000000, 0.9898214418809326842, 1.000000000000000000, 0.9898214418809326842, 1.000000000000000000, 0.9898214418809326842, 1.000000000000000000, 0.9898214418809326842, 1.000000000000000000, 0.9898214418809326842, 1.000000000000000000, 0.9898214418809326842, 1.000000000000000000, 0.9898214418809326842, 1.000000000000000000, 0.9898214418809326842, 1.000000000000000000, 0.9898214418809326842, 1.000000000000000000, 0.9898214418809326842, 1.000000000000000000, 0.9898214418809326842, 1.000000000000000000, 0.9898214418809326842, 1.000000000000000000, 0.9898214418809326842, 1.000000000000000000, 0.9898214418809326842, 1.000000000000000000, 0.9898214418809326842, 1.000000000000000000, 0.9898214418809326842, 1.000000000000000000, 0.9898214418809326842, 1.000000000000000000, 0.9898214418809326842, 1.000000000000000000, 0.9898214418809326842, 1.000000000000000000, 0.9898214418809326842, 1.000000000000000000, 0.9898214418809326842, 1.000000000000000000, 0.9898214418809326842, 1.000000000000000000, 0.9898214418809326842, 1.000000000000000000, 0.9898214418809326842, 1.000000000000000000, 0.9898214418809326842, 1.000000000000000000, 0.9898214418809326842, 1.000000000000000000, 0.9898214418809326842, 1.000000000000000000, 0.9898214418809326842, 1.000000000000000000, 0.9898214418809326842, 1.000000000000000000, 0.9898214418809326842, 1.000000000000000000, 0.9898214418809326842, 1.000000000000000000, 0.9898214418809326842, 1.000000000000000000, 0.9898214418809326842, 1.000000000000000000, 0.9898214418809326842, 1.000000000000000000, 0.9898214418809326842, 1.000000000000000000, 0.9898214418809326842, 1.000000000000000000, 0.9898214418809326842, 1.000000000000000000, 0.9898214418809326842, 1.000000000000000000, 0.9898214418809326842, 1.000000000000000000, 0.9898214418809326842, 1.000000000000000000, 0.9898214418809326842, 1.000000000000000000, 0.9898214418809326842, 1.000000000000000000, 0.9898214418809326842, 1.000000000000000000, 0.9898214418809326842, 1.000000000000000000, 0.9898214418809326842, 1.000000000000000000, 0.9898214418809326842, 1.000000000000000000, 0.9898214418809326842, 1.000000000000000000, 0.9898214418809326842, 1.000000000000000000, 0.9898214418809326842, 1.000000000000000000, 0.9898214418809326842, 1.000000000000000000, 0.9898214418809326842, 1.000000000000000000, 0.9898214418809326842, 1.000000000000000000, 0.9898214418809326842, 1.000000000000000000, 0.9898214418809326842, 1.000000000000000000, 0.9898214418809326842, 1.000000000000000000, 0.9898214418809326842, 1.000000000000000000, 0.9898214418809326842, 1.000000000000000000, 0.9898214418809326842, 1.000000000000000000, 0.9898214418809326842, 1.000000000000000000, 0.9898214418809326842, 1.000000000000000000, 0.9898214418809326842, 1.000000000000000000, 0.9898214418809326842, 1.000000000000000000, 0.9898214418809326842, 1.000000000000000000, 0.9898214418809326842, 1.000000000000000000, 0.9898214418809326842, 1.000000000000000000, 0.9898214418809326842, 1.000000000000000000, 0.9898214418809326842, 1.000000000000000000, 0.9898214418809326842, 1.000000000000000000, 0.9898214418809326842, 1.000000000000000000, 0.9898214418809326842, 1.000000000000000000, 0.9898214418809326842, 1.000000000000000000, 0.9898214418809326842, 1.000000000000000000, 0.9898214418809326842, 1.000000000000000000, 0.9898214418809326842, 1.000000000000000000, 0.9898214418809326842, 1.000000000000000000, 0.9898214418809326842, 1.000000000000000000, 0.9898214418809326842, 1.000000000000000000, 0.9898214418809326842, 1.000000000000000000, 0.9898214418809326842, 1.000000000000000000, 0.9898214418809326842, 1.000000000000000000, 0.9898214418809326842, 1.000000000000000000, 0.9898214418809326842, 1.000000000000000000, 0.9898214418809326842, 1.000000000000000000, 0.9898214418809326842, 1.000000000000000000, 0.9898214418809326842, 1.000000000000000000, 0.9898214418809326842, 1.000000000000000000, 0.9898214418809326842, 1.000000000000000000, 0.9898214418809326842, 1.000000000000000000, 0.9898214418809326842, 1.000000000000000000, 0.9898214418809326842, 1.000000000000000000, 0.9898214418809326842, 1.000000000000000000, 0.9898214418809326842, 1.000000000000000000, 0.9898214418809326842, 1.000000000000000000, 0.9898214418809326842, 1.000000000000000000, 0.9898214418809326842, 1.000000000000000000, 0.9898214418809326842, 1.000000000000000000, 0.9898214418809326842, 1.000000000000000000, 0.9898214418809326842, 1.000000000000000000, 0.9898214418809326842, 1.000000000000000000, 0.9898214418809326842, 1.000000000000000000, 0.9898214418809326842, 1.000000000000000000, 0.9898214418809326842, 1.000000000000000000, 0.9898214418809326842, 1.000000000000000000, 0.9898214418809326842, 1.000000000000000000, 0.9898214418809326842, 1.000000000000000000, 0.9898214418809326842, 1.000000000000000000, 0.9898214418809326842, 1.000000000000000000, 0.9898214418809326842, 1.000000000000000000, 0.9898214418809326842, 1.000000000000000000, 0.9898214418809326842, 1.000000000000000000, 0.9898214418809326842, 1.000000000000000000, 0.9898214418809326842, 1.000000000000000000, 0.9898214418809326842, 1.000000000000000000, 0.9898214418809326842, 1.000000000000000000, 0.9898214418809326842, 1.000000000000000000, 0.9898214418809326842, 1.000000000000000000, 0.9898214418809326842, 1.000000000000000000, 0.9898214418809326842, 1.000000000000000000, 0.9898214418809326842, 1.000000000000000000, 0.9898214418809326842, 1.000000000000000000, 0.9898214418809326842, 1.000000000000000000, 0.9898214418809326842, 1.000000000000000000, 0.9898214418809326842, 1.000000000000000000, 0.9898214418809326842, 1.000000000000000000, 0.9898214418809326842, 1.000000000000000000, 0.9898214418809326842, 1.000000000000000000, 0.9898214418809326842, 1.000000000000000000, 0.9898214418809326842, 1.000000000000000000, 0.9898214418809326842, 1.000000000000000000, 0.9898214418809326842, 1.000000000000000000, 0.9898214418809326842, 1.000000000000000000, 0.9898214418809326842, 1.000000000000000000, 0.9898214418809326842, 1.000000000000000000, 0.9898214418809326842, 1.000000000000000000, 0.9898214418809326842, 1.000000000000000000, 0.9898214418809326842, 1.000000000000000000, 0.9898214418809326842, 1.000000000000000000, 0.9898214418809326842, 1.000000000000000000, 0.9898214418809326842, 1.000000000000000000, 0.9898214418809326842, 1.000000000000000000, 0.9898214418809326842, 1.000000000000000000, 0.9898214418809326842, 1.000000000000000000, 0.9898214418809326842, 1.000000000000000000, 0.9898214418809326842, 1.000000000000000000, 0.9898214418809326842, 1.000000000000000000, 0.9898214418809326842, 1.000000000000000000, 0.9898214418809326842, 1.000000000000000000, 0.9898214418809326842, 1.000000000000000000, 0.9898214418809326842, 1.000000000000000000, 0.9898214418809326842, 1.000000000000000000, 0.9898214418809326842, 1.000000000000000000, 0.9898214418809326842, 1.000000000000000000, 0.9898214418809326842, 1.000000000000000000, 0.9898214418809326842, 1.000000000000000000, 0.9898214418809326842, 1.000000000000000000, 0.9898214418809326842, 1.000000000000000000, 0.9898214418809326842, 1.000000000000000000, 0.9898214418809326842, 1.000000000000000000, 0.9898214418809326842, 1.000000000000000000, 0.9898214418809326842, 1.000000000000000000, 0.9898214418809326842, 1.000000000000000000, 0.9898214418809326842, 1.000000000000000000, 0.9898214418809326842, 1.000000000000000000, 0.9898214418809326842, 1.000000000000000000, 0.9898214418809326842, 1.000000000000000000, 0.9898214418809326842, 1.000000000000000000, 0.9898214418809326842, 1.000000000000000000, 0.9898214418809326842, 1.000000000000000000, 0.9898214418809326842, 1.000000000000000000, 0.9898214418809326842, 1.000000000000000000, 0.9898214418809326842, 1.000000000000000000, 0.9898214418809326842, 1.000000000000000000, 0.9898214418809326842, 1.000000000000000000, 0.9898214418809326842, 1.000000000000000000, 0.9898214418809326842, 1.000000000000000000, 0.9898214418809326842, 1.000000000000000000, 0.9898214418809326842, 1.000000000000000000, 0.9898214418809326842, 1.000000000000000000, 0.9898214418809326842, 1.000000000000000000, 0.9898214418809326842, 1.000000000000000000, 0.9898214418809326842, 1.000000000000000000, 0.9898214418809326842, 1.000000000000000000, 0.9898214418809326842, 1.000000000000000000, 0.9898214418809326842, 1.000000000000000000, 0.9898214418809326842, 1.000000000000000000, 0.9898214418809326842, 1.000000000000000000, 0.9898214418809326842, 1.000000000000000000, 0.9898214418809326842, 1.000000000000000000, 0.9898214418809326842, 1.000000000000000000, 0.9898214418809326842, 1.000000000000000000, 0.9898214418809326842, 1.000000000000000000, 0.9898214418809326842, 1.000000000000000000, 0.9898214418809326842, 1.000000000000000000, 0.9898214418809326842, 1.000000000000000000, 0.9898214418809326842, 1.000000000000000000, 0.9898214418809326842, 1.000000000000000000, 0.9898214418809326842, 1.000000000000000000, 0.9898214418809326842, 1.000000000000000000, 0.9898214418809326842, 1.000000000000000000, 0.9898214418809326842, 1.000000000000000000, 0.9898214418809326842, 1.000000000000000000, 0.9898214418809326842, 1.000000000000000000, 0.9898214418809326842, 1.000000000000000000, 0.9898214418809326842, 1.000000000000000000, 0.9898214418809326842, 1.000000000000000000, 0.9898214418809326842, 1.000000000000000000, 0.9898214418809326842, 1.000000000000000000, 0.9898214418809326842, 1.000000000000000000, 0.9898214418809326842, 1.000000000000000000, 0.9898214418809326842, 1.000000000000000000, 0.9898214418809326842, 1.000000000000000000, 0.9898214418809326842, 1.000000000000000000, 0.9898214418809326842, 1.000000000000000000, 0.9898214418809326842, 1.000000000000000000, 0.9898214418809326842, 1.000000000000000000, 0.9898214418809326842, 1.000000000000000000, 0.9898214418809326842, 1.000000000000000000, 0.9898214418809326842, 1.000000000000000000, 0.9898214418809326842, 1.000000000000000000, 0.9898214418809326842, 1.000000000000000000, 0.9898214418809326842, 1.000000000000000000, 0.9898214418809326842, 1.000000000000000000, 0.9898214418809326842, 1.000000000000000000, 0.9898214418809326842, 1.000000000000000000, 0.9898214418809326842, 1.000000000000000000, 0.9898214418809326842, 1.000000000000000000, 0.9898214418809326842, 1.000000000000000000, 0.9898214418809326842, 1.000000000000000000, 0.9898214418809326842, 1.000000000000000000, 0.9898214418809326842, 1.000000000000000000, 0.9898214418809326842, 1.000000000000000000, 0.9898214418809326842, 1.000000000000000000, 0.9898214418809326842, 1.000000000000000000, 0.9898214418809326842, 1.000000000000000000, 0.9898214418809326842, 1.000000000000000000, 0.9898214418809326842, 1.000000000000000000, 0.9898214418809326842, 1.000000000000000000, 0.9898214418809326842, 1.000000000000000000, 0.9898214418809326842, 1.000000000000000000, 0.9898214418809326842, 1.000000000000000000, 0.9898214418809326842, 1.000000000000000000, 0.9898214418809326842, 1.000000000000000000, 0.9898214418809326842, 1.000000000000000000, 0.9898214418809326842, 1.000000000000000000, 0.9898214418809326842, 1.000000000000000000, 0.9898214418809326842, 1.000000000000000000, 0.9898214418809326842, 1.000000000000000000, 0.9898214418809326842, 1.000000000000000000, 0.9898214418809326842, 1.000000000000000000, 0.9898214418809326842, 1.000000000000000000, 0.9898214418809326842, 1.000000000000000000, 0.9898214418809326842, 1.000000000000000000, 0.9898214418809326842, 1.000000000000000000, 0.9898214418809326842, 1.000000000000000000, 0.9898214418809326842, 1.000000000000000000, 0.9898214418809326842, 1.000000000000000000, 0.9898214418809326842, 1.000000000000000000, 0.9898214418809326842, 1.000000000000000000, 0.9898214418809326842, 1.000000000000000000, 0.9898214418809326842, 1.000000000000000000, 0.9898214418809326842, 1.000000000000000000, 0.9898214418809326842, 1.000000000000000000, 0.9898214418809326842, 1.000000000000000000, 0.9898214418809326842, 1.000000000000000000, 0.9898214418809326842, 1.000000000000000000, 0.9898214418809326842, 1.000000000000000000, 0.9898214418809326842, 1.000000000000000000, 0.9898214418809326842, 1.000000000000000000, 0.9898214418809326842, 1.000000000000000000, 0.9898214418809326842, 1.000000000000000000, 0.9898214418809326842, 1.000000000000000000, 0.9898214418809326842, 1.000000000000000000, 0.9898214418809326842, 1.000000000000000000, 0.9898214418809326842, 1.000000000000000000, 0.9898214418809326842, 1.000000000000000000, 0.9898214418809326842, 1.000000000000000000, 0.9898214418809326842, 1.000000000000000000, 0.9898214418809326842, 1.000000000000000000, 0.9898214418809326842, 1.000000000000000000, 0.9898214418809326842, 1.000000000000000000, 0.9898214418809326842, 1.000000000000000000, 0.9898214418809326842, 1.000000000000000000, 0.9898214418809326842, 1.000000000000000000, 0.9898214418809326842, 1.000000000000000000, 0.9898214418809326842, 1.000000000000000000, 0.9898214418809326842, 1.000000000000000000, 0.9898214418809326842, 1.000000000000000000, 0.9898214418809326842, 1.000000000000000000, 0.9898214418809326842, 1.000000000000000000, 0.9898214418809326842, 1.000000000000000000, 0.9898214418809326842, 1.000000000000000000, 0.9898214418809326842, 1.000000000000000000, 0.9898214418809326842, 1.000000000000000000, 0.9898214418809326842, 1.000000000000000000, 0.9898214418809326842, 1.000000000000000000, 0.9898214418809326842, 1.000000000000000000, 0.9898214418809326842, 1.000000000000000000, 0.9898214418809326842, 1.000000000000000000, 0.9898214418809326842, 1.000000000000000000, 0.9898214418809326842, 1.000000000000000000, 0.9898214418809326842, 1.000000000000000000, 0.9898214418809326842, 1.000000000000000000, 0.9898214418809326842, 1.000000000000000000, 0.9968793409778355930, 0.9956722167842187998 ) ) 
 REPRESENTATION_ITEM ( '' )  );
#36165 = DIRECTION ( 'NONE',  ( -0.000000000000000000, -1.000000000000000000, -0.000000000000000000 ) ) ;
#36166 = CARTESIAN_POINT ( 'NONE',  ( 809.0717654672305343, -196.9181544815164386, -360.1688906516309885 ) ) ;
#36167 = DIRECTION ( 'NONE',  ( -1.880165489482579047E-16, -1.000000000000000000, -0.000000000000000000 ) ) ;
#36168 = DIRECTION ( 'NONE',  ( -0.000000000000000000, 1.000000000000000000, -0.000000000000000000 ) ) ;
#36169 = CARTESIAN_POINT ( 'NONE',  ( 804.4086373105744769, -409.6454272087884760, 333.3843516231986541 ) ) ;
#36170 = CARTESIAN_POINT ( 'NONE',  ( 781.2370466360911223, -356.7363362996978253, 304.9990715423533629 ) ) ;
#36171 = CARTESIAN_POINT ( 'NONE',  ( 796.7737145352015204, -236.6346026584198228, -370.7187646348536987 ) ) ;
#36172 = CARTESIAN_POINT ( 'NONE',  ( 791.4716058693660443, -452.9681489794448339, 367.7200696026887954 ) ) ;
#36173 = CARTESIAN_POINT ( 'NONE',  ( 755.0636971347428243, -4.270966294784170003, -341.7834795799807353 ) ) ;
#36174 = CARTESIAN_POINT ( 'NONE',  ( 747.6481478633932056, -181.0999726633347109, 353.4146539503763620 ) ) ;
#36175 = CARTESIAN_POINT ( 'NONE',  ( 805.9055244015594326, -99.62377810805098477, -315.8990559732753240 ) ) ;
#36176 = CARTESIAN_POINT ( 'NONE',  ( 745.0891759886404770, -124.2709662947837899, 342.4968714119734159 ) ) ;
#36177 = CARTESIAN_POINT ( 'NONE',  ( 755.2512626584698410, -391.5436935675101608, -315.2512626584710915 ) ) ;
#36178 = DIRECTION ( 'NONE',  ( 1.000000000000000000, 0.000000000000000000, 0.000000000000000000 ) ) ;
#36179 = DIRECTION ( 'NONE',  ( 0.000000000000000000, -0.3826834323650836756, -0.9238795325112892920 ) ) ;
#36180 = CARTESIAN_POINT ( 'NONE',  ( 788.8264449731200330, -213.1800572038743553, 363.6646147819171233 ) ) ;
#36181 = CARTESIAN_POINT ( 'NONE',  ( 786.2694204179717872, -453.2817908451519315, 305.1769319972829067 ) ) ;
#36182 = CARTESIAN_POINT ( 'NONE',  ( 751.2241431872005251, -424.1692326535044799, -359.9636004259367610 ) ) ;
#36183 = CARTESIAN_POINT ( 'NONE',  ( 805.6418435158337843, -5.463609026971610660, -363.8556311672236916 ) ) ;
#36184 = CARTESIAN_POINT ( 'NONE',  ( -598.8365100919716042, 240.0000000000001705, -199.9999999999899671 ) ) ;
#36185 = CARTESIAN_POINT ( 'NONE',  ( 805.9055244015594326, -27.62377810805120149, 315.8990559732753240 ) ) ;
#36186 = VERTEX_POINT ( 'NONE', #37818 ) ;
#36187 = CARTESIAN_POINT ( 'NONE',  ( 803.8651313633788504, -197.2601417444143124, -332.4468031744301015 ) ) ;
#36188 = CARTESIAN_POINT ( 'NONE',  ( 767.8955696845333705, -24.45278447660229304, 362.1676090361162323 ) ) ;
#36189 = CARTESIAN_POINT ( 'NONE',  ( 773.7943932421234194, -191.8055962898689017, -305.5313806188329409 ) ) ;
#36190 = CARTESIAN_POINT ( 'NONE',  ( 788.7631598425961101, -337.4419599262319593, 305.7194118038759143 ) ) ;
#36191 = CARTESIAN_POINT ( 'NONE',  ( 803.4237431249931660, -159.1800572038746111, 331.2633955100225194 ) ) ;
#36192 = ORIENTED_EDGE ( 'NONE', *, *, #32957, .F. ) ;
#36193 = CARTESIAN_POINT ( 'NONE',  ( 805.1927285166397041, -136.8164208402382371, -341.8018195045277707 ) ) ;
#36194 = CARTESIAN_POINT ( 'NONE',  ( 781.8018195045266339, -334.2709662947829656, 365.1927285166406705 ) ) ;
#36195 = CARTESIAN_POINT ( 'NONE',  ( 758.8095938919642549, -32.08914811296588709, -311.6929314249763365 ) ) ;
#36196 = EDGE_CURVE ( 'NONE', #26360, #15531, #6167, .T. ) ;
#36197 = ORIENTED_EDGE ( 'NONE', *, *, #23454, .T. ) ;
#36198 = CARTESIAN_POINT ( 'NONE',  ( 745.5313806188320314, -447.2817908451521021, -333.7943932421247268 ) ) ;
#36199 = ORIENTED_EDGE ( 'NONE', *, *, #27723, .F. ) ;
#36200 = CARTESIAN_POINT ( 'NONE',  ( 757.4527132478984868, -304.3726999360615082, -329.1273215169538844 ) ) ;
#36202 = CARTESIAN_POINT ( 'NONE',  ( 766.9102291470427417, -378.5545181178795247, 318.6633372737382501 ) ) ;
#36201 = CARTESIAN_POINT ( 'NONE',  ( 764.8639956371174549, -56.08914811296580893, 319.7806653035542013 ) ) ;
#36204 = CARTESIAN_POINT ( 'NONE',  ( 791.1614460488616487, -275.2601417444140566, 373.5763878283158874 ) ) ;
#36203 = CARTESIAN_POINT ( 'NONE',  ( 782.5225473063383106, -406.2709662947828519, 375.2698199232970637 ) ) ;
#36205 = CARTESIAN_POINT ( 'NONE',  ( 799.2566176426618085, -288.0090635724252479, -324.0069404352559559 ) ) ;
#36206 = CARTESIAN_POINT ( 'NONE',  ( 759.7806653035534055, -270.9982390220561115, -324.8639956371180801 ) ) ;
#36207 = DIRECTION ( 'NONE',  ( 1.000000000000000000, -0.000000000000000000, -0.000000000000000000 ) ) ;
#36208 = CARTESIAN_POINT ( 'NONE',  ( 774.6858677611749044, -153.7255117493291721, -315.5713283507209894 ) ) ;
#36209 = CARTESIAN_POINT ( 'NONE',  ( -78.83651009197140525, 260.0000000000000568, -202.7499999999934346 ) ) ;
#36210 = ORIENTED_EDGE ( 'NONE', *, *, #18266, .F. ) ;
#36211 = CARTESIAN_POINT ( 'NONE',  ( 777.4774526936600978, -442.2709662947826814, 304.7301800767027657 ) ) ;
#36213 = LINE ( 'NONE', #22335, #37374 ) ;
#36212 = CARTESIAN_POINT ( 'NONE',  ( 999.5857864376259840, -600.0000000000001137, 360.0000000000000000 ) ) ;
#36214 = CARTESIAN_POINT ( 'NONE',  ( 812.3518521366052028, -97.09997266333496668, -326.5853460496235243 ) ) ;
#36215 = DIRECTION ( 'NONE',  ( -0.000000000000000000, -0.000000000000000000, -1.000000000000000000 ) ) ;
#36216 = DIRECTION ( 'NONE',  ( -0.000000000000000000, 1.000000000000000000, -0.000000000000000000 ) ) ;
#36217 = EDGE_CURVE ( 'NONE', #2736, #38472, #45447, .T. ) ;
#36218 = CARTESIAN_POINT ( 'NONE',  ( 796.9571628226829034, -287.4636090269708575, 321.2382568024804641 ) ) ;
#36219 = CARTESIAN_POINT ( 'NONE',  ( 797.6776695296629214, -139.5436935675110135, 357.6776695296636603 ) ) ;
#36220 = ORIENTED_EDGE ( 'NONE', *, *, #44416, .F. ) ;
#36221 = CARTESIAN_POINT ( 'NONE',  ( 747.2067596250078623, -147.1800572038746395, -352.2312462859687230 ) ) ;
#36222 = CARTESIAN_POINT ( 'NONE',  ( 796.7845633553578182, -321.6237781080502600, 358.5707757039688204 ) ) ;
#36223 = DIRECTION ( 'NONE',  ( 8.659560562354932858E-17, 0.7071067811865474617, -0.7071067811865474617 ) ) ;
#36224 = CARTESIAN_POINT ( 'NONE',  ( 799.9636004259356241, -46.91815448151694312, 311.2241431872006956 ) ) ;
#36225 = CARTESIAN_POINT ( 'NONE',  ( 772.5602148656447525, -249.7255117493288594, -305.7998596910095443 ) ) ;
#36226 = EDGE_CURVE ( 'NONE', #45131, #27073, #19773, .T. ) ;
#36227 = CARTESIAN_POINT ( 'NONE',  ( 800.9747183278959710, -204.9982390220562820, 311.9810565676471583 ) ) ;
#36228 = CARTESIAN_POINT ( 'NONE',  ( 778.1981804954714335, -130.2709662947837899, 314.8072714833589885 ) ) ;
#36229 = LINE ( 'NONE', #14551, #15869 ) ;
#36230 = CARTESIAN_POINT ( 'NONE',  ( 807.5423716828161105, -297.0783235625957559, -362.2119215644372048 ) ) ;
#36231 = CARTESIAN_POINT ( 'NONE',  ( 786.5483106153019435, -31.64542720878970883, 364.1601925771022366 ) ) ;
#36232 = CARTESIAN_POINT ( 'NONE',  ( 796.7737145352015204, -356.6346026584193964, -370.7187646348536987 ) ) ;
#36233 = CYLINDRICAL_SURFACE ( 'NONE', #39485, 19.99999999999990763 ) ;
#36234 = CARTESIAN_POINT ( 'NONE',  ( 754.9735926884551418, -402.3510508353228374, 340.5236548041000333 ) ) ;
#36235 = VERTEX_POINT ( 'NONE', #2717 ) ;
#36236 = CARTESIAN_POINT ( 'NONE',  ( 804.6798772138708955, -423.7255117493281205, -334.6312213355107019 ) ) ;
#36237 = CARTESIAN_POINT ( 'NONE',  ( 774.6858677611749044, -225.7255117493289163, -315.5713283507209894 ) ) ;
#36238 = CARTESIAN_POINT ( 'NONE',  ( 803.8556311672234642, -81.62377810805104161, -365.6418435158340117 ) ) ;
#36240 = EDGE_CURVE ( 'NONE', #24825, #25236, #2473, .T. ) ;
#36239 = LINE ( 'NONE', #33027, #33652 ) ;
#36241 = CARTESIAN_POINT ( 'NONE',  ( 810.1134526219336749, -224.5328690171415076, 357.8822607201570349 ) ) ;
#36242 = CARTESIAN_POINT ( 'NONE',  ( 805.1927285166399315, -40.81642084023859951, 341.8018195045277707 ) ) ;
#36243 = EDGE_CURVE ( 'NONE', #577, #43693, #42197, .T. ) ;
#36244 = CARTESIAN_POINT ( 'NONE',  ( 772.3691319403857278, -239.2601417444141987, -315.8894580844506663 ) ) ;
#36245 = CARTESIAN_POINT ( 'NONE',  ( 797.8594530101008786, -229.5436935675106440, 322.1405469898980982 ) ) ;
#36246 = EDGE_LOOP ( 'NONE', ( #3419, #42728 ) ) ;
#36247 = CARTESIAN_POINT ( 'NONE',  ( 746.0683387631852383, -67.44195992623289726, -331.3260364891676204 ) ) ;
#36248 = ADVANCED_FACE ( 'NONE', ( #31106 ), #13807, .F. ) ;
#36249 = CARTESIAN_POINT ( 'NONE',  ( 809.0082352070306797, -452.9681489794448908, -335.5949598064873385 ) ) ;
#36250 = ORIENTED_EDGE ( 'NONE', *, *, #37961, .F. ) ;
#36251 = CARTESIAN_POINT ( 'NONE',  ( 814.2805881961230625, -337.6454272087888171, -331.2368401574024119 ) ) ;
#36252 = CARTESIAN_POINT ( 'NONE',  ( 755.2512626584698410, -295.5436935675105588, 315.2512626584710915 ) ) ;
#36253 = CARTESIAN_POINT ( 'NONE',  ( 800.1688906516307043, -10.16923265350579442, 369.0717654672308186 ) ) ;
#36254 = CARTESIAN_POINT ( 'NONE',  ( 804.4086373105744769, -169.6454272087892718, -333.3843516231986541 ) ) ;
#36255 = CARTESIAN_POINT ( 'NONE',  ( 774.6858677611749044, -177.7255117493290868, -315.5713283507209894 ) ) ;
#36256 = VECTOR ( 'NONE', #9972, 1000.000000000000000 ) ;
#36257 = CARTESIAN_POINT ( 'NONE',  ( 797.8594530101009923, -373.5436935675102177, -322.1405469898982119 ) ) ;
#36258 = ORIENTED_EDGE ( 'NONE', *, *, #24682, .F. ) ;
#36259 = CARTESIAN_POINT ( 'NONE',  ( 802.7791456095903868, 19.28531280103956647, -329.0155153010375102 ) ) ;
#36260 = ORIENTED_EDGE ( 'NONE', *, *, #2706, .T. ) ;
#36261 = CARTESIAN_POINT ( 'NONE',  ( 810.7187646348534145, -330.4527844766013231, 356.7737145352016341 ) ) ;
#36262 = ADVANCED_FACE ( 'NONE', ( #30891 ), #13566, .F. ) ;
#36263 = DIRECTION ( 'NONE',  ( 0.000000000000000000, 0.000000000000000000, 1.000000000000000000 ) ) ;
#36264 = CARTESIAN_POINT ( 'NONE',  ( 804.6971507214547046, -219.2817908451527558, 344.0799538623459739 ) ) ;
#36265 = VECTOR ( 'NONE', #9641, 1000.000000000000000 ) ;
#36266 = CARTESIAN_POINT ( 'NONE',  ( 805.1016975059191054, -366.8965053807773984, 343.0745993439771837 ) ) ;
#36267 = LINE ( 'NONE', #18954, #29040 ) ;
#36268 = EDGE_CURVE ( 'NONE', #1111, #9315, #9455, .T. ) ;
#36269 = CARTESIAN_POINT ( 'NONE',  ( 804.8461984189677878, -194.1908817542437475, 336.9566956441385628 ) ) ;
#36270 = CARTESIAN_POINT ( 'NONE',  ( 802.1676090361156639, -62.63460265842031305, 327.8955696845344505 ) ) ;
#36271 = ORIENTED_EDGE ( 'NONE', *, *, #14169, .F. ) ;
#36272 = CARTESIAN_POINT ( 'NONE',  ( 805.6418435158337843, -413.4636090269704027, -363.8556311672236916 ) ) ;
#36273 = CARTESIAN_POINT ( 'NONE',  ( 777.5031285880264704, 1.183579159761269040, -374.9108240113588408 ) ) ;
#36274 = CARTESIAN_POINT ( 'NONE',  ( 745.7194118038753459, -253.6454272087889876, 348.7631598425976449 ) ) ;
#36275 = CARTESIAN_POINT ( 'NONE',  ( 798.7617431975189675, -219.6237781080506295, 323.0428371773161871 ) ) ;
#36276 = CARTESIAN_POINT ( 'NONE',  ( 781.8018195045266339, -406.2709662947829088, -365.1927285166406705 ) ) ;
#36277 = LINE ( 'NONE', #4202, #35643 ) ;
#36278 = CARTESIAN_POINT ( 'NONE',  ( 774.6858677611749044, 14.27448825067031812, 315.5713283507209894 ) ) ;
#36279 = LINE ( 'NONE', #8124, #3089 ) ;
#36280 = CARTESIAN_POINT ( 'NONE',  ( 786.5483106153019435, -247.6454272087890160, -364.1601925771022366 ) ) ;
#36281 = ADVANCED_FACE ( 'NONE', ( #10324 ), #34546, .F. ) ;
#36282 = CARTESIAN_POINT ( 'NONE',  ( 749.2812353651451076, -54.45278447660219001, 323.2262854647983090 ) ) ;
#36283 = CARTESIAN_POINT ( 'NONE',  ( 763.0537975583475827, -120.4527844766019484, 371.0346526505627480 ) ) ;
#36284 = DIRECTION ( 'NONE',  ( 1.000000000000000000, 4.625929269271485914E-16, 0.000000000000000000 ) ) ;
#36285 = CARTESIAN_POINT ( 'NONE',  ( 190.7583438952258916, 294.6698570112193920, -274.9999999999999432 ) ) ;
#36286 = CARTESIAN_POINT ( 'NONE',  ( 804.1009440267234822, -383.4636090269704596, 314.0944755984392600 ) ) ;
#36287 = CARTESIAN_POINT ( 'NONE',  ( -468.8365100919714337, 260.0000000000001705, -199.9999999999908766 ) ) ;
#36288 = CARTESIAN_POINT ( 'NONE',  ( 814.5518280994195948, -375.7255117493283478, 332.4837098697145734 ) ) ;
#36289 = CARTESIAN_POINT ( 'NONE',  ( 788.8264449731200330, -309.1800572038740711, -363.6646147819171233 ) ) ;
#36290 = CARTESIAN_POINT ( 'NONE',  ( 803.4237431249931660, -423.1800572038737300, 331.2633955100225194 ) ) ;
#36291 = CIRCLE ( 'NONE', #41473, 8.000000000000007105 ) ;
#36292 = CARTESIAN_POINT ( 'NONE',  ( 779.4763451958990572, -176.7363362996983369, 365.0264073115438919 ) ) ;
#36293 = CARTESIAN_POINT ( 'NONE',  ( 814.8207195650702488, -74.19088175424410281, -336.2433038121456548 ) ) ;
#36294 = CARTESIAN_POINT ( 'NONE',  ( 754.9735926884551418, -114.3510508353236617, -340.5236548041000333 ) ) ;
#36295 = CARTESIAN_POINT ( 'NONE',  ( 766.5853460496234675, -133.9874144716872024, 372.3518521366060554 ) ) ;
#36296 = CARTESIAN_POINT ( 'NONE',  ( 785.3141322388236176, -429.7255117493282910, 364.4286716492789537 ) ) ;
#36297 = ADVANCED_FACE ( 'NONE', ( #20932 ), #35029, .F. ) ;
#36298 = CARTESIAN_POINT ( 'NONE',  ( 767.8955696845333705, -24.45278447660229304, -362.1676090361162323 ) ) ;
#36299 = CARTESIAN_POINT ( 'NONE',  ( 772.3691319403857278, -143.2601417444144829, -315.8894580844506663 ) ) ;
#36300 = CARTESIAN_POINT ( 'NONE',  ( 785.3141322388236176, -93.72551174932934259, -364.4286716492789537 ) ) ;
#36301 = CARTESIAN_POINT ( 'NONE',  ( 754.9735926884551418, -426.3510508353226669, -340.5236548041000333 ) ) ;
#36303 = CARTESIAN_POINT ( 'NONE',  ( 781.7834795799800531, -250.8164208402379245, 315.0636971347436202 ) ) ;
#36302 = CARTESIAN_POINT ( 'NONE',  ( 756.3353852180819104, -245.9073299311469896, 331.1735550268788302 ) ) ;
#36304 = DIRECTION ( 'NONE',  ( 0.000000000000000000, 0.000000000000000000, -1.000000000000000000 ) ) ;
#36305 = ORIENTED_EDGE ( 'NONE', *, *, #24982, .T. ) ;
#36306 = CARTESIAN_POINT ( 'NONE',  ( 805.1927285166397041, -448.8164208402371855, 341.8018195045277707 ) ) ;
#36307 = ORIENTED_EDGE ( 'NONE', *, *, #25787, .T. ) ;
#36308 = CARTESIAN_POINT ( 'NONE',  ( 777.5031285880264704, -190.8164208402381234, 374.9108240113588408 ) ) ;
#36309 = CARTESIAN_POINT ( 'NONE',  ( 763.0428371773158460, -275.4636090269708575, 358.7617431975195359 ) ) ;
#36310 = VERTEX_POINT ( 'NONE', #41752 ) ;
#36311 = CARTESIAN_POINT ( 'NONE',  ( 772.4468031744293057, -81.82724539060772884, -363.8651313633793620 ) ) ;
#36312 = AXIS2_PLACEMENT_3D ( 'NONE', #40141, #15222, #33424 ) ;
#36313 = CARTESIAN_POINT ( 'NONE',  ( 758.0141637701419768, -207.0783235625960685, 367.2620300519063790 ) ) ;
#36314 = CARTESIAN_POINT ( 'NONE',  ( 805.1927285166399315, -280.8164208402378108, -341.8018195045277707 ) ) ;
#36315 = ORIENTED_EDGE ( 'NONE', *, *, #37373, .T. ) ;
#36316 = CARTESIAN_POINT ( 'NONE',  ( 762.1405469898971887, -385.5436935675102745, -357.8594530101015607 ) ) ;
#36317 = CARTESIAN_POINT ( 'NONE',  ( 804.6798772138708955, -63.72551174932939233, -334.6312213355107019 ) ) ;
#36318 = EDGE_CURVE ( 'NONE', #19003, #28399, #10103, .T. ) ;
#36319 = CARTESIAN_POINT ( 'NONE',  ( 760.5453621957607311, -261.0783235625959264, 323.8424801807151425 ) ) ;
#36320 = DIRECTION ( 'NONE',  ( -0.000000000000000000, 1.000000000000000000, -0.000000000000000000 ) ) ;
#36321 = LINE ( 'NONE', #544, #10851 ) ;
#36322 = ADVANCED_FACE ( 'NONE', ( #14941 ), #25559, .F. ) ;
#36323 = CARTESIAN_POINT ( 'NONE',  ( 810.4231160770870019, -24.55451811788064020, -321.9338519418446936 ) ) ;
#36324 = CARTESIAN_POINT ( 'NONE',  ( 829.9999999999992042, 529.9999999999997726, -360.0000000000000000 ) ) ;
#36325 = ORIENTED_EDGE ( 'NONE', *, *, #18811, .F. ) ;
#36326 = CARTESIAN_POINT ( 'NONE',  ( 776.2046728542105711, -308.1908817542434349, -304.8212110874238761 ) ) ;
#36327 = VECTOR ( 'NONE', #13275, 1000.000000000000000 ) ;
#36328 = CARTESIAN_POINT ( 'NONE',  ( 776.2046728542105711, -164.1908817542438612, 304.8212110874238761 ) ) ;
#36330 = CARTESIAN_POINT ( 'NONE',  ( 792.1044303154645831, -252.4527844766015789, -317.8323909638837677 ) ) ;
#36329 = CARTESIAN_POINT ( 'NONE',  ( 200.7583438952259485, 394.6698570112193920, -224.9999999999999716 ) ) ;
#36331 = CARTESIAN_POINT ( 'NONE',  ( 772.4999999999993179, -462.9681489794448339, -370.0000000000000568 ) ) ;
#36332 = CARTESIAN_POINT ( 'NONE',  ( 798.5707757039680246, -149.4636090269711417, -356.7845633553585003 ) ) ;
#36333 = PRODUCT_DEFINITION ( 'UNKNOWN', '', #25299, #38575 ) ;
#36334 = LINE ( 'NONE', #32433, #12153 ) ;
#36335 = CARTESIAN_POINT ( 'NONE',  ( 788.7631598425961101, -25.44195992623301450, -305.7194118038759143 ) ) ;
#36336 = CARTESIAN_POINT ( 'NONE',  ( 796.7737145352015204, -356.6346026584193964, -370.7187646348536987 ) ) ;
#36337 = CARTESIAN_POINT ( 'NONE',  ( -789.9999999999989768, 240.0000000000000853, -360.0000000000000000 ) ) ;
#36338 = CARTESIAN_POINT ( 'NONE',  ( 757.8323909638827445, -2.634602658420536869, 352.1044303154654358 ) ) ;
#36339 = CARTESIAN_POINT ( 'NONE',  ( 791.0478386215596629, -285.8272453906071178, 306.7653713866226326 ) ) ;
#36340 = CARTESIAN_POINT ( 'NONE',  ( 756.1443688327750579, -237.6237781080505442, -314.3581564841659315 ) ) ;
#36341 = CARTESIAN_POINT ( 'NONE',  ( 767.7687537140311633, -263.9073299311469327, 372.7932403749916830 ) ) ;
#36342 = CARTESIAN_POINT ( 'NONE',  ( 795.6651683502461765, -442.7146871989589840, -371.3240766477733814 ) ) ;
#36343 = FACE_BOUND ( 'NONE', #6189, .T. ) ;
#36344 = ORIENTED_EDGE ( 'NONE', *, *, #10062, .F. ) ;
#36345 = CARTESIAN_POINT ( 'NONE',  ( 755.0636971347428243, -340.2709662947831362, 341.7834795799807353 ) ) ;
#36346 = VECTOR ( 'NONE', #20698, 1000.000000000000000 ) ;
#36347 = CARTESIAN_POINT ( 'NONE',  ( 761.4292242960306112, -89.46360902697134065, 323.2154366446414429 ) ) ;
#36348 = CARTESIAN_POINT ( 'NONE',  ( 796.7845633553578182, -9.623778108051251223, -358.5707757039688204 ) ) ;
#36349 = FACE_BOUND ( 'NONE', #12842, .T. ) ;
#36350 = DIRECTION ( 'NONE',  ( 0.000000000000000000, -0.6755902076156505842, -0.7372773368101328550 ) ) ;
#36351 = CARTESIAN_POINT ( 'NONE',  ( 807.5423716828161105, -129.0783235625963243, 362.2119215644372048 ) ) ;
#36353 = CARTESIAN_POINT ( 'NONE',  ( 778.2165204200184689, -382.8164208402374697, 364.9363028652563230 ) ) ;
#36352 = CARTESIAN_POINT ( 'NONE',  ( 783.0433043558608688, -168.8965053807780237, 315.1538015810313027 ) ) ;
#36354 = ORIENTED_EDGE ( 'NONE', *, *, #11174, .T. ) ;
#36355 = CARTESIAN_POINT ( 'NONE',  ( 804.9511171171677688, -341.8055962898683333, -335.8780910478229202 ) ) ;
#36356 = CARTESIAN_POINT ( 'NONE',  ( 804.6798772138708955, -159.7255117493291436, 334.6312213355107019 ) ) ;
#36357 = CARTESIAN_POINT ( 'NONE',  ( 776.2433038121456548, -324.8965053807775121, -374.8207195650711014 ) ) ;
#36358 = CARTESIAN_POINT ( 'NONE',  ( -26.63011601220122060, -544.8427095258973623, -350.0000000000000000 ) ) ;
#36359 = CARTESIAN_POINT ( 'NONE',  ( 783.7566961878529810, -432.8965053807771142, 305.1792804349288417 ) ) ;
#36360 = EDGE_LOOP ( 'NONE', ( #27232, #8824, #21598, #10029 ) ) ;
#36361 = CARTESIAN_POINT ( 'NONE',  ( 767.8955696845333705, -360.4527844766010958, 362.1676090361162323 ) ) ;
#36362 = CARTESIAN_POINT ( 'NONE',  ( 759.2295555964440155, -64.16923265350563099, -353.9708237608231229 ) ) ;
#36363 = ORIENTED_EDGE ( 'NONE', *, *, #37672, .F. ) ;
#36364 = CARTESIAN_POINT ( 'NONE',  ( 800.2193346964447755, -426.9982390220554862, 355.1360043628815788 ) ) ;
#36365 = CARTESIAN_POINT ( 'NONE',  ( 747.2067596250078623, -195.1800572038744974, -352.2312462859687230 ) ) ;
#36366 = VERTEX_POINT ( 'NONE', #39433 ) ;
#36367 = CARTESIAN_POINT ( 'NONE',  ( 804.4286716492782716, -185.3618753856926844, -345.3141322388244703 ) ) ;
#36368 = ORIENTED_EDGE ( 'NONE', *, *, #27299, .F. ) ;
#36369 = CARTESIAN_POINT ( 'NONE',  ( 773.4516893846965786, -427.6454272087885897, -315.8398074228977066 ) ) ;
#36370 = CARTESIAN_POINT ( 'NONE',  ( 805.2837595273609850, -458.7363362996973706, 340.5290396650784714 ) ) ;
#36371 = CARTESIAN_POINT ( 'NONE',  ( 747.2067596250078623, -219.1800572038744122, 352.2312462859687230 ) ) ;
#36372 = CARTESIAN_POINT ( 'NONE',  ( 804.9511171171677688, -149.8055962898689870, 335.8780910478229202 ) ) ;
#36374 = DIRECTION ( 'NONE',  ( 0.000000000000000000, 0.000000000000000000, 1.000000000000000000 ) ) ;
#36373 = CARTESIAN_POINT ( 'NONE',  ( 999.9999999999992042, 249.5857864376267798, -359.5857864376268935 ) ) ;
#36375 = ORIENTED_EDGE ( 'NONE', *, *, #32907, .F. ) ;
#36376 = CARTESIAN_POINT ( 'NONE',  ( 790.0220218866281812, -415.0999726633340288, -363.2186876482849129 ) ) ;
#36377 = CARTESIAN_POINT ( 'NONE',  ( 919.9999999999993179, 154.9999999999998863, -350.0000000000000000 ) ) ;
#36378 = CIRCLE ( 'NONE', #214, 19.99999999999990763 ) ;
#36379 = CARTESIAN_POINT ( 'NONE',  ( 746.4236121716829757, -207.8272453906073451, -328.8385539511384650 ) ) ;
#36380 = CARTESIAN_POINT ( 'NONE',  ( 745.5313806188320314, -63.28179084515324604, 333.7943932421247268 ) ) ;
#36382 = CYLINDRICAL_SURFACE ( 'NONE', #24739, 9.999999999999980460 ) ;
#36381 = DIRECTION ( 'NONE',  ( 0.000000000000000000, 0.000000000000000000, 1.000000000000000000 ) ) ;
#36383 = CARTESIAN_POINT ( 'NONE',  ( 805.1016975059191054, -318.8965053807775121, -343.0745993439771837 ) ) ;
#36384 = CARTESIAN_POINT ( 'NONE',  ( 794.9999999999993179, 205.0000000000000568, -255.0000000000000000 ) ) ;
#36385 = CARTESIAN_POINT ( 'NONE',  ( 814.4686193811664907, -171.2817908451529263, -346.2056067578752732 ) ) ;
#36386 = DIRECTION ( 'NONE',  ( 0.000000000000000000, 0.000000000000000000, 1.000000000000000000 ) ) ;
#36387 = CARTESIAN_POINT ( 'NONE',  ( 441.1634899080286232, 239.9999999999999716, -199.9999999999972431 ) ) ;
#36388 = CARTESIAN_POINT ( 'NONE',  ( 796.9571628226829034, -407.4636090269703459, 321.2382568024804641 ) ) ;
#36389 = CARTESIAN_POINT ( 'NONE',  ( 814.9108240113580450, -256.2709662947834204, -337.5031285880265273 ) ) ;
#36390 = CARTESIAN_POINT ( 'NONE',  ( 757.4527132478984868, -232.3726999360617924, 329.1273215169538844 ) ) ;
#36391 = PLANE ( 'NONE',  #39396 ) ;
#36392 = CARTESIAN_POINT ( 'NONE',  ( 759.7806653035534055, -6.998239022056885972, -324.8639956371180801 ) ) ;
#36393 = CIRCLE ( 'NONE', #15007, 9.999999999999980460 ) ;
#36394 = CARTESIAN_POINT ( 'NONE',  ( 795.8262568251477660, -190.3726999360619629, 308.3538107759623585 ) ) ;
#36395 = CARTESIAN_POINT ( 'NONE',  ( 756.1443688327750579, -117.6237781080509279, -314.3581564841659315 ) ) ;
#36396 = CARTESIAN_POINT ( 'NONE',  ( 801.1904061080336987, -116.0891481129656029, 368.3070685750235498 ) ) ;
#36397 = CARTESIAN_POINT ( 'NONE',  ( 782.5225473063381969, -382.2709662947828519, -375.2698199232970637 ) ) ;
#36398 = DIRECTION ( 'NONE',  ( 1.000000000000000000, 0.000000000000000000, 0.000000000000000000 ) ) ;
#36399 = DIRECTION ( 'NONE',  ( -1.000000000000000000, -0.000000000000000000, -0.000000000000000000 ) ) ;
#36400 = CARTESIAN_POINT ( 'NONE',  ( 759.7806653035534055, -222.9982390220561399, 324.8639956371180801 ) ) ;
#36401 = CARTESIAN_POINT ( 'NONE',  ( 766.0291762391763086, -34.91815448151697154, 360.7704444035551319 ) ) ;
#36402 = CARTESIAN_POINT ( 'NONE',  ( 778.2165204200184689, -382.8164208402374697, -364.9363028652563230 ) ) ;
#36403 = CARTESIAN_POINT ( 'NONE',  ( 810.4231160770870019, -0.5545181178807169209, -321.9338519418446936 ) ) ;
#36404 = DIRECTION ( 'NONE',  ( -1.000000000000000000, -0.000000000000000000, -0.000000000000000000 ) ) ;
#36405 = CARTESIAN_POINT ( 'NONE',  ( 801.9858362298568863, -27.07832356259665474, 312.7379699480935642 ) ) ;
#36406 = ORIENTED_EDGE ( 'NONE', *, *, #38814, .F. ) ;
#36407 = APPLICATION_CONTEXT ( 'automotive_design' ) ;
#36408 = CARTESIAN_POINT ( 'NONE',  ( 787.6308680596127942, -179.2601417444143692, -364.1105419155492768 ) ) ;
#36409 = AXIS2_PLACEMENT_3D ( 'NONE', #17983, #38776, #32053 ) ;
#36410 = CARTESIAN_POINT ( 'NONE',  ( 781.7834795799800531, -34.81642084023861372, 315.0636971347436202 ) ) ;
#36411 = CARTESIAN_POINT ( 'NONE',  ( 749.8865473780648472, -212.5328690171415076, -322.1177392798429082 ) ) ;
#36412 = DIRECTION ( 'NONE',  ( 0.000000000000000000, 0.000000000000000000, 1.000000000000000000 ) ) ;
#36413 = CARTESIAN_POINT ( 'NONE',  ( 749.8865473780648472, -356.5328690171410813, 322.1177392798429082 ) ) ;
#36414 = VECTOR ( 'NONE', #31382, 1000.000000000000000 ) ;
#36415 = EDGE_LOOP ( 'NONE', ( #25852, #11886 ) ) ;
#36416 = CARTESIAN_POINT ( 'NONE',  ( 748.3538107759620743, -424.7146871989589840, 355.8262568251490165 ) ) ;
#36417 = CARTESIAN_POINT ( 'NONE',  ( 762.1405469898971887, -337.5436935675102177, 357.8594530101015607 ) ) ;
#36418 = CARTESIAN_POINT ( 'NONE',  ( 804.7487373415286811, -91.54369356751116982, -364.7487373415288516 ) ) ;
#36419 = ORIENTED_EDGE ( 'NONE', *, *, #13993, .T. ) ;
#36420 = CARTESIAN_POINT ( 'NONE',  ( 755.8894580844503253, -15.82724539060794200, -332.3691319403863531 ) ) ;
#36421 = ORIENTED_EDGE ( 'NONE', *, *, #20102, .T. ) ;
#36422 = CARTESIAN_POINT ( 'NONE',  ( 769.9779781133707957, -331.0999726633342561, -316.7813123517150871 ) ) ;
#36423 = VECTOR ( 'NONE', #28495, 1000.000000000000000 ) ;
#36425 = CARTESIAN_POINT ( 'NONE',  ( 769.9779781133707957, -355.0999726633341993, 316.7813123517150871 ) ) ;
#36424 = CARTESIAN_POINT ( 'NONE',  ( 785.3141322388236176, -45.72551174932949181, 364.4286716492789537 ) ) ;
#36426 = CARTESIAN_POINT ( 'NONE',  ( 802.1676090361156639, -302.6346026584196238, -327.8955696845344505 ) ) ;
#36428 = CARTESIAN_POINT ( 'NONE',  ( 759.8311093483677041, -334.1692326535047073, 310.9282345327691814 ) ) ;
#36427 = CARTESIAN_POINT ( 'NONE',  ( 810.7187646348534145, -402.4527844766010389, 356.7737145352016341 ) ) ;
#36429 = CARTESIAN_POINT ( 'NONE',  ( 755.1538015810308480, -302.1908817542433781, -343.0433043558613804 ) ) ;
#36430 = CARTESIAN_POINT ( 'NONE',  ( 778.1981804954714335, -298.2709662947830793, -314.8072714833589885 ) ) ;
#36431 = LINE ( 'NONE', #2390, #3661 ) ;
#36432 = CARTESIAN_POINT ( 'NONE',  ( 756.3353852180819104, -149.9073299311473875, -331.1735550268788302 ) ) ;
#36433 = EDGE_CURVE ( 'NONE', #11158, #44330, #28321, .T. ) ;
#36434 = CARTESIAN_POINT ( 'NONE',  ( -39.63011601220123481, -513.1383975375929367, -369.9999999999999432 ) ) ;
#36435 = CARTESIAN_POINT ( 'NONE',  ( 744.7301800767019131, -412.8164208402372992, 337.4774526936615757 ) ) ;
#36437 = CYLINDRICAL_SURFACE ( 'NONE', #20388, 10.00000000000000888 ) ;
#36436 = DIRECTION ( 'NONE',  ( 1.000000000000000000, -0.000000000000000000, -0.000000000000000000 ) ) ;
#36438 = CARTESIAN_POINT ( 'NONE',  ( 795.8262568251477660, -94.37269993606224716, -308.3538107759623585 ) ) ;
#36439 = CARTESIAN_POINT ( 'NONE',  ( 989.9999999999992042, -179.7356316342496712, -69.11609595480017276 ) ) ;
#36440 = DIRECTION ( 'NONE',  ( -0.000000000000000000, -0.000000000000000000, 1.000000000000000000 ) ) ;
#36441 = CARTESIAN_POINT ( 'NONE',  ( 802.5472867521000353, -292.3726999360616219, 350.8726784830461156 ) ) ;
#36442 = CARTESIAN_POINT ( 'NONE',  ( 800.2193346964447755, -138.9982390220563957, 355.1360043628815788 ) ) ;
#36443 = ORIENTED_EDGE ( 'NONE', *, *, #30014, .T. ) ;
#36444 = AXIS2_PLACEMENT_3D ( 'NONE', #12812, #23429, #26893 ) ;
#36445 = AXIS2_PLACEMENT_3D ( 'NONE', #18796, #15337, #39832 ) ;
#36446 = CARTESIAN_POINT ( 'NONE',  ( 746.8695393053151292, -125.9073299311474159, -327.6429770376306578 ) ) ;
#36447 = CARTESIAN_POINT ( 'NONE',  ( 800.7704444035546203, -340.1692326535047641, 326.0291762391768771 ) ) ;
#36448 = PLANE ( 'NONE',  #24871 ) ;
#36449 = CARTESIAN_POINT ( 'NONE',  ( 805.1016975059191054, -438.8965053807771710, -343.0745993439771837 ) ) ;
#36450 = CARTESIAN_POINT ( 'NONE',  ( 754.3581564841646241, -65.46360902697142592, 316.1443688327762516 ) ) ;
#36451 = CARTESIAN_POINT ( 'NONE',  ( 782.4968714119720516, -274.8164208402378108, -305.0891759886411023 ) ) ;
#36452 = ADVANCED_FACE ( 'NONE', ( #35486 ), #842, .T. ) ;
#36453 = CARTESIAN_POINT ( 'NONE',  ( 808.3070685750230950, -210.9982390220561967, 361.1904061080339261 ) ) ;
#36454 = CARTESIAN_POINT ( 'NONE',  ( 755.3201227861273992, -123.7255117493292147, 345.3687786644892981 ) ) ;
#36455 = CARTESIAN_POINT ( 'NONE',  ( 793.4146539503750546, -25.98741447168755769, -307.6481478633938877 ) ) ;
#36456 = VERTEX_POINT ( 'NONE', #7787 ) ;
#36457 = CARTESIAN_POINT ( 'NONE',  ( 786.2056067578752163, -299.8055962898685038, -374.4686193811670023 ) ) ;
#36458 = CONICAL_SURFACE ( 'NONE', #13614, 8.024999999999948841, 0.7853981633974337351 ) ;
#36459 = CARTESIAN_POINT ( 'NONE',  ( 757.0176451133909268, -13.09997266333522248, 349.9200121543848354 ) ) ;
#36460 = CARTESIAN_POINT ( 'NONE',  ( 815.2698199232961542, -352.8164208402374129, -342.5225473063383106 ) ) ;
#36461 = DIRECTION ( 'NONE',  ( -0.000000000000000000, 1.000000000000000000, -0.000000000000000000 ) ) ;
#36462 = CARTESIAN_POINT ( 'NONE',  ( 784.0799538623451781, -395.8055962898682765, 364.6971507214555572 ) ) ;
#36463 = ORIENTED_EDGE ( 'NONE', *, *, #28665, .T. ) ;
#36464 = CARTESIAN_POINT ( 'NONE',  ( 797.8594530101008786, -421.5436935675101040, -322.1405469898980982 ) ) ;
#36465 = VECTOR ( 'NONE', #43339, 1000.000000000000000 ) ;
#36466 = CARTESIAN_POINT ( 'NONE',  ( 813.9316612368132837, -127.4419599262326983, -348.6739635108323228 ) ) ;
#36467 = DIRECTION ( 'NONE',  ( -1.000000000000000000, -0.000000000000000000, -0.000000000000000000 ) ) ;
#36468 = CARTESIAN_POINT ( 'NONE',  ( 758.0141637701419768, -231.0783235625960401, 367.2620300519063790 ) ) ;
#36469 = CARTESIAN_POINT ( 'NONE',  ( 801.9419747391806368, -66.45278447660216159, 351.9812246680014027 ) ) ;
#36470 = CARTESIAN_POINT ( 'NONE',  ( 790.8726784830453198, -226.7146871989596661, -362.5472867521010585 ) ) ;
#36471 = CARTESIAN_POINT ( 'NONE',  ( 756.3353852180819104, -245.9073299311469896, 331.1735550268788302 ) ) ;
#36472 = CARTESIAN_POINT ( 'NONE',  ( 813.9316612368132837, -55.44195992623293989, -348.6739635108323228 ) ) ;
#36473 = DIRECTION ( 'NONE',  ( -1.644774851296528363E-16, 1.000000000000000000, 0.000000000000000000 ) ) ;
#36474 = PRESENTATION_LAYER_ASSIGNMENT (  '', '', ( #28356 ) ) ;
#36475 = ORIENTED_EDGE ( 'NONE', *, *, #4371, .T. ) ;
#36476 = ORIENTED_EDGE ( 'NONE', *, *, #43051, .F. ) ;
#36477 = CARTESIAN_POINT ( 'NONE',  ( 746.4236121716829757, -351.8272453906068336, -328.8385539511384650 ) ) ;
#36478 = EDGE_CURVE ( 'NONE', #26915, #34024, #18191, .T. ) ;
#36479 = CARTESIAN_POINT ( 'NONE',  ( 815.2698199232962679, -304.8164208402376971, 342.5225473063383674 ) ) ;
#36480 = CARTESIAN_POINT ( 'NONE',  ( 744.9990715423526808, -18.35105083532395298, 341.2370466360926002 ) ) ;
#36481 = CARTESIAN_POINT ( 'NONE',  ( 801.5560724626406000, -192.5545181178801215, -326.7756240680316182 ) ) ;
#36482 = CARTESIAN_POINT ( 'NONE',  ( 762.3223304703356007, -199.5436935675108430, -322.3223304703362828 ) ) ;
#36483 = CARTESIAN_POINT ( 'NONE',  ( 768.0187753319979720, -392.6346026584193396, -318.0580252608186242 ) ) ;
#36484 = ORIENTED_EDGE ( 'NONE', *, *, #44388, .T. ) ;
#36485 = ORIENTED_EDGE ( 'NONE', *, *, #184, .T. ) ;
#36486 = CARTESIAN_POINT ( 'NONE',  ( 801.1904061080336987, -308.0891481129650629, 368.3070685750235498 ) ) ;
#36487 = VECTOR ( 'NONE', #25325, 1000.000000000000000 ) ;
#36488 = PLANE ( 'NONE',  #7868 ) ;
#36489 = CARTESIAN_POINT ( 'NONE',  ( 801.5560724626406000, -216.5545181178800931, 326.7756240680316182 ) ) ;
#36490 = DIRECTION ( 'NONE',  ( 1.644774851296528363E-16, -1.000000000000000000, -0.000000000000000000 ) ) ;
#36491 = AXIS2_PLACEMENT_3D ( 'NONE', #16526, #37074, #5212 ) ;
#36492 = CARTESIAN_POINT ( 'NONE',  ( 804.4086373105744769, -193.6454272087891582, 333.3843516231986541 ) ) ;
#36493 = CARTESIAN_POINT ( 'NONE',  ( 756.5762568750052424, -51.18005720387493085, 348.7366044899774238 ) ) ;
#36494 = ORIENTED_EDGE ( 'NONE', *, *, #26116, .T. ) ;
#36495 = CARTESIAN_POINT ( 'NONE',  ( 814.2805881961230625, -409.6454272087884760, -331.2368401574024119 ) ) ;
#36496 = CARTESIAN_POINT ( 'NONE',  ( 747.2067596250078623, -51.18005720387493085, -352.2312462859687230 ) ) ;
#36497 = CARTESIAN_POINT ( 'NONE',  ( 776.9566956441375396, -228.8965053807778816, 364.8461984189686405 ) ) ;
#36498 = CARTESIAN_POINT ( 'NONE',  ( 762.1405469898971887, -385.5436935675102745, -357.8594530101015607 ) ) ;
#36499 = CARTESIAN_POINT ( 'NONE',  ( 781.7834795799800531, -10.81642084023869543, -315.0636971347436202 ) ) ;
#36500 = CARTESIAN_POINT ( 'NONE',  ( 751.9810565676468741, -434.0891481129646081, 360.9747183278973921 ) ) ;
#36501 = DIRECTION ( 'NONE',  ( 0.000000000000000000, 0.3826834323650836200, 0.9238795325112892920 ) ) ;
#36502 = CARTESIAN_POINT ( 'NONE',  ( 800.9840315886518738, -244.9181544815162681, -354.1144889064786412 ) ) ;
#36503 = CARTESIAN_POINT ( 'NONE',  ( 745.7998596910086917, -173.3618753856927128, -332.5602148656461168 ) ) ;
#36504 = CLOSED_SHELL ( 'NONE', ( #39160, #5482, #24160, #19526, #16564, #38233, #5547, #5542, #14601, #15411, #20664, #31994, #21588, #38900, #28990, #24634, #29796, #45360, #1508, #6627, #4907, #105, #22445, #3109, #9067, #15961, #9149, #5720, #23807, #45578, #10783, #15618, #10901, #28070, #4610, #1831, #18431, #18765, #17403, #44942, #11095, #30957, #16541, #4782, #13693, #2382, #40701, #33390, #12597, #5963 ) ) ;
#36505 = CARTESIAN_POINT ( 'NONE',  ( 813.1304606946830518, -65.90732993114758642, 352.3570229623690580 ) ) ;
#36506 = EDGE_CURVE ( 'NONE', #15902, #16465, #39672, .T. ) ;
#36507 = CARTESIAN_POINT ( 'NONE',  ( 763.2262854647970016, -104.6346026584202207, 309.2812353651462445 ) ) ;
#36508 = DIRECTION ( 'NONE',  ( 1.892425610156518354E-16, 1.000000000000000000, -0.000000000000000000 ) ) ;
#36509 = AXIS2_PLACEMENT_3D ( 'NONE', #9920, #34158, #20761 ) ;
#36510 = FACE_OUTER_BOUND ( 'NONE', #33866, .T. ) ;
#36511 = CIRCLE ( 'NONE', #32093, 9.999999999999982236 ) ;
#36512 = CARTESIAN_POINT ( 'NONE',  ( 807.2620300519052989, -384.0090635724249637, 318.0141637701419768 ) ) ;
#36513 = CARTESIAN_POINT ( 'NONE',  ( -786.4999999999993179, 262.9227088301245203, 634.7515695135432452 ) ) ;
#36514 = CARTESIAN_POINT ( 'NONE',  ( 796.7737145352015204, -356.6346026584193964, 370.7187646348536987 ) ) ;
#36515 = CARTESIAN_POINT ( 'NONE',  ( 800.0135310231082713, -302.0891481129650629, -325.0180583372163028 ) ) ;
#36516 = CARTESIAN_POINT ( 'NONE',  ( 796.7845633553578182, 14.37622189194867417, 358.5707757039688204 ) ) ;
#36517 = AXIS2_PLACEMENT_3D ( 'NONE', #15157, #40329, #43989 ) ;
#36518 = CARTESIAN_POINT ( 'NONE',  ( 748.6759233522253680, -64.37269993606231822, -324.3348316497537098 ) ) ;
#36519 = CARTESIAN_POINT ( 'NONE',  ( 755.0488828828309806, -113.8055962898691149, -344.1219089521771934 ) ) ;
#36520 = CARTESIAN_POINT ( 'NONE',  ( 752.4576283171824116, -141.0783235625962959, 317.7880784355627952 ) ) ;
#36521 = CARTESIAN_POINT ( 'NONE',  ( 803.4237431249931660, -447.1800572038736732, 331.2633955100225194 ) ) ;
#36522 = AXIS2_PLACEMENT_3D ( 'NONE', #9600, #6363, #37772 ) ;
#36523 = CARTESIAN_POINT ( 'NONE',  ( 744.8212110874229666, -162.8965053807780521, 336.2046728542121627 ) ) ;
#36524 = CARTESIAN_POINT ( 'NONE',  ( 778.2165204200184689, -22.81642084023865280, -364.9363028652563230 ) ) ;
#36525 = CARTESIAN_POINT ( 'NONE',  ( 795.9930595647434757, -123.0783235625963385, -320.7433823573372820 ) ) ;
#36526 = CARTESIAN_POINT ( 'NONE',  ( 800.0135310231082713, -134.0891481129655745, -325.0180583372163028 ) ) ;
#36527 = CARTESIAN_POINT ( 'NONE',  ( 804.9363028652555840, -112.2709662947838325, 338.2165204200192079 ) ) ;
#36528 = VECTOR ( 'NONE', #9992, 1000.000000000000000 ) ;
#36529 = EDGE_CURVE ( 'NONE', #463, #45642, #43340, .T. ) ;
#36530 = VECTOR ( 'NONE', #22956, 1000.000000000000000 ) ;
#36531 = CARTESIAN_POINT ( 'NONE',  ( 769.1273215169530886, -430.7146871989590409, -317.4527132478988847 ) ) ;
#36533 = CARTESIAN_POINT ( 'NONE',  ( 791.9812246680005501, -260.6346026584197375, 361.9419747391813189 ) ) ;
#36532 = CARTESIAN_POINT ( 'NONE',  ( 803.6646147819161570, -257.9073299311469896, 348.8264449731210561 ) ) ;
#36534 = LINE ( 'NONE', #22425, #10179 ) ;
#36535 = VERTEX_POINT ( 'NONE', #14726 ) ;
#36536 = CARTESIAN_POINT ( 'NONE',  ( 805.1016975059191054, 17.10349461922139369, 343.0745993439771837 ) ) ;
#36537 = VERTEX_POINT ( 'NONE', #29025 ) ;
#36538 = ADVANCED_FACE ( 'NONE', ( #24867 ), #25780, .F. ) ;
#36539 = CARTESIAN_POINT ( 'NONE',  ( 758.8095938919644823, -176.0891481129654039, 311.6929314249762797 ) ) ;
#36540 = CARTESIAN_POINT ( 'NONE',  ( 760.7433823573367135, -300.0090635724252479, 355.9930595647440441 ) ) ;
#36541 = CARTESIAN_POINT ( 'NONE',  ( 793.2243759319678702, -386.5328690171409676, 318.4439275373583200 ) ) ;
#36542 = ORIENTED_EDGE ( 'NONE', *, *, #2975, .F. ) ;
#36543 = CARTESIAN_POINT ( 'NONE',  ( 786.5483106153019435, -79.64542720878957027, -364.1601925771022366 ) ) ;
#36544 = CARTESIAN_POINT ( 'NONE',  ( 781.2497674668890113, -204.3510508353233774, 375.3608509340180603 ) ) ;
#36545 = CARTESIAN_POINT ( 'NONE',  ( 764.8639956371174549, -272.0891481129651197, -319.7806653035542581 ) ) ;
#36546 = AXIS2_PLACEMENT_3D ( 'NONE', #5872, #32996, #27124 ) ;
#36547 = ORIENTED_EDGE ( 'NONE', *, *, #38237, .F. ) ;
#36548 = CARTESIAN_POINT ( 'NONE',  ( 803.4237431249931660, -399.1800572038738437, -331.2633955100225194 ) ) ;
#36549 = CARTESIAN_POINT ( 'NONE',  ( 755.0636971347428243, -52.27096629478401724, -341.7834795799807353 ) ) ;
#36550 = CIRCLE ( 'NONE', #42445, 7.999999999999785061 ) ;
#36551 = CARTESIAN_POINT ( 'NONE',  ( 803.2186876482843445, -271.9874144716868045, 350.0220218866286928 ) ) ;
#36552 = FACE_OUTER_BOUND ( 'NONE', #26433, .T. ) ;
#36553 = DIRECTION ( 'NONE',  ( -0.000000000000000000, 1.000000000000000000, -0.000000000000000000 ) ) ;
#36554 = CARTESIAN_POINT ( 'NONE',  ( 752.7379699480933368, -12.00906357242613609, -361.9858362298580232 ) ) ;
#36555 = DIRECTION ( 'NONE',  ( -1.000000000000000000, -0.000000000000000000, -0.000000000000000000 ) ) ;
#36556 = ORIENTED_EDGE ( 'NONE', *, *, #2120, .F. ) ;
#36557 = CARTESIAN_POINT ( 'NONE',  ( 811.3240766477731540, -292.3726999360616219, -355.6651683502462902 ) ) ;
#36558 = EDGE_CURVE ( 'NONE', #16670, #12174, #30117, .T. ) ;
#36559 = CARTESIAN_POINT ( 'NONE',  ( 804.1009440267234822, -167.4636090269711133, 314.0944755984392600 ) ) ;
#36560 = AXIS2_PLACEMENT_3D ( 'NONE', #24295, #38401, #6751 ) ;
#36562 = CARTESIAN_POINT ( 'NONE',  ( 802.1676090361156639, -302.6346026584196238, -327.8955696845344505 ) ) ;
#36561 = DIRECTION ( 'NONE',  ( -0.000000000000000000, -0.3826834323650836756, -0.9238795325112892920 ) ) ;
#36563 =( BOUNDED_CURVE ( )  B_SPLINE_CURVE ( 3, ( #3930, #471, #14102, #38828 ),
 .UNSPECIFIED., .F., .T. ) 
 B_SPLINE_CURVE_WITH_KNOTS ( ( 4, 4 ),
 ( 4.712388980384714543, 4.733441231200429478 ),
 .UNSPECIFIED. ) 
 CURVE ( )  GEOMETRIC_REPRESENTATION_ITEM ( )  RATIONAL_B_SPLINE_CURVE ( ( 1.000000000000000000, 0.9999630672356449868, 0.9999630672356449868, 1.000000000000000000 ) ) 
 REPRESENTATION_ITEM ( '' )  );
#36564 = EDGE_CURVE ( 'NONE', #41202, #20268, #44899, .T. ) ;
#36565 = CARTESIAN_POINT ( 'NONE',  ( 757.4527132478984868, -160.3726999360620482, -329.1273215169538844 ) ) ;
#36566 = AXIS2_PLACEMENT_3D ( 'NONE', #4515, #1040, #15145 ) ;
#36567 = CARTESIAN_POINT ( 'NONE',  ( 814.9108240113580450, -16.27096629478413092, 337.5031285880265273 ) ) ;
#36568 = CARTESIAN_POINT ( 'NONE',  ( 989.9999999999992042, 249.9999999999998863, 350.0000000000000000 ) ) ;
#36569 = CARTESIAN_POINT ( 'NONE',  ( 807.5423716828161105, -9.078323562596708030, -362.2119215644372048 ) ) ;
#36570 = CARTESIAN_POINT ( 'NONE',  ( 814.2001403089898304, -353.3618753856922012, -347.4397851343538264 ) ) ;
#36571 = DIRECTION ( 'NONE',  ( 0.000000000000000000, 0.000000000000000000, -1.000000000000000000 ) ) ;
#36572 = CARTESIAN_POINT ( 'NONE',  ( 795.1360043628807261, -44.08914811296584446, 360.2193346964456282 ) ) ;
#36573 = CARTESIAN_POINT ( 'NONE',  ( 755.8990559732751535, -299.4636090269707438, 365.9055244015606831 ) ) ;
#36574 = CARTESIAN_POINT ( 'NONE',  ( 807.5423716828161105, -249.0783235625959549, -362.2119215644372048 ) ) ;
#36575 = CARTESIAN_POINT ( 'NONE',  ( 810.7187646348534145, -258.4527844766016074, 356.7737145352016341 ) ) ;
#36576 = CARTESIAN_POINT ( 'NONE',  ( 788.7631598425961101, -433.4419599262316183, -305.7194118038759143 ) ) ;
#36577 = CARTESIAN_POINT ( 'NONE',  ( 779.9999999999992042, 126.4563064324884465, 339.9999999999999432 ) ) ;
#36578 = ORIENTED_EDGE ( 'NONE', *, *, #10459, .T. ) ;
#36579 = CARTESIAN_POINT ( 'NONE',  ( 781.8018195045266339, -358.2709662947829088, 365.1927285166406705 ) ) ;
#36580 = CARTESIAN_POINT ( 'NONE',  ( 755.3028492785439312, -87.28179084515316788, 335.9200461376539693 ) ) ;
#36581 = CARTESIAN_POINT ( 'NONE',  ( 804.1601925771018387, -31.44195992623299674, -346.5483106153029098 ) ) ;
#36582 = AXIS2_PLACEMENT_3D ( 'NONE', #10944, #76, #17648 ) ;
#36583 = DIRECTION ( 'NONE',  ( 0.000000000000000000, 0.000000000000000000, 1.000000000000000000 ) ) ;
#36584 = ADVANCED_FACE ( 'NONE', ( #42878 ), #8020, .F. ) ;
#36585 = DIRECTION ( 'NONE',  ( 1.644774851296528363E-16, -1.000000000000000000, 0.000000000000000000 ) ) ;
#36586 = CARTESIAN_POINT ( 'NONE',  ( 797.6776695296629214, -379.5436935675102745, 357.6776695296636603 ) ) ;
#36587 = EDGE_LOOP ( 'NONE', ( #15974, #37446 ) ) ;
#36588 = CIRCLE ( 'NONE', #10779, 8.024999999999948841 ) ;
#36589 = EDGE_CURVE ( 'NONE', #30631, #21713, #4359, .T. ) ;
#36590 = CARTESIAN_POINT ( 'NONE',  ( 789.9200121543843807, -337.9874144716865771, -317.0176451133914384 ) ) ;
#36591 = CARTESIAN_POINT ( 'NONE',  ( 771.2633955100217236, -143.9073299311473590, 363.4237431249939618 ) ) ;
#36592 = UNCERTAINTY_MEASURE_WITH_UNIT (LENGTH_MEASURE( 1.000000000000000082E-05 ), #43968, 'distance_accuracy_value', 'NONE');
#36593 = CARTESIAN_POINT ( 'NONE',  ( 788.7631598425961101, -337.4419599262319593, -305.7194118038759143 ) ) ;
#36594 = LINE ( 'NONE', #40725, #31518 ) ;
#36595 = CARTESIAN_POINT ( 'NONE',  ( 814.8230680027162407, -437.8055962898679923, 333.7305795820267917 ) ) ;
#36596 = ORIENTED_EDGE ( 'NONE', *, *, #6009, .T. ) ;
#36597 = CARTESIAN_POINT ( 'NONE',  ( 788.7366044899766848, -347.9073299311467053, 316.5762568750059813 ) ) ;
#36598 = AXIS2_PLACEMENT_3D ( 'NONE', #34120, #43832, #16595 ) ;
#36599 = CARTESIAN_POINT ( 'NONE',  ( 802.7791456095903868, -76.71468719896012090, -329.0155153010375102 ) ) ;
#36600 = ORIENTED_EDGE ( 'NONE', *, *, #32332, .F. ) ;
#36601 = CARTESIAN_POINT ( 'NONE',  ( 791.7608162188021197, 205.0000000000000568, 360.0000000000000000 ) ) ;
#36602 = VECTOR ( 'NONE', #41789, 1000.000000000000000 ) ;
#36603 = CARTESIAN_POINT ( 'NONE',  ( 787.4397851343537695, -165.7255117493291152, -374.2001403089903988 ) ) ;
#36604 = CARTESIAN_POINT ( 'NONE',  ( 767.7687537140311633, -95.90732993114751537, 372.7932403749916830 ) ) ;
#36605 = ORIENTED_EDGE ( 'NONE', *, *, #4428, .F. ) ;
#36606 = CARTESIAN_POINT ( 'NONE',  ( 795.1360043628808398, -188.0891481129653755, -360.2193346964456282 ) ) ;
#36607 = EDGE_LOOP ( 'NONE', ( #32223, #5577, #16252, #14228 ) ) ;
#36608 = CARTESIAN_POINT ( 'NONE',  ( 780.5236548040995785, -428.7363362996975980, -314.9735926884559944 ) ) ;
#36609 = CARTESIAN_POINT ( 'NONE',  ( 771.2633955100217236, 0.09267006885218045942, 363.4237431249939618 ) ) ;
#36610 = CARTESIAN_POINT ( 'NONE',  ( 800.9747183278959710, -228.9982390220561683, 311.9810565676471583 ) ) ;
#36611 = CARTESIAN_POINT ( 'NONE',  ( 776.9566956441375396, -156.8965053807780805, 364.8461984189686405 ) ) ;
#36613 = CARTESIAN_POINT ( 'NONE',  ( 571.1634899080285095, 259.9999999999999432, -191.9749999999982037 ) ) ;
#36612 = CARTESIAN_POINT ( 'NONE',  ( 799.9999999999993179, 212.6707680665973612, -236.5295014342203785 ) ) ;
#36614 = ORIENTED_EDGE ( 'NONE', *, *, #40526, .T. ) ;
#36615 = CARTESIAN_POINT ( 'NONE',  ( 769.9779781133707957, -427.0999726633338582, -316.7813123517150871 ) ) ;
#36616 = CARTESIAN_POINT ( 'NONE',  ( 759.9999999999992042, -512.9681489794448908, -339.9999999999999432 ) ) ;
#36617 = CARTESIAN_POINT ( 'NONE',  ( 762.1177392798416577, -210.5545181178800647, -309.8865473780659272 ) ) ;
#36618 = CARTESIAN_POINT ( 'NONE',  ( 768.9521613784389729, -81.82724539060772884, 373.2346286133773106 ) ) ;
#36619 = VECTOR ( 'NONE', #30072, 1000.000000000000000 ) ;
#36621 = CARTESIAN_POINT ( 'NONE',  ( 788.7366044899766848, -203.9073299311471885, -316.5762568750059813 ) ) ;
#36620 = DIRECTION ( 'NONE',  ( -1.000000000000000000, -8.326672684688676025E-16, 0.000000000000000000 ) ) ;
#36622 = CARTESIAN_POINT ( 'NONE',  ( 758.6633372737375112, -332.5328690171411381, -326.9102291470432533 ) ) ;
#36623 = CARTESIAN_POINT ( 'NONE',  ( 779.9999999999992042, 166.4563064324884465, -339.9999999999999432 ) ) ;
#36624 = CARTESIAN_POINT ( 'NONE',  ( 748.6759233522253680, -208.3726999360619061, -324.3348316497537098 ) ) ;
#36625 = LINE ( 'NONE', #22076, #8278 ) ;
#36626 = LINE ( 'NONE', #18402, #39325 ) ;
#36627 = CARTESIAN_POINT ( 'NONE',  ( 779.4763451958990572, -32.73633629969879877, -365.0264073115438919 ) ) ;
#36628 = AXIS2_PLACEMENT_3D ( 'NONE', #13728, #3565, #16732 ) ;
#36629 = CARTESIAN_POINT ( 'NONE',  ( 804.4086373105744769, -385.6454272087888171, 333.3843516231986541 ) ) ;
#36630 = CARTESIAN_POINT ( 'NONE',  ( 787.5162901302840055, -227.3618753856925423, -305.4481719005793252 ) ) ;
#36631 = CARTESIAN_POINT ( 'NONE',  ( 769.9779781133707957, -235.0999726633344835, 316.7813123517150871 ) ) ;
#36632 = LINE ( 'NONE', #33168, #34954 ) ;
#36633 = CARTESIAN_POINT ( 'NONE',  ( 794.9819416627830151, -12.99823902205686821, -319.9864689768909898 ) ) ;
#36634 = CARTESIAN_POINT ( 'NONE',  ( 809.0717654672305343, -172.9181544815165239, 360.1688906516309885 ) ) ;
#36635 = CARTESIAN_POINT ( 'NONE',  ( 771.2368401574024119, -133.4419599262326699, -374.2805881961240857 ) ) ;
#36636 = CARTESIAN_POINT ( 'NONE',  ( 796.7737145352015204, -164.6346026584200217, 370.7187646348536987 ) ) ;
#36637 = CARTESIAN_POINT ( 'NONE',  ( 767.7687537140311633, -383.9073299311466485, -372.7932403749916830 ) ) ;
#36638 = AXIS2_PLACEMENT_3D ( 'NONE', #44501, #23242, #29960 ) ;
#36639 = DIRECTION ( 'NONE',  ( 0.000000000000000000, 0.000000000000000000, 1.000000000000000000 ) ) ;
#36640 = CARTESIAN_POINT ( 'NONE',  ( 939.9999999999992042, 56.73212367640090292, 362.5753187112032947 ) ) ;
#36641 = CARTESIAN_POINT ( 'NONE',  ( 792.1044303154645831, -204.4527844766016926, 317.8323909638837677 ) ) ;
#36642 = CARTESIAN_POINT ( 'NONE',  ( 754.7162404726377645, -14.73633629969885384, 339.4709603349214717 ) ) ;
#36643 = CARTESIAN_POINT ( 'NONE',  ( 771.1735550268778070, -393.1800572038737300, -316.3353852180827630 ) ) ;
#36644 = CARTESIAN_POINT ( 'NONE',  ( 799.9636004259356241, 1.081845518482914104, -311.2241431872006956 ) ) ;
#36645 = DIRECTION ( 'NONE',  ( 1.000000000000000000, 0.000000000000000000, 0.000000000000000000 ) ) ;
#36646 = CARTESIAN_POINT ( 'NONE',  ( 744.8212110874229666, -42.89650538077842157, 336.2046728542121627 ) ) ;
#36647 = ORIENTED_EDGE ( 'NONE', *, *, #15570, .T. ) ;
#36648 = CARTESIAN_POINT ( 'NONE',  ( 775.9200461376533440, -215.8055962898687881, -315.3028492785443291 ) ) ;
#36649 = CARTESIAN_POINT ( 'NONE',  ( 802.1676090361156639, -38.63460265842041252, 327.8955696845344505 ) ) ;
#36650 = CARTESIAN_POINT ( 'NONE',  ( 771.2368401574024119, -229.4419599262323572, -374.2805881961240857 ) ) ;
#36651 = CARTESIAN_POINT ( 'NONE',  ( 810.1134526219336749, -344.5328690171410813, 357.8822607201570349 ) ) ;
#36652 = ORIENTED_EDGE ( 'NONE', *, *, #37131, .T. ) ;
#36653 = VECTOR ( 'NONE', #35877, 1000.000000000000000 ) ;
#36654 = CARTESIAN_POINT ( 'NONE',  ( 755.0636971347428243, -340.2709662947831362, 341.7834795799807353 ) ) ;
#36655 = AXIS2_PLACEMENT_3D ( 'NONE', #433, #14536, #13842 ) ;
#36656 = CARTESIAN_POINT ( 'NONE',  ( 815.2698199232961542, -64.81642084023852135, -342.5225473063383106 ) ) ;
#36657 = CARTESIAN_POINT ( 'NONE',  ( 800.0135310231082713, -86.08914811296573077, -325.0180583372163028 ) ) ;
#36658 = ORIENTED_EDGE ( 'NONE', *, *, #18785, .F. ) ;
#36659 = CARTESIAN_POINT ( 'NONE',  ( 804.6971507214547046, -3.281790845153435221, -344.0799538623459739 ) ) ;
#36660 = ORIENTED_EDGE ( 'NONE', *, *, #32638, .F. ) ;
#36661 = CARTESIAN_POINT ( 'NONE',  ( 761.4292242960306112, -329.4636090269706870, -323.2154366446414429 ) ) ;
#36663 = CARTESIAN_POINT ( 'NONE',  ( 796.1575198192839480, -366.0090635724250774, 359.4546378042384163 ) ) ;
#36662 = CARTESIAN_POINT ( 'NONE',  ( 800.0135310231082713, -62.08914811296580183, 325.0180583372163028 ) ) ;
#36664 = AXIS2_PLACEMENT_3D ( 'NONE', #17932, #32247, #43322 ) ;
#36667 = CARTESIAN_POINT ( 'NONE',  ( 759.8311093483677041, -310.1692326535048778, 310.9282345327691814 ) ) ;
#36666 = PLANE ( 'NONE',  #9251 ) ;
#36665 = CARTESIAN_POINT ( 'NONE',  ( 772.5602148656447525, -417.7255117493283478, 305.7998596910095443 ) ) ;
#36668 = CARTESIAN_POINT ( 'NONE',  ( 805.9055244015594326, -99.62377810805098477, 315.8990559732753240 ) ) ;
#36669 = CARTESIAN_POINT ( 'NONE',  ( 805.2837595273609850, -314.7363362996979959, -340.5290396650784714 ) ) ;
#36670 = CARTESIAN_POINT ( 'NONE',  ( 768.0187753319979720, -272.6346026584196807, -318.0580252608186242 ) ) ;
#36671 = CARTESIAN_POINT ( 'NONE',  ( 754.8072714833581358, -148.8164208402382656, -338.1981804954720587 ) ) ;
#36672 = CARTESIAN_POINT ( 'NONE',  ( 751.9810565676468741, -410.0891481129647218, 360.9747183278973921 ) ) ;
#36674 = CARTESIAN_POINT ( 'NONE',  ( 799.9999999999993179, 205.0000000000000568, -245.0000000000000284 ) ) ;
#36673 = CARTESIAN_POINT ( 'NONE',  ( 772.4999999999993179, -462.9681489794447202, 270.0000000000000568 ) ) ;
#36675 = CARTESIAN_POINT ( 'NONE',  ( 783.7953271457878373, -128.1908817542439465, -375.1787889125761239 ) ) ;
#36676 = DIRECTION ( 'NONE',  ( 0.000000000000000000, 0.000000000000000000, 1.000000000000000000 ) ) ;
#36677 = CARTESIAN_POINT ( 'NONE',  ( 799.9999999999993179, -365.3551492539851893, 28.13243251470704109 ) ) ;
#36678 = CARTESIAN_POINT ( 'NONE',  ( 773.4516893846965786, -307.6454272087888171, 315.8398074228977066 ) ) ;
#36679 = CARTESIAN_POINT ( 'NONE',  ( 785.3687786644884454, -179.3618753856927128, 315.3201227861279676 ) ) ;
#36680 = ORIENTED_EDGE ( 'NONE', *, *, #37114, .T. ) ;
#36681 = CARTESIAN_POINT ( 'NONE',  ( 811.0346526505617248, -134.6346026584201070, -323.0537975583478101 ) ) ;
#36682 = CARTESIAN_POINT ( 'NONE',  ( 939.9999999999992042, 74.99999999999984368, -360.0000000000000000 ) ) ;
#36683 = CARTESIAN_POINT ( 'NONE',  ( 745.1792804349281596, -86.19088175424408860, 343.7566961878542884 ) ) ;
#36684 = CARTESIAN_POINT ( 'NONE',  ( 763.2262854647970016, -272.6346026584196807, -309.2812353651462445 ) ) ;
#36685 = CARTESIAN_POINT ( 'NONE',  ( 745.4481719005789273, -435.7255117493282341, -347.5162901302853697 ) ) ;
#36686 = CARTESIAN_POINT ( 'NONE',  ( 755.5713283507202505, -125.3618753856928834, 334.6858677611754729 ) ) ;
#36687 = ORIENTED_EDGE ( 'NONE', *, *, #11683, .T. ) ;
#36688 = CARTESIAN_POINT ( 'NONE',  ( 754.0944755984390895, -327.6237781080502600, -364.1009440267246760 ) ) ;
#36689 = VECTOR ( 'NONE', #45640, 1000.000000000000000 ) ;
#36690 = CARTESIAN_POINT ( 'NONE',  ( 804.7487373415286811, -91.54369356751116982, -364.7487373415288516 ) ) ;
#36691 = CARTESIAN_POINT ( 'NONE',  ( 804.4086373105744769, -25.64542720878973014, 333.3843516231986541 ) ) ;
#36692 = CARTESIAN_POINT ( 'NONE',  ( 782.5225473063381969, -358.2709662947829088, -375.2698199232970637 ) ) ;
#36693 = CARTESIAN_POINT ( 'NONE',  ( -39.63011601220123481, -512.9681489794448908, -329.9999999999999432 ) ) ;
#36694 = CARTESIAN_POINT ( 'NONE',  ( 765.8855110935204493, -406.1692326535045368, 319.0159684113471599 ) ) ;
#36695 = ORIENTED_EDGE ( 'NONE', *, *, #30520, .T. ) ;
#36696 = EDGE_CURVE ( 'NONE', #22008, #12108, #21633, .T. ) ;
#36697 = CARTESIAN_POINT ( 'NONE',  ( 776.2433038121456548, -108.8965053807782084, -374.8207195650711014 ) ) ;
#36698 = CARTESIAN_POINT ( 'NONE',  ( -265.7583438952258916, 290.0000000000001137, -320.0000000000000568 ) ) ;
#36699 = CARTESIAN_POINT ( 'NONE',  ( 808.7758568127978833, -244.1692326535050768, 320.0363995740631822 ) ) ;
#36700 = CARTESIAN_POINT ( 'NONE',  ( 781.7834795799800531, -58.81642084023854267, 315.0636971347436202 ) ) ;
#36701 = VERTEX_POINT ( 'NONE', #32266 ) ;
#36702 = CARTESIAN_POINT ( 'NONE',  ( 796.7845633553578182, -249.6237781080505158, -358.5707757039688204 ) ) ;
#36703 = CARTESIAN_POINT ( 'NONE',  ( 788.8264449731200330, -237.1800572038742985, 363.6646147819171233 ) ) ;
#36704 = CARTESIAN_POINT ( 'NONE',  ( 800.9747183278959710, 11.00176097794305541, -311.9810565676471583 ) ) ;
#36705 = CARTESIAN_POINT ( 'NONE',  ( 788.7631598425961101, -73.44195992623286884, -305.7194118038759143 ) ) ;
#36706 = CARTESIAN_POINT ( 'NONE',  ( -598.8365100919716042, 260.0000000000001705, -208.0249999999899160 ) ) ;
#36707 = EDGE_LOOP ( 'NONE', ( #39637, #43203, #28103, #20412 ) ) ;
#36708 = ORIENTED_EDGE ( 'NONE', *, *, #29361, .F. ) ;
#36709 = CARTESIAN_POINT ( 'NONE',  ( 788.6739635108323228, -391.6454272087885897, -373.9316612368139090 ) ) ;
#36710 = CARTESIAN_POINT ( 'NONE',  ( 763.0537975583476964, -312.4527844766013800, 371.0346526505628617 ) ) ;
#36711 = CARTESIAN_POINT ( 'NONE',  ( 811.6461892240364477, -28.71468719896028077, 324.1737431748509835 ) ) ;
#36712 = CARTESIAN_POINT ( 'NONE',  ( 776.9254006560222479, -212.1908817542436623, -314.8983024940802125 ) ) ;
#36713 = CARTESIAN_POINT ( 'NONE',  ( 788.7366044899766848, -179.9073299311472454, -316.5762568750059813 ) ) ;
#36714 = CARTESIAN_POINT ( 'NONE',  ( 802.1676090361155502, -398.6346026584193396, -327.8955696845344505 ) ) ;
#36715 = ORIENTED_EDGE ( 'NONE', *, *, #30000, .T. ) ;
#36716 = CARTESIAN_POINT ( 'NONE',  ( 774.6858677611749044, -225.7255117493289163, 315.5713283507209894 ) ) ;
#36717 = CARTESIAN_POINT ( 'NONE',  ( 776.9566956441375396, 11.10349461922141145, -364.8461984189686405 ) ) ;
#36718 = EDGE_LOOP ( 'NONE', ( #18548, #38760, #22940, #35740 ) ) ;
#36719 = AXIS2_PLACEMENT_3D ( 'NONE', #31419, #12961, #20105 ) ;
#36720 = CARTESIAN_POINT ( 'NONE',  ( 787.4397851343537695, -309.7255117493287457, 374.2001403089903988 ) ) ;
#36721 = DIRECTION ( 'NONE',  ( 8.659560562354869996E-17, 0.7071067811865526798, -0.7071067811865423547 ) ) ;
#36722 = CARTESIAN_POINT ( 'NONE',  ( 779.4709603349208464, -360.3510508353228374, 314.7162404726379918 ) ) ;
#36723 = PLANE ( 'NONE',  #1238 ) ;
#36724 = CYLINDRICAL_SURFACE ( 'NONE', #20903, 2.749999999999863665 ) ;
#36725 = CARTESIAN_POINT ( 'NONE',  ( 754.7162404726377645, -206.7363362996982801, 339.4709603349214717 ) ) ;
#36726 = CARTESIAN_POINT ( 'NONE',  ( 800.0135310231082713, -62.08914811296580183, 325.0180583372163028 ) ) ;
#36727 = ORIENTED_EDGE ( 'NONE', *, *, #23804, .T. ) ;
#36728 = CARTESIAN_POINT ( 'NONE',  ( 809.0717654672305343, -412.9181544815157281, -360.1688906516309885 ) ) ;
#36729 = CARTESIAN_POINT ( 'NONE',  ( 808.3070685750232087, -18.99823902205684689, -361.1904061080339829 ) ) ;
#36730 = CARTESIAN_POINT ( 'NONE',  ( 802.7791456095903868, -220.7146871989596661, 329.0155153010375102 ) ) ;
#36731 = CARTESIAN_POINT ( 'NONE',  ( 756.5762568750052424, -411.1800572038738437, -348.7366044899774238 ) ) ;
#36732 = CARTESIAN_POINT ( 'NONE',  ( 781.8018195045267476, 1.729033705215812233, -365.1927285166407273 ) ) ;
#36733 = CARTESIAN_POINT ( 'NONE',  ( 751.6929314249748586, -414.9982390220555430, 318.8095938919659034 ) ) ;
#36734 = DIRECTION ( 'NONE',  ( 1.000000000000000000, 0.000000000000000000, 0.000000000000000000 ) ) ;
#36735 = CARTESIAN_POINT ( 'NONE',  ( 801.5560724626406000, -264.5545181178798657, -326.7756240680316182 ) ) ;
#36736 = CARTESIAN_POINT ( 'NONE',  ( 755.2512626584698410, -151.5436935675109851, -315.2512626584710915 ) ) ;
#36737 = CARTESIAN_POINT ( 'NONE',  ( 767.6429770376289525, -33.18005720387498769, 306.8695393053162093 ) ) ;
#36738 = CARTESIAN_POINT ( 'NONE',  ( 745.0891759886404770, -124.2709662947837899, 342.4968714119734159 ) ) ;
#36739 = CARTESIAN_POINT ( 'NONE',  ( 770.1068079863199500, 16.45630643248850333, -316.7980005127122922 ) ) ;
#36740 = EDGE_CURVE ( 'NONE', #5516, #12844, #11708, .T. ) ;
#36741 = CARTESIAN_POINT ( 'NONE',  ( 745.1792804349281596, -398.1908817542431507, 343.7566961878542884 ) ) ;
#36742 = CARTESIAN_POINT ( 'NONE',  ( 879.9999999999992042, 99.99999999999984368, -360.0000000000000000 ) ) ;
#36743 = CARTESIAN_POINT ( 'NONE',  ( 746.8695393053150156, -365.9073299311465917, 327.6429770376306010 ) ) ;
#36744 = EDGE_CURVE ( 'NONE', #19442, #26065, #42690, .T. ) ;
#36745 = CARTESIAN_POINT ( 'NONE',  ( 804.4286716492782716, -329.3618753856922581, -345.3141322388244703 ) ) ;
#36746 = CARTESIAN_POINT ( 'NONE',  ( 776.9566956441375396, 11.10349461922141145, 364.8461984189686405 ) ) ;
#36747 = CARTESIAN_POINT ( 'NONE',  ( 781.2370466360911223, -92.73633629969860692, -304.9990715423533629 ) ) ;
#36748 = CARTESIAN_POINT ( 'NONE',  ( 795.9930595647434757, -123.0783235625963385, -320.7433823573372820 ) ) ;
#36749 = CARTESIAN_POINT ( 'NONE',  ( 798.0661480581538854, -146.5328690171417350, 309.5768839229118043 ) ) ;
#36750 = CARTESIAN_POINT ( 'NONE',  ( 802.1676090361155502, -446.6346026584191122, 327.8955696845344505 ) ) ;
#36751 = AXIS2_PLACEMENT_3D ( 'NONE', #42951, #28407, #21703 ) ;
#36752 = CARTESIAN_POINT ( 'NONE',  ( 768.8385539511368734, -167.2601417444143976, 306.4236121716840557 ) ) ;
#36753 = CARTESIAN_POINT ( 'NONE',  ( 755.3201227861273992, -27.72551174932954510, -345.3687786644892981 ) ) ;
#36754 = CARTESIAN_POINT ( 'NONE',  ( 761.2382568024794409, -135.6237781080508853, -356.9571628226838129 ) ) ;
#36755 = CARTESIAN_POINT ( 'NONE',  ( 771.1735550268778070, -129.1800572038746111, -316.3353852180827630 ) ) ;
#36756 = CARTESIAN_POINT ( 'NONE',  ( 795.1360043628807261, -116.0891481129656029, 360.2193346964456282 ) ) ;
#36757 = CARTESIAN_POINT ( 'NONE',  ( 794.1144889064781864, -442.1692326535044231, -360.9840315886528401 ) ) ;
#36759 = CARTESIAN_POINT ( 'NONE',  ( 764.8639956371174549, -272.0891481129651197, 319.7806653035542581 ) ) ;
#36758 = CARTESIAN_POINT ( 'NONE',  ( 758.0580252608178853, -246.4527844766016074, 328.0187753319985404 ) ) ;
#36760 = LINE ( 'NONE', #40673, #33047 ) ;
#36761 = ORIENTED_EDGE ( 'NONE', *, *, #15671, .T. ) ;
#36762 = CARTESIAN_POINT ( 'NONE',  ( 754.9735926884551418, 5.648949164675971524, 340.5236548041000333 ) ) ;
#36763 = CARTESIAN_POINT ( 'NONE',  ( 793.5525998758768083, -271.0999726633344267, -372.6845335610516941 ) ) ;
#36764 = VERTEX_POINT ( 'NONE', #11245 ) ;
#36765 = DIRECTION ( 'NONE',  ( 0.000000000000000000, 0.000000000000000000, 1.000000000000000000 ) ) ;
#36766 = CARTESIAN_POINT ( 'NONE',  ( 767.7687537140311633, -191.9073299311471885, 372.7932403749916830 ) ) ;
#36767 = CARTESIAN_POINT ( 'NONE',  ( 766.0291762391763086, -298.9181544815161828, 360.7704444035551319 ) ) ;
#36768 = CARTESIAN_POINT ( 'NONE',  ( 789.9200121543843807, -385.9874144716864066, 317.0176451133914384 ) ) ;
#36769 = ADVANCED_FACE ( 'NONE', ( #15174 ), #25319, .F. ) ;
#36770 = ORIENTED_EDGE ( 'NONE', *, *, #24413, .T. ) ;
#36771 = CARTESIAN_POINT ( 'NONE',  ( 790.9844846989617508, -70.37269993606230400, -317.2208543904092721 ) ) ;
#36772 = CARTESIAN_POINT ( 'NONE',  ( 756.3353852180820240, -293.9073299311468759, -331.1735550268787733 ) ) ;
#36773 = VERTEX_POINT ( 'NONE', #4322 ) ;
#36774 = CARTESIAN_POINT ( 'NONE',  ( 759.7806653035534055, -390.9982390220557136, -324.8639956371180801 ) ) ;
#36775 = CARTESIAN_POINT ( 'NONE',  ( 768.0187753319979720, -56.63460265842036279, -318.0580252608186242 ) ) ;
#36776 = CARTESIAN_POINT ( 'NONE',  ( 794.1144889064781864, -274.1692326535049915, 360.9840315886528401 ) ) ;
#36777 = CARTESIAN_POINT ( 'NONE',  ( -949.5497976682736407, 240.0000000000002274, -209.9999999999999716 ) ) ;
#36778 = DIRECTION ( 'NONE',  ( -1.000000000000000000, -0.000000000000000000, -0.000000000000000000 ) ) ;
#36779 = CARTESIAN_POINT ( 'NONE',  ( 764.1737431748507561, -10.37269993606250473, -371.6461892240376415 ) ) ;
#36780 = DIRECTION ( 'NONE',  ( 1.000000000000000000, 0.000000000000000000, 0.000000000000000000 ) ) ;
#36781 = VERTEX_POINT ( 'NONE', #3642 ) ;
#36782 = CARTESIAN_POINT ( 'NONE',  ( 804.1009440267234822, -311.4636090269706870, -314.0944755984392600 ) ) ;
#36783 = CARTESIAN_POINT ( 'NONE',  ( 757.7880784355613741, -210.0090635724255321, 312.4576283171834916 ) ) ;
#36784 = CIRCLE ( 'NONE', #658, 7.999999999999785061 ) ;
#36786 = CARTESIAN_POINT ( 'NONE',  ( 759.7806653035534055, -294.9982390220560546, -324.8639956371180801 ) ) ;
#36785 = DIRECTION ( 'NONE',  ( 0.000000000000000000, 0.000000000000000000, 1.000000000000000000 ) ) ;
#36787 = CARTESIAN_POINT ( 'NONE',  ( 1238.921997096861332, 240.0000000000000853, -360.0000000000000000 ) ) ;
#36788 = CARTESIAN_POINT ( 'NONE',  ( 796.9571628226829034, -167.4636090269711133, -321.2382568024804641 ) ) ;
#36789 = EDGE_CURVE ( 'NONE', #29612, #37323, #36066, .T. ) ;
#36790 = PLANE ( 'NONE',  #18058 ) ;
#36791 = CARTESIAN_POINT ( 'NONE',  ( 814.8230680027162407, -5.805596289869448867, -333.7305795820267917 ) ) ;
#36792 = CARTESIAN_POINT ( 'NONE',  ( 811.0346526505617248, -350.6346026584193396, -323.0537975583478101 ) ) ;
#36793 = DIRECTION ( 'NONE',  ( 0.000000000000000000, -0.9238795325112891810, 0.3826834323650837866 ) ) ;
#36794 = CARTESIAN_POINT ( 'NONE',  ( 791.9812246680005501, -44.63460265842040542, 361.9419747391813189 ) ) ;
#36795 = CARTESIAN_POINT ( 'NONE',  ( 745.7194118038753459, -301.6454272087889308, 348.7631598425976449 ) ) ;
#36796 = CARTESIAN_POINT ( 'NONE',  ( 745.4481719005789273, -243.7255117493287742, 347.5162901302853129 ) ) ;
#36797 = CARTESIAN_POINT ( 'NONE',  ( 759.8311093483677041, -430.1692326535043094, -310.9282345327691814 ) ) ;
#36798 = EDGE_CURVE ( 'NONE', #5612, #56, #19092, .T. ) ;
#36799 = DIRECTION ( 'NONE',  ( 0.000000000000000000, 0.000000000000000000, -1.000000000000000000 ) ) ;
#36800 = VERTEX_POINT ( 'NONE', #6049 ) ;
#36801 = CARTESIAN_POINT ( 'NONE',  ( 778.2165204200184689, -358.8164208402375834, 364.9363028652563230 ) ) ;
#36802 = CARTESIAN_POINT ( 'NONE',  ( 779.4763451958990572, -104.7363362996985785, 365.0264073115438919 ) ) ;
#36803 = CARTESIAN_POINT ( 'NONE',  ( 779.4709603349208464, -0.3510508353240099355, -314.7162404726379918 ) ) ;
#36804 = LINE ( 'NONE', #44406, #38025 ) ;
#36805 = DIRECTION ( 'NONE',  ( 0.000000000000000000, 0.000000000000000000, 1.000000000000000000 ) ) ;
#36806 = CARTESIAN_POINT ( 'NONE',  ( 794.9819416627830151, -396.9982390220556567, 319.9864689768909898 ) ) ;
#36807 = ORIENTED_EDGE ( 'NONE', *, *, #2367, .T. ) ;
#36808 = CARTESIAN_POINT ( 'NONE',  ( 797.6776695296629214, -43.54369356751131903, -357.6776695296636603 ) ) ;
#36809 = CARTESIAN_POINT ( 'NONE',  ( 805.0264073115434940, -342.3510508353228943, -339.4763451958999099 ) ) ;
#36810 = CARTESIAN_POINT ( 'NONE',  ( 762.1405469898971887, -169.5436935675108430, 357.8594530101015607 ) ) ;
#36811 = CARTESIAN_POINT ( 'NONE',  ( 795.6651683502461765, -346.7146871989592682, -371.3240766477733814 ) ) ;
#36812 = DIRECTION ( 'NONE',  ( 1.000000000000000000, 0.000000000000000000, 0.000000000000000000 ) ) ;
#36813 = ADVANCED_FACE ( 'NONE', ( #8233, #19088 ), #20138, .F. ) ;
#36814 = VERTEX_POINT ( 'NONE', #45095 ) ;
#36815 = CARTESIAN_POINT ( 'NONE',  ( 754.8072714833581358, -364.8164208402374697, 338.1981804954720587 ) ) ;
#36816 = EDGE_CURVE ( 'NONE', #31071, #18371, #37926, .T. ) ;
#36817 = VERTEX_POINT ( 'NONE', #27083 ) ;
#36818 = SHAPE_REPRESENTATION_RELATIONSHIP ( 'NONE' , 'NONE' ,  #18903, #31528 ) ;
#36819 = CARTESIAN_POINT ( 'NONE',  ( 767.7687537140311633, -191.9073299311471885, -372.7932403749916830 ) ) ;
#36820 = CARTESIAN_POINT ( 'NONE',  ( 800.9747183278959710, -84.99823902205663728, 311.9810565676471583 ) ) ;
#36821 = EDGE_CURVE ( 'NONE', #19659, #28329, #15913, .T. ) ;
#36822 = ORIENTED_EDGE ( 'NONE', *, *, #29910, .F. ) ;
#36823 = CARTESIAN_POINT ( 'NONE',  ( 800.0135310231082713, -182.0891481129654323, -325.0180583372163028 ) ) ;
#36824 = ORIENTED_EDGE ( 'NONE', *, *, #21615, .F. ) ;
#36825 = CARTESIAN_POINT ( 'NONE',  ( 779.4763451958990572, -440.7363362996975980, -365.0264073115438919 ) ) ;
#36826 =( BOUNDED_SURFACE ( )  B_SPLINE_SURFACE ( 3, 2, ( 
 ( #25445, #32614, #39318, #3753, #28218, #35848, #3535, #39099, #39566, #32154, #7449, #24989, #28458, #24519, #24760, #21302, #42775, #10443, #17842, #32397, #7920, #42313, #747, #4224, #28697, #42557, #28921, #11136, #10677, #31909, #14379, #31687, #17619, #21524, #35601, #25207, #3977, #7673, #35155, #517, #18534, #21753, #42999, #11365, #36079, #4446, #956, #15061, #42092, #6988, #21073, #40003, #8808, #29597, #36968, #22419, #32841, #1414, #15517, #26118, #43675, #25892, #26351, #43455, #1192, #5322, #22655, #43898, #25682, #12491, #19649, #40455, #36524, #15299, #22876, #36298, #40232, #26568, #5109, #8589, #12046, #36753, #11603, #11822, #8353, #29817, #43232, #4883, #19416, #40666, #29384, #33507, #1855, #15728, #19197, #15963, #12276, #18986, #33077, #33284, #18753, #4655, #1629, #30045, #44126, #9020, #23090, #22205, #37190, #5556, #33742, #2092, #29148, #39794, #8142, #30737, #41824, #9492, #34656, #27041, #33958, #38131, #41582, #9937, #34871, #2310, #31183, #20099, #16651, #30489, #3015, #44594, #16181, #30262, #12711, #44831, #24009, #24246, #6700, #6482, #19881, #45278, #23555, #9263, #44354, #37657, #6006, #38355, #13191, #5795, #12954, #26790, #13637, #20778, #34174, #2546, #27272, #20561, #40895, #41363, #41139, #9711, #23774, #27484, #17102, #10169, #30964, #37888, #6239, #13415, #20328, #34422, #2790, #16882, #45058, #27720, #37435, #8475, #4554, #3476, #39906, #15193, #15416, #14323, #31857, #43355, #22546, #4775, #38820, #17324, #32971, #7174, #3235, #10391, #21011, #15923, #30007, #40636, #8776, #33704, #23057, #2054, #19384, #16148, #8989, #27002, #9223, #1815, #2275, #37617, #30231, #29781, #44322, #23297, #44555, #26757, #33470, #30451, #16374, #19611, #36937, #33924, #12914, #41098, #44094, #37157, #23516, #40423, #9453, #12459, #15696, #5970, #12677, #37399, #19842, #20060, #19168, #40862, #26318, #5753, #26538, #22844, #5515, #33252, #43856, #1598, #12239, #5291, #28808, #42887, #39444, #37318, #44473, #41471, #16533, #6369, #13074, #19767, #2672, #16767, #33626, #30848, #12609, #1977, #44944, #44249, #5676, #9378, #26685, #2207, #23444, #13300, #20451, #27376, #9824, #23893, #18428, #11937, #39908, #32508, #5014, #36193, #26004, #43128, #22315, #15196, #32974, #8038, #40576, #29281, #29939, #35973, #1317, #33398, #14957, #15419, #22549, #29043, #8714, #1744, #19105, #4557, #11496, #43359, #8249, #39691, #25576, #33192, #43785, #22104, #12166, #26249, #36875, #18647, #32737, #1082, #20460, #20224, #16306, #41480, #45173, #41256, #1984, #9612, #34311, #6379, #37785, #33860, #38023, #9833, #16542, #37325, #13308, #23902, #34548, #19776, #34076, #13533, #26693, #2907, #26919, #19536, #16998, #23673, #2681, #44952, #31074, #27608, #6133, #30166, #16777, #12838, #12615, #41024, #30857, #5441, #44721, #2213, #41715, #30625, #13084, #22992, #30389, #37551, #37085, #27385, #33632, #27168, #9384, #16082, #44256, #9147, #40789, #44481, #23216, #5685, #23451, #5909, #2439, #19999, #38251, #21146, #17216, #28765, #14455, #24142, #28064, #6596, #31755, #31544, #20674, #24829, #10288, #3607, #31303, #42158, #34995, #10510, #27850, #14689, #3371, #35674, #587, #7063, #39170, #34765, #38703, #124, #10071, #28533, #21594, #24586, #24363, #7520, #17462, #45647, #13772, #4050, #41947, #31979, #17694, #18148, #35228, #14214, #28283, #32227, #42383, #38466, #3127, #42628, #13996, #45410, #6819, #20897, #10752, #10990, #3821, #38949, #7299, #350, #21374, #35450, #17911, #25058, #1588, #19160, #5283, #15688, #12668, #19602, #9213, #5069, #8768, #8543, #29770, #22835, #19833, #2044, #1808, #12451, #23509, #36929, #16364, #33460, #43848, #33915, #23288, #37390, #22609, #26309, #15914, #29998, #26530, #8980, #44545, #23049, #37147, #16138, #2267, #45230, #10348, #38770, #21206, #24422, #34375, #45705, #23963, #23731, #30691, #38084, #20519, #7127, #31133, #20283, #2745, #13144, #14056, #35287, #34611, #6440, #2968, #35056, #27225, #27673, #16840, #41778, #30918, #42005, #6881, #10576, #45474, #17056, #24202, #27908, #13367, #3189, #13591, #45014, #10128, #3429, #31367, #3665, #34825, #9889, #38527, #38311, #20957, #6657, #27439, #20731, #17276, #13831, #17527, #31600, #28127, #42222, #24653, #41317, #9666, #6191, #14277, #1093, #8259, #14968, #25113, #21432, #11505, #24891, #14750, #15206, #39461, #28823, #648, #4124, #186, #418, #14522, #18439, #31816, #39227, #39701, #29294, #35508, #43370, #39917, #25804, #11048, #7580, #32293, #3883, #25346, #42903, #7819, #28599, #35983, #11270, #11734, #29053, #21657, #4566, #22325, #4348, #42450, #32517, #43139, #36426, #25590, #35745, #17752, #18657, #8049, #32046, #22113, #28348, #10818, #39005, #7356, #17976, #8489, #45126, #9332, #1326, #34497, #23622, #2622, #27337, #13484, #2857, #37731, #11948, #44900, #40970, #40126, #23401, #34250, #32987, #27115, #30333, #41661, #13025, #41206, #10016, #12780, #19952, #27556, #6083, #24085, #9562, #37504, #41430, #9781, #37269, #16722, #16255, #23161, #30806, #5629, #44426, #30564, #19723, #15430, #16483, #26015, #4789, #23848, #18892, #5863, #29507, #13259, #26862, #43580, #37962, #33811, #44664, #2164, #34027, #2383, #20401, #16949, #42799, #31491, #18096, #28719, #35181, #21542, #31255, #21095, #28236, #11159, #42581, #3996, #24537, #6771, #35624, #45594, #13942, #41892, #32177, #24316, #14401, #31706, #540, #3557, #38650, #17644, #14644, #7008, #38420, #6547, #10939, #28016, #73, #10237, #3771, #28480, #38199, #7252, #14165, #42331, #35399, #20847, #10698, #42110, #34945, #10461, #25012, #38898, #20626, #24780, #3313, #17861, #21323, #300, #31929, #17409, #39121, #7471, #34719, #3078, #45357, #13717, #27796, #43020, #1434, #18775, #40022, #21775, #8612, #15750, #22442, #32635, #28942, #19004, #32417, #22222, #22677, #1211, #36316, #8159, #11623, #7694, #7942, #22009, #25912, #39341, #978, #15535, #36774, #11384, #29616, #33096, #11841, #25701, #43694, #8373, #25467, #39586, #36100, #14866, #765, #15082, #4464, #36548, #32863, #4905, #18336, #18553, #1649, #29169, #43252, #12066, #15319, #39813, #4677, #5130, #29401, #26140, #43473, #40256, #19217, #33304, #29838, #43920, #25230, #35869, #4246, #12732, #12514, #30757, #30068, #30980, #26374, #8829, #26811, #37680, #20348, #2808, #6029, #15986, #27289, #5578, #5342, #12299, #19669, #2114, #34443, #40918, #1877, #44149, #40476, #41382, #16899, #16203, #33763, #30283, #16671, #22896, #9284, #26589, #40687, #9042, #23111, #37213, #33529, #44376, #23354, #27065, #19903, #41160, #19436, #37456, #36988, #5816, #33980, #34196, #2331, #16431, #30511, #37907, #44614, #44850, #12977, #9511, #2566, #20121, #13212, #23575, #9730, #23796, #6261, #45537, #6718, #24950, #10408, #31653, #38838, #39065, #15024, #11790, #40189, #22616, #25861, #18282 ),
 ( #12011, #1156, #32577, #25646, #29350, #14807, #4616, #39528, #42961, #21959, #4850, #15261, #8554, #36259, #11329, #8316, #43195, #33045, #25406, #7883, #11564, #39760, #18715, #43423, #36045, #15486, #43642, #26076, #36717, #32116, #481, #11102, #14586, #39282, #7638, #21714, #37139, #27215, #8973, #44538, #45003, #37603, #12897, #26983, #19825, #15905, #16130, #30217, #34124, #1796, #9204, #23723, #13358, #5497, #37836, #41309, #2491, #33908, #6185, #30682, #29990, #41082, #13137, #38074, #6433, #20275, #19591, #2737, #26741, #26523, #44077, #23278, #5738, #12443, #5956, #23041, #33688, #2037, #16831, #44307, #44781, #34367, #27432, #12661, #27663, #38517, #19535, #5684, #23215, #13083, #27167, #34310, #41255, #19775, #12837, #9611, #23672, #2680, #16776, #30856, #13307, #40361, #22780, #5225, #19315, #38250, #7061, #27848, #35227, #20672, #31073, #45408, #13770, #24361, #41945, #24141, #24584, #41714, #27607, #3606, #20895, #42157, #23901, #10750, #17909, #38701, #34763, #10070, #21144, #34547, #6817, #24827, #3369, #34993, #10287, #17460, #9832, #6594, #3125, #10508, #41479, #17214, #17692, #38947, #31301, #31753, #122, #13994, #31543, #14212, #28281, #45645, #42381, #7297, #16997, #2906, #21372, #35448, #3819, #31977, #27384, #20459, #38022, #6378, #32225, #11207, #36362, #36143, #18378, #28988, #40060, #7744, #32917, #25279, #585, #4723, #39857, #8198, #33137, #14687, #29442, #32458, #14907, #28763, #1262, #42843, #14453, #28531, #25518, #36599, #39391, #8420, #806, #10988, #11882, #32682, #11667, #18826, #22490, #25953, #15132, #21592, #22265, #4287, #4048, #43069, #43300, #42626, #4505, #21821, #4954, #22053, #18597, #25056, #35915, #11434, #39168, #29223, #7518, #25744, #39631, #35672, #7986, #12773, #38079, #31128, #42093, #35602, #38630, #55, #14380, #35156, #45574, #28459, #27998, #25446, #11137, #20827, #42558, #10444, #10921, #14625, #24520, #42776, #6989, #39319, #17620, #7674, #31688, #35849, #14148, #6754, #4225, #32398, #43000, #18318, #748, #28922, #22420, #29598, #30046, #43899, #5323, #25893, #8143, #36969, #32842, #1193, #43233, #19417, #25683, #15729, #33078, #33508, #36525, #40004, #4884, #1856, #8354, #39795, #7921, #12277, #15300, #22877, #15964, #44127, #29385, #43456, #18987, #11604, #1415, #15518, #43676, #22206, #12047, #26119, #12492, #36754, #11823, #26352, #39567, #40233, #18535, #8590, #5110, #21992, #22656, #4656, #8809, #40456, #19198, #36299, #29818, #36080, #4447, #18754, #33285, #1630, #32615, #957, #15062, #29149, #37436, #6240, #27042, #34423, #19882, #30263, #44595, #12955, #23556, #41140, #23332, #23775, #40896, #44355, #2791, #20100, #41364, #23091, #9938, #17103, #37889, #33959, #12712, #20329, #33743, #37658, #24010, #2547, #6007, #9493, #34175, #9021, #9264, #5796, #27273, #40667, #2311, #16883, #38132, #26791, #30965, #45059, #13192, #16652, #13416, #9712, #16410, #30490, #30738, #16182, #2093, #44832, #27485, #41583, #6483, #20562, #19650, #34657, #3016, #31184, #45279, #26569, #37191, #5557, #28171, #39265, #6929, #32097, #24468, #31413, #35549, #39048, #7397, #32339, #45519, #28644, #17567, #14097, #13873, #464, #27949, #13638, #27721, #10170, #42264, #21471, #21697, #4171, #3925, #17325, #42722, #21012, #6701, #41825, #35100, #3477, #35793, #10624, #3236, #42045, #24247, #11085, #18265, #31639, #7, #24701, #18020, #38356, #38821, #10392, #7175, #38574, #24933, #14568, #7621, #28400, #21248, #35328, #10867, #3706, #31858, #17792, #20779, #229, #14324, #34872, #42499, #25155, #8302, #7866, #32788, #25633, #1139, #18484, #5275, #39744, #26299, #36921, #43409, #29760, #25390, #29337, #36470, #19368, #5060, #12221, #15248, #15009, #43837, #8093, #22155, #4393, #8760, #32561, #22599, #22366, #22827, #25846, #4832, #18935, #695, #33030, #905, #14791, #19152, #36244, #28864, #42945, #11313, #4603, #18698, #1368, #29096, #15472, #29550, #43625, #43182, #11993, #26059, #39510, #40170, #8534, #33238, #21944, #36702, #36029, #1579, #15678, #11551, #44746, #40812, #44973, #2702, #23472, #44277, #20243, #30876, #27404, #26713, #41045, #6401, #33655, #9852, #2232, #26495, #41501, #2461, #41277, #6155, #23922, #20483, #16565, #37107, #23694, #16327, #19560, #30409, #13104, #8944, #20018, #44504, #34570, #37572, #9630, #2929, #12863, #26946, #29962, #37806, #44046, #34334, #5464, #2006, #16103, #30187, #12634, #27872, #6620, #35248, #3148, #10311, #42181, #31325, #45193, #28085, #24166, #35698, #35469, #31094, #35015, #34785, #10531, #20694, #28305, #38969, #11009, #31776, #17486, #24607, #14236, #45432, #3626, #24383, #13795, #6839, #3843, #146, #25076, #21167, #41969, #10774, #31565, #24851, #38487, #17239, #45665, #14017, #38724, #7086, #20919, #7319, #17934, #32003, #374, #14476, #28556, #13555, #39190, #7540, #21616, #17017, #27628, #41737, #38273, #10090, #1495, #25765, #15156, #32704, #36163, #32249, #32478, #828, #4745, #18173, #11459, #25974, #15593, #21845, #8442, #43536, #36383, #4525, #40082, #18849, #4306, #18398, #7767, #39415, #25303, #25542, #35938, #32939, #11692, #1285, #42863, #14927, #26213, #29010, #43093, #22512, #39877, #8007, #18617, #29675, #39655, #36622, #22073, #1050, #4977, #29463, #11903, #22745, #29247, #19070, #43324, #8218, #22287, #33158, #15384, #4074, #608, #14709, #43753, #12131, #40328, #8681, #28785, #11230, #6098, #30131, #29903, #36839, #44219, #26654, #13273, #37286, #26441, #40540, #19277, #20188, #44915, #40750, #12577, #9109, #41221, #5190, #33827, #9578, #30582, #23419, #23178, #27132, #5879, #37051, #5403, #8890, #22955, #12365, #5646, #19499, #19969, #44443, #34044, #43988, #1947, #27351, #33596, #16049, #13042, #12799, #19740, #2180, #16738, #16272, #23638, #30351, #26881, #37748, #16502, #44684, #9796, #40989, #34268, #9349, #37520, #2401, #2641, #30821, #33364, #1709, #15813, #41445, #3572, #31943, #14418, #17659, #27573, #38914, #17182, #16963, #23864, #31270, #13734, #314, #24330, #13497, #41677, #6336, #7267, #28497, #27811, #45372, #41908, #28248, #37981, #20861, #10034, #34960, #24101, #35195, #87, #3785, #38666, #10252, #17427, #21112, #6562, #42125, #38434, #38214, #6785, #42347, #24551, #42595, #28031, #34733, #31720, #3332, #14180, #31505, #20639, #45610, #13957, #10476, #7023, #3093, #10714, #24796, #21337, #35415, #17877, #20418, #34513, #2872, #31040, #45139, #19748, #15453, #34276, #33010, #23426, #9804, #34051, #37527, #5886, #44453, #39937, #40760, #9118, #13052, #25825, #2188, #44922, #37991, #30139, #19975, #26663, #13280, #27357, #41452, #16280, #2409, #34521, #44227, #6344, #30359, #22346, #20428, #30592, #9586, #2879, #16971, #31047, #44692, #1350, #11758, #12809, #12584, #26890, #23646, #36449, #16510, #27140, #37757, #7031, #21117, #4017, #6791, #13964, #39140 ),
 ( #20868, #41686, #14185, #45379, #38672, #6568, #31513, #24336, #45616, #17189, #18118, #38440, #25030, #35645, #42131, #28502, #24109, #28038, #35201, #45146, #3792, #10961, #10482, #13741, #42600, #34966, #3340, #3098, #7490, #31276, #21343, #3577, #21562, #24556, #17663, #31726, #13507, #93, #27818, #27580, #17882, #17433, #10040, #38221, #20646, #28253, #42352, #10721, #41915, #24801, #38920, #7272, #10259, #35419, #31949, #34738, #319, #14423, #4923, #36791, #1229, #25249, #15335, #25929, #15550, #36569, #43040, #1449, #19021, #18572, #14661, #11402, #25490, #33112, #42818, #39602, #29630, #43709, #32434, #26161, #40276, #5148, #32655, #32196, #21794, #7958, #22026, #36115, #4480, #997, #15100, #43269, #25718, #39830, #22238, #36335, #36455, #34413, #34862, #13864, #20551, #3005, #24458, #3467, #17093, #42036, #31172, #10382, #38565, #13868, #17318, #31408, #10619, #9706, #6923, #41577, #38126, #37882, #10386, #23769, #37652, #6000, #34168, #6477, #45515, #1, #28166, #27943, #41355, #21003, #30959, #30732, #20093, #45053, #27479, #14092, #20554, #27267, #6232, #2541, #35095, #42259, #9931, #13407, #24004, #42040, #16645, #34650, #20322, #3009, #34417, #3228, #24461, #17562, #6694, #17097, #31176, #34866, #2784, #10164, #45272, #16876, #13631, #38569, #38349, #44826, #41819, #27714, #3471, #24240, #31634, #20773, #13185, #42717, #11081, #21693, #25150, #21467, #21939, #39043, #42494, #900, #18261, #39505, #21243, #8088, #15244, #36024, #32089, #28394, #18477, #31853, #35788, #22150, #688, #4165, #7617, #35322, #36238, #29333, #4387, #459, #10861, #32556, #225, #32335, #4599, #14787, #28860, #42941, #39261, #7169, #7392, #35545, #25386, #38813, #14564, #15002, #18693, #24929, #29091, #43176, #11309, #7861, #11545, #25628, #3921, #18016, #28638, #14318, #39738, #32782, #1133, #43405, #24696, #3701, #17788, #22594, #33903, #15467, #8530, #33681, #33447, #15674, #26294, #37375, #5055, #30210, #36697, #29545, #2031, #37132, #5491, #30433, #43621, #26736, #29754, #12215, #11988, #44301, #26054, #11771, #25841, #8296, #40406, #19586, #19820, #2256, #16125, #40165, #40838, #19147, #4828, #39953, #33233, #1574, #16353, #8755, #1363, #43831, #22361, #9198, #36466, #22821, #36915, #5269, #12656, #18931, #19362, #1791, #15898, #29985, #23037, #23272, #5733, #26517, #44071, #12437, #8968, #40617, #33026, #6180, #13132, #34361, #3173, #45216, #6864, #2954, #9655, #24191, #44998, #6644, #37830, #2485, #16825, #30904, #41525, #13353, #41304, #41764, #27210, #16594, #20718, #38069, #13578, #10115, #27896, #27657, #23718, #13818, #17263, #6427, #20270, #34812, #45457, #31352, #2732, #9877, #20944, #30676, #24408, #27428, #41076, #41992, #17042, #38298, #10335, #38512, #35041, #31120, #5951, #3416, #23950, #34119, #20508, #17510, #26976, #34596, #44532, #12892, #9432, #23497, #37598, #20041, #44774, #25571, #32277, #22099, #21642, #3869, #21877, #35967, #17739, #28810, #42433, #21194, #4106, #31802, #24877, #11033, #172, #14044, #42671, #38756, #4550, #4334, #45691, #17961, #28114, #7566, #7342, #42208, #634, #14263, #25099, #7113, #32030, #10802, #403, #3651, #36189, #38992, #11491, #31588, #28584, #14952, #10558, #14506, #35728, #24635, #18423, #43122, #39214, #28331, #29036, #21419, #35495, #35273, #39684, #18201, #7802, #14736, #8032, #42889, #11256, #25331, #39446, #32503, #852, #32730, #22987, #11932, #1979, #40784, #26688, #25999, #40109, #19099, #36411, #26245, #1524, #40356, #1313, #8708, #33188, #16076, #15843, #8472, #37081, #9141, #36869, #43352, #5220, #22543, #5436, #18642, #15622, #4772, #29705, #22312, #29935, #40571, #44251, #33394, #5008, #12161, #44018, #15413, #19309, #36650, #32968, #43781, #19529, #1740, #23209, #22775, #29491, #12391, #26470, #8918, #33628, #18877, #30160, #12611, #37320, #1077, #43563, #15189, #29275, #11718, #25790, #39904, #8244, #2209, #34758, #41937, #2901, #13076, #9380, #45168, #12833, #2674, #3120, #27378, #16769, #34302, #37779, #33855, #34072, #2433, #6371, #19769, #27161, #27602, #17209, #23446, #10065, #13528, #38016, #6127, #41709, #20453, #5905, #19994, #37547, #41020, #26912, #41249, #16535, #34541, #13302, #16992, #44475, #30618, #27843, #44715, #9605, #24133, #41474, #23666, #20218, #31296, #30850, #38244, #44946, #9826, #6589, #31068, #20667, #24356, #23896, #45402, #13766, #10282, #5678, #16300, #30384, #11426, #6812, #34988, #7292, #18140, #801, #28983, #32220, #42152, #7738, #31746, #31538, #38460, #117, #28275, #14901, #38942, #28059, #10503, #20890, #21816, #43064, #42376, #14207, #7055, #10744, #42838, #39163, #3363, #42621, #3600, #580, #21367, #14681, #24822, #24579, #35443, #3812, #17904, #31972, #35222, #35667, #21139, #38696, #28758, #343, #7513, #17455, #35909, #45639, #4042, #14446, #17687, #11202, #13987, #28526, #4282, #10982, #25051, #21585, #25274, #39384, #18373, #32453, #26185, #39626, #32912, #1684, #22931, #43295, #29877, #19251, #12106, #11877, #15788, #40299, #25738, #39852, #29215, #15126, #1023, #1255, #11662, #8653, #33132, #22717, #18592, #36357, #1919, #8193, #22260, #43962, #1469, #29436, #40055, #5379, #18820, #12339, #4716, #15358, #26413, #5167, #33339, #44190, #43510, #40514, #25948, #8415, #22483, #8865, #36593, #25512, #7980, #22047, #4950, #37025, #33568, #16025, #19473, #19041, #30105, #15568, #32676, #36138, #29651, #43728, #4500, #36811, #2151, #16243, #40724, #41647, #20614, #16469, #5852, #30552, #16938, #12552, #9549, #30322, #23612, #44414, #23835, #34486, #38189, #27326, #44653, #6070, #9769, #40958, #30795, #19940, #13473, #45116, #9321, #37719, #34709, #12768, #6534, #13014, #9081, #10003, #44888, #37950, #2845, #3067, #24072, #13248, #19713, #6305, #2372, #26849, #27104, #41419, #23147, #34235, #37492, #17158, #20159, #2610, #31244, #34016, #41195, #26626, #20389, #37256, #16710, #31018, #27543, #5617, #23391, #33799, #10450, #34934, #17849, #31478, #38637, #24767, #13930, #27782, #10684, #6761, #18324, #3983, #13703, #17629, #41881, #21310, #21081, #10225, #14387, #45582, #38883, #20835, #31694, #24527, #62, #17394, #4232, #6996, #25214, #35855, #42319, #28703, #24303, #28225, #35386, #45340, #18080, #11144, #14154, #28005, #42782, #35165, #3543, #3300, #39326, #42100, #21530, #7238, #7681, #3759, #31916, #287, #21761, #28466, #42567, #38410, #32160, #10928, #24996, #39107, #7457, #35610, #525, #14631, #5062, #40624, #15907, #8975, #15682, #23043, #1799, #30439, #30219, #26302, #5740, #9438, #5500, #11995, #19594, #44309, #16359, #2039, #43839, #2262, #19827, #26525, #1582, #23282, #37142, #29762, #33691, #29993, #44540, #12663, #40412, #33910, #23503, #16132, #26061, #26743, #40845, #12900, #9207, #12223, #26986, #41086, #37383, #8762, #37605, #5958, #32404, #22829, #44079, #1370 ),
 ( #36923, #12445, #15474, #29553, #43628, #40172, #5277, #8536, #22602, #19154, #36704, #19371, #33240, #33455, #6187, #13360, #45223, #34369, #2493, #31126, #27217, #38762, #24416, #34126, #38076, #16601, #41772, #41532, #30684, #34818, #20277, #13585, #41311, #6435, #45005, #20514, #37838, #24644, #27434, #45697, #10567, #17047, #3423, #44785, #2961, #10122, #20047, #38520, #31594, #34604, #2739, #17519, #9884, #23956, #23725, #14050, #16834, #41998, #27666, #28120, #24197, #38304, #6652, #42216, #20726, #30912, #13140, #6871, #3180, #9661, #17270, #31359, #45465, #13825, #27902, #10341, #20952, #35049, #22106, #410, #177, #7120, #14514, #42676, #29284, #7572, #42440, #10810, #35279, #36195, #15198, #11039, #28591, #25105, #11498, #21199, #4115, #24884, #18209, #38998, #18430, #29045, #32739, #21887, #39220, #639, #4340, #35501, #25337, #21649, #21425, #35736, #25579, #7808, #43361, #11261, #17968, #32510, #32284, #14959, #14741, #7348, #28815, #42895, #39453, #35976, #3875, #859, #32040, #43131, #39694, #8041, #4559, #3657, #18649, #11727, #1085, #25796, #17745, #31809, #14271, #28340, #37327, #15851, #5227, #22782, #26251, #22317, #22551, #36656, #40578, #8251, #1531, #16084, #5688, #11939, #44259, #33634, #26476, #40364, #30168, #8924, #40116, #8481, #43571, #29499, #15421, #15627, #26006, #22994, #1746, #37088, #32977, #5016, #16309, #19107, #33194, #12617, #29941, #43787, #8716, #19778, #29710, #26695, #12169, #36877, #40791, #19539, #1987, #12840, #19318, #9150, #33401, #44025, #12397, #23220, #5444, #39910, #36418, #4781, #33862, #2215, #30391, #44483, #18883, #1319, #6821, #17464, #23905, #10290, #5911, #9835, #17000, #31547, #31305, #38469, #13310, #41258, #24366, #20226, #34314, #30628, #20899, #13087, #3129, #20462, #34997, #38026, #27387, #6381, #3374, #41482, #27170, #41027, #45413, #2683, #45649, #26923, #9387, #16780, #30860, #34551, #44724, #2910, #31076, #45175, #9614, #13535, #27610, #23453, #24144, #44954, #13774, #37553, #41719, #20001, #10073, #38253, #34078, #6599, #37787, #41949, #27852, #20677, #23675, #17218, #2441, #16544, #6135, #34767, #36145, #17696, #39634, #17913, #10513, #43071, #32229, #11211, #35918, #7989, #11436, #589, #21148, #7746, #3823, #3609, #31982, #42846, #42161, #35676, #38951, #4507, #21596, #4053, #18599, #21376, #28535, #22055, #14691, #32685, #18152, #353, #4289, #18380, #126, #25282, #24831, #31757, #28767, #14217, #7301, #39173, #28286, #24588, #25060, #35230, #13998, #32460, #28066, #14458, #38705, #39393, #35452, #7066, #21825, #42385, #7522, #10755, #42630, #10992, #808, #14909, #28991, #25521, #36603, #5385, #1689, #9087, #5172, #11885, #26421, #1476, #8872, #40063, #4726, #19049, #33140, #43734, #15576, #43519, #43970, #15365, #18829, #22936, #40308, #15793, #43303, #30111, #37263, #12345, #8423, #32921, #40521, #8201, #12112, #44200, #22723, #26192, #29657, #8661, #29227, #29446, #25956, #29883, #15135, #22493, #37032, #12558, #1265, #19478, #33575, #33346, #36819, #1927, #16030, #4957, #19258, #26634, #36365, #22268, #40730, #23154, #5624, #19718, #1031, #39860, #11671, #25748, #37498, #30557, #10010, #9774, #37725, #2617, #13711, #27110, #6540, #44659, #5858, #24080, #13479, #27550, #6766, #19946, #3072, #6077, #34242, #34022, #20620, #2377, #33805, #2158, #30327, #16717, #41654, #41887, #24310, #38194, #16478, #17163, #41200, #26854, #16250, #9557, #23617, #10230, #30801, #23396, #13020, #44421, #31250, #38415, #20165, #44894, #13254, #34714, #12775, #27332, #41425, #23843, #37955, #45121, #45349, #27789, #2851, #6314, #20396, #31023, #34491, #16944, #40965, #9327, #42105, #28473, #35392, #42574, #45587, #35175, #7687, #10455, #21090, #35617, #17855, #28231, #24775, #11151, #17636, #18086, #3551, #24532, #21535, #39113, #7462, #35861, #38645, #14636, #42326, #10690, #7002, #32169, #31700, #20841, #3306, #17402, #38891, #3989, #21766, #34940, #532, #67, #25220, #7245, #14160, #31486, #21317, #3765, #13935, #31921, #293, #14392, #10933, #28010, #25002, #28709, #42789, #39332, #20766, #16398, #13401, #34162, #27473, #20087, #27708, #38343, #42032, #31168, #2778, #9923, #13624, #44820, #34644, #23763, #30726, #6224, #34857, #17089, #24454, #20547, #27259, #41812, #16870, #24234, #9699, #2533, #34409, #30952, #41571, #45046, #13178, #10158, #41349, #16638, #6688, #23996, #45265, #12942, #45507, #6915, #3221, #37876, #20316, #17311, #23542, #38118, #13860, #6471, #3001, #31402, #27936, #44581, #10378, #38561, #20995, #30478, #35088, #27028, #41127, #9479, #37645, #5994, #35780, #35539, #39496, #18253, #3694, #17781, #7162, #38806, #24687, #10853, #14997, #35316, #25379, #42711, #29084, #451, #3915, #32081, #43171, #18009, #31846, #17556, #7853, #42486, #32548, #25621, #11539, #24922, #39036, #14555, #21236, #11075, #28633, #25143, #218, #39256, #7610, #894, #681, #7385, #21931, #39732, #21687, #28160, #4158, #14781, #8081, #32327, #14312, #18469, #36016, #28853, #28384, #4379, #22143, #3463, #21461, #42934, #31628, #11301, #11299, #14085, #42253, #10611, #8751, #33441, #12432, #30206, #19581, #22817, #43400, #29980, #26047, #25834, #8523, #19355, #18688, #12209, #15460, #26731, #43825, #26288, #40834, #43613, #5051, #44296, #36909, #9192, #40401, #22588, #26511, #40612, #22355, #1784, #1357, #39946, #5263, #36460, #29538, #15667, #4822, #32777, #1569, #11766, #36232, #8963, #4593, #36692, #1124, #15894, #11979, #15237, #44067, #18924, #29747, #8291, #19142, #40158, #33229, #33019, #29326, #23032, #16120, #37127, #5484, #33676, #2026, #12651, #13349, #13813, #27651, #34806, #9649, #37592, #20713, #16589, #30671, #26970, #9425, #44768, #2725, #5946, #5729, #34356, #30427, #41988, #41760, #37367, #41299, #19815, #44993, #13127, #33898, #38064, #23492, #16821, #44527, #23714, #2481, #37825, #41067, #27891, #27205, #3168, #23267, #20265, #6640, #2252, #6176, #27424, #16347, #10110, #17259, #30899, #20037, #31346, #41521, #9873, #34114, #45453, #23944, #45211, #6421, #12885, #20503, #34592, #2949, #17037, #31115, #13574, #24187, #38293, #3647, #39439, #32496, #18417, #17734, #31797, #10798, #28107, #17955, #38988, #32026, #38751, #397, #24872, #7794, #7561, #167, #28804, #846, #28579, #35036, #42667, #21636, #21871, #25095, #21189, #25324, #42882, #3865, #24630, #629, #11250, #35959, #7109, #21414, #14946, #14039, #4327, #14258, #6858, #29029, #11029, #35722, #32271, #10330, #24404, #39209, #17506, #4100, #28326, #45686, #42427, #18195, #38507, #14501, #35269, #20940, #14731, #3412, #31584, #7338, #35490, #42204, #10552, #33621, #33181, #15405, #33386, #1731, #29269, #40350, #8237, #32723, #15613, #26463, #29698, #8702, #19301, #37075, #40564, #43773, #4543, #36862, #32961, #1071, #29485, #26238, #25564, #19093, #22306, #1972 ),
 ( #16070, #15836, #11485, #43556, #39677, #1518, #18870, #8025, #12155, #43345, #36644, #18637, #11922, #36403, #25993, #15180, #43116, #4766, #22979, #22093, #40101, #8912, #36183, #8465, #22768, #11712, #29928, #5427, #22535, #25783, #19522, #1307, #5000, #39895, #5213, #44012, #12385, #24290, #42307, #27767, #31230, #13688, #10671, #45326, #31005, #44244, #35149, #24057, #14142, #7225, #38870, #38175, #20602, #41869, #2833, #38396, #10213, #6746, #13460, #20820, #34921, #28213, #27991, #34697, #3526, #21296, #3285, #9133, #17380, #42086, #24755, #45567, #41629, #48, #17612, #13919, #45103, #21066, #31681, #35374, #27529, #10437, #3749, #34473, #30154, #3056, #26680, #24512, #38621, #12602, #6981, #9988, #40776, #23200, #37309, #17145, #5671, #19762, #16925, #14620, #28914, #39999, #21519, #43451, #21747, #14373, #1187, #36075, #15057, #39789, #11818, #15295, #4442, #24984, #11598, #7669, #7444, #35844, #951, #276, #39561, #42771, #8347, #25440, #7916, #22415, #25203, #32391, #25886, #18528, #36518, #21986, #4219, #8137, #22201, #3973, #29143, #28692, #35596, #32610, #18067, #11131, #42995, #32149, #28454, #11361, #39094, #17837, #36293, #31904, #18312, #42553, #43227, #39313, #10915, #25676, #512, #4651, #742, #14841, #18748, #32836, #29379, #9486, #43891, #30484, #41134, #1850, #33954, #29593, #33502, #40662, #23548, #9259, #16404, #36963, #19193, #2305, #12271, #26346, #8585, #44589, #36747, #26786, #44121, #12949, #15956, #5317, #30040, #27035, #19412, #5105, #18981, #23328, #40450, #4879, #33071, #1410, #8804, #22871, #12487, #22649, #26564, #9016, #23086, #33280, #37186, #5550, #15513, #2086, #19644, #37431, #43671, #33736, #12042, #16177, #26111, #30258, #1625, #40226, #5787, #44350, #15724, #29812, #12707, #40891, #19877, #27184, #44497, #34327, #9627, #2698, #9401, #16795, #41272, #24159, #23918, #20014, #45189, #3144, #44968, #5705, #13324, #38039, #10086, #41496, #37567, #41732, #13550, #20240, #41040, #17013, #27624, #38269, #23468, #37802, #17234, #30405, #6615, #30644, #23237, #20690, #27400, #6396, #2924, #34781, #31321, #20479, #33875, #34566, #16559, #16323, #44742, #31090, #9164, #30872, #5924, #45427, #26708, #40807, #37343, #34091, #23690, #19792, #2228, #12859, #26940, #13100, #2456, #6150, #45661, #11005, #24602, #3387, #31998, #14011, #7080, #38965, #28081, #41963, #24846, #20914, #32474, #18168, #27868, #31771, #10306, #35465, #35244, #24379, #28551, #42177, #7315, #35011, #142, #38720, #14232, #31561, #18394, #21161, #39409, #4303, #10769, #42859, #38483, #42400, #3838, #13790, #32244, #25298, #28300, #10527, #11226, #3622, #17710, #17481, #7763, #21392, #35693, #17929, #21840, #370, #14471, #604, #42644, #35933, #6835, #25072, #39186, #7536, #21611, #4070, #14705, #28781, #8438, #29241, #22508, #15380, #43983, #43748, #39873, #19272, #22951, #19065, #25537, #33154, #12126, #29899, #15589, #11688, #15808, #33360, #40077, #15152, #36834, #1704, #12360, #43319, #11898, #37047, #4521, #26437, #4741, #43088, #40536, #1491, #26209, #22741, #8885, #5399, #29671, #8003, #40323, #36379, #36159, #18845, #8676, #29005, #36617, #25761, #19494, #4972, #5186, #823, #8214, #29459, #14923, #11454, #39650, #22069, #32935, #18613, #32699, #1045, #22283, #1280, #43532, #25970, #19735, #26875, #13037, #2176, #16044, #44680, #40746, #6558, #37976, #1942, #5875, #30127, #9574, #9344, #44215, #2637, #33823, #27127, #9104, #19965, #12794, #34039, #5641, #38209, #40985, #13494, #24095, #30577, #16959, #12573, #16496, #23634, #33592, #6331, #45135, #2397, #16268, #31036, #23414, #37516, #37282, #27568, #30346, #9792, #41217, #41672, #37743, #6094, #20184, #10030, #34261, #44438, #26648, #20413, #23173, #16734, #30816, #44911, #13269, #27347, #23859, #41441, #34509, #2868, #14176, #17872, #3326, #38909, #28027, #34956, #10471, #25023, #21333, #28730, #24792, #31501, #310, #21108, #28493, #13952, #24326, #38661, #7017, #17655, #35191, #17423, #31939, #45605, #38430, #42591, #28245, #35411, #17178, #4008, #11169, #14412, #42121, #6780, #10951, #27807, #31716, #18107, #42342, #83, #3567, #10708, #3088, #24547, #7262, #3781, #34729, #39131, #7483, #32189, #20857, #21552, #35635, #550, #14653, #42810, #25241, #39351, #20635, #31265, #10248, #41902, #45367, #13730, #22453, #15327, #36557, #775, #18563, #29847, #11393, #4472, #29623, #29409, #11631, #22230, #33312, #987, #26151, #32645, #25477, #43702, #33104, #1442, #26382, #39595, #22686, #25709, #8167, #7950, #40267, #22017, #7706, #21785, #4255, #36326, #15543, #15759, #43931, #12075, #36108, #36782, #15092, #14875, #35880, #29178, #43261, #12310, #4687, #43030, #39821, #18345, #5138, #32426, #18783, #32874, #1220, #43481, #11849, #25920, #40030, #8384, #19225, #4915, #19012, #8621, #28949, #1657, #19443, #12986, #6036, #23803, #9518, #5586, #9738, #13219, #33986, #9049, #30766, #41390, #27296, #37221, #5824, #16906, #44156, #20356, #44383, #36995, #37915, #27074, #37689, #16679, #34452, #6269, #41167, #1885, #34204, #30291, #30077, #12739, #23584, #22904, #16438, #19678, #30987, #2338, #30519, #45084, #2123, #9291, #2815, #20128, #13440, #44621, #26819, #44857, #40484, #26596, #2574, #33772, #12522, #8836, #40694, #16210, #19910, #23118, #5349, #33537, #15996, #40924, #23361, #37462, #45545, #9966, #3504, #3262, #24035, #42286, #27746, #21039, #34679, #13896, #6724, #27970, #45304, #32124, #20799, #7422, #18044, #24491, #10892, #6504, #10415, #17590, #489, #31881, #39073, #42066, #41848, #24959, #34896, #17354, #31209, #21495, #13663, #3727, #35126, #35572, #38598, #6955, #31661, #3949, #28, #10192, #41608, #253, #31439, #27510, #38155, #20583, #14120, #28193, #10648, #24268, #24727, #3036, #14350, #17124, #38848, #38376, #7201, #21272, #35352, #17815, #28427, #42526, #21724, #929, #39536, #15033, #32363, #19177, #7893, #40202, #5086, #11575, #43651, #39290, #43204, #4628, #33262, #18958, #26088, #29121, #28890, #12020, #21968, #36054, #18289, #8563, #719, #36495, #8117, #22628, #25656, #39769, #22177, #36728, #36272, #14817, #28669, #33054, #4416, #14596, #42747, #11109, #18508, #32587, #18725, #42971, #32813, #1165, #15273, #11337, #29359, #43431, #25179, #11799, #25868, #1391, #7645, #39978, #35817, #8327, #22391, #4196, #4858, #25416, #29575, #15495, #40871, #15934, #37628, #2516, #34145, #44104, #12686, #23747, #5299, #27241, #5525, #43870, #30708, #19853, #44564, #23526, #41333, #44805, #33933, #8785, #41110, #37166, #36946, #19620, #30460, #29790, #23306, #26547, #37860, #9235, #37407, #6208, #8998, #16157, #9683, #2284, #20301, #5765, #33716, #5979, #20071, #33480, #12925, #12468, #19393, #16383, #1826, #40645, #26765, #30018, #12249, #27011, #22853, #9463, #16622, #2065, #13162, #1608, #23066, #30239, #44331 ),
 ( #15705, #26328, #40433, #31387, #34842, #17297, #206, #3206, #34630, #2763, #38792, #27693, #17770, #10838, #42472, #41796, #10146, #45492, #6457, #42021, #13848, #10367, #17074, #24442, #27926, #31835, #31618, #24221, #7147, #24910, #6899, #13385, #20979, #45721, #14298, #3448, #45249, #3683, #21225, #38547, #2987, #24673, #35306, #28370, #31152, #35076, #39024, #38101, #7374, #38329, #30937, #34392, #17545, #14074, #10597, #16857, #45030, #28148, #41555, #42241, #6675, #23981, #20751, #27458, #9909, #20536, #13609, #12582, #29680, #43758, #26659, #28842, #36627, #16054, #22750, #40755, #12136, #39482, #12370, #26446, #7598, #19282, #32313, #11065, #40333, #21674, #14770, #1500, #35767, #3902, #33163, #28619, #21450, #40545, #35526, #8447, #17995, #22517, #25132, #39245, #32067, #5408, #30136, #25365, #42922, #4982, #8895, #439, #19075, #4145, #15598, #18239, #33369, #43993, #1952, #36845, #26218, #8686, #1714, #669, #5196, #11288, #15818, #29908, #22961, #37056, #44224, #19504, #33601, #14541, #42701, #16967, #2405, #12804, #27136, #41225, #6102, #9582, #5883, #6340, #23423, #26886, #31044, #2645, #23868, #5651, #38217, #45375, #20422, #16506, #40993, #2876, #16277, #20192, #6565, #30825, #34272, #37753, #23642, #37291, #37524, #19972, #9800, #23183, #30586, #45143, #20642, #9353, #13501, #27576, #41449, #16742, #41681, #37985, #34048, #44688, #13046, #44448, #30356, #44919, #13277, #34517, #27354, #10037, #2185, #24104, #31273, #34736, #3096, #17185, #13738, #27814, #9114, #19745, #33832, #14658, #7026, #13960, #18114, #21558, #35640, #14880, #28034, #11176, #89, #42349, #42128, #28734, #10479, #41911, #10255, #38437, #10716, #4014, #4260, #32431, #32194, #45613, #25246, #35197, #34963, #24333, #3575, #31722, #18351, #21791, #14182, #6788, #39355, #14420, #39138, #556, #35885, #7711, #28499, #3335, #42815, #28250, #31509, #24798, #25027, #20864, #17879, #21114, #780, #3788, #31945, #17430, #17661, #38916, #24554, #42597, #38669, #316, #7269, #21340, #35417, #10957, #7488, #39827, #18567, #1446, #15098, #22235, #8389, #43266, #11399, #40034, #36112, #1892, #33316, #43036, #1225, #25484, #4920, #4692, #39600, #43707, #29185, #22459, #4477, #15332, #8172, #29416, #994, #33543, #36332, #8841, #19448, #25925, #12315, #7955, #11854, #19017, #28957, #1662, #40490, #43486, #11637, #26389, #18791, #32880, #32651, #22909, #25715, #5144, #36565, #37000, #33109, #15548, #29627, #5355, #12081, #26158, #22023, #15764, #40272, #8628, #22691, #36788, #19230, #29853, #43936, #33776, #23588, #44625, #37693, #44387, #6041, #30523, #13444, #13224, #9296, #34458, #38162, #34207, #40700, #2581, #27301, #45089, #30770, #26823, #30991, #2820, #9524, #30294, #6275, #16912, #27514, #12743, #27077, #6511, #19684, #12527, #41615, #20589, #41394, #23365, #2128, #9742, #23122, #12989, #9973, #20132, #41170, #16684, #2342, #44164, #40930, #37467, #44861, #30082, #5828, #37919, #24042, #16216, #20362, #23809, #34684, #16442, #16000, #26601, #19914, #33991, #9056, #5592, #37227, #10421, #38383, #17822, #10656, #31889, #41854, #13903, #25186, #6731, #45552, #24967, #24738, #6963, #17596, #28675, #42072, #21502, #27977, #20805, #39081, #28437, #42535, #21731, #34904, #18051, #21047, #3512, #3267, #35580, #17362, #3042, #17131, #45310, #31667, #10899, #11117, #39298, #7429, #31447, #32133, #24498, #10199, #31215, #38606, #35132, #7653, #34, #14127, #28199, #13672, #498, #27752, #42293, #38856, #7208, #3958, #24277, #21281, #35359, #3734, #261, #14357, #14604, #42754, #4866, #22187, #29368, #33061, #18515, #8335, #43212, #4427, #25664, #40209, #36502, #43877, #39987, #938, #15502, #36280, #43658, #29127, #39546, #8125, #4637, #32821, #18735, #32595, #1398, #15042, #7903, #12029, #43438, #18967, #25424, #29582, #11806, #26096, #28899, #11585, #12256, #21975, #39777, #8572, #25875, #1173, #15282, #15714, #22399, #22637, #36735, #36061, #5093, #19183, #33269, #8792, #1615, #29799, #26336, #40440, #35827, #4205, #18297, #32374, #727, #14825, #42980, #11346, #27249, #9690, #41118, #44111, #2524, #5532, #1834, #22860, #33723, #16164, #41340, #26773, #12475, #26554, #19402, #16629, #23754, #30246, #19629, #44338, #5986, #36953, #23313, #40652, #37416, #9005, #9471, #20078, #5306, #23533, #40879, #2292, #37635, #2072, #44572, #12693, #9242, #5772, #30716, #27019, #33488, #34153, #19860, #44812, #33940, #13169, #16390, #37174, #30469, #12932, #15943, #30026, #23075, #15633, #32743, #36200, #40370, #11944, #33199, #14965, #1750, #8929, #29716, #25801, #22110, #12175, #25585, #15426, #15858, #40121, #29504, #1323, #4786, #862, #1089, #15203, #19112, #32514, #39914, #8721, #29947, #4563, #22787, #26257, #5021, #18889, #36882, #1536, #18654, #29290, #43366, #8045, #39698, #8256, #32984, #11731, #26012, #43576, #8486, #22322, #22557, #36661, #44031, #43793, #36422, #5232, #40583, #19322, #43135, #33407, #12402, #26481, #22999, #37094, #18436, #29049, #11502, #19782, #41486, #6386, #38030, #2220, #16548, #27614, #9155, #31081, #9390, #1993, #34555, #23680, #2687, #27391, #45179, #2914, #37791, #12622, #44958, #41031, #40797, #23459, #34318, #33640, #27174, #30396, #41723, #13092, #41262, #10077, #12845, #20006, #13541, #6141, #24149, #9618, #37558, #9841, #23909, #37333, #16785, #16314, #23227, #20230, #5695, #44489, #30633, #33867, #16089, #44729, #26700, #5449, #20467, #19544, #5916, #30173, #30864, #26928, #44264, #13315, #34082, #17004, #2447, #24591, #17469, #38708, #10294, #42850, #31551, #18158, #28771, #35234, #21601, #17224, #21151, #28290, #11217, #42635, #4057, #7070, #6824, #35682, #45652, #14001, #41953, #32233, #24369, #14462, #31761, #594, #3613, #17700, #131, #14695, #14220, #38473, #6603, #10996, #28069, #38257, #20681, #34771, #42165, #10516, #42388, #27858, #7305, #10759, #21382, #31309, #3377, #3134, #20904, #35000, #28540, #24836, #38955, #35456, #45417, #3828, #25064, #17917, #31988, #39177, #358, #7527, #13779, #43077, #40313, #29232, #25752, #25525, #43739, #11441, #43975, #39399, #21829, #39864, #4963, #33352, #15799, #19055, #28995, #8667, #18604, #18384, #25286, #32689, #15139, #1694, #8205, #14914, #39639, #7750, #22730, #29888, #43307, #1037, #11676, #29663, #35923, #22273, #7993, #36369, #22059, #36608, #1481, #5177, #40067, #4732, #18833, #22497, #36149, #43523, #32925, #4511, #1271, #12118, #25961, #4294, #29450, #15370, #33145, #11889, #15581, #8429, #26198, #36825, #19263, #32464, #812, #9092, #9563, #26640, #30118, #34251, #5864, #27116, #8877, #41431, #2858, #23623, #19724, #16035, #6084, #19485, #9333, #9782, #34028, #23402, #40971, #44427, #40527, #40736, #23162, #13026, #26427, #33812, #2623, #23849, #44205, #16723, #20171, #44665, #12781, #30807, #41207, #12564, #37270, #5630 ),
 ( #2384, #30334, #44901, #13260, #2165, #37732, #16256, #1932, #30565, #26863, #37505, #19953, #16484, #22941, #27338, #33581, #31028, #37963, #37038, #6319, #5390, #20402, #34498, #16950, #12350, #45358, #38651, #6548, #31492, #24317, #45595, #17170, #3997, #38421, #25013, #35625, #42111, #28481, #24086, #28017, #35182, #18097, #3772, #10940, #13943, #13718, #42582, #6772, #20848, #3079, #39122, #31256, #21324, #7009, #7472, #10462, #24538, #21096, #21543, #3558, #27797, #13485, #17862, #34946, #45127, #27557, #41662, #3314, #17410, #17645, #41893, #31707, #74, #14166, #10238, #28237, #42332, #10017, #10699, #24781, #31930, #38200, #38899, #20627, #7253, #35400, #34720, #301, #14402, #1435, #4906, #25702, #766, #22443, #33097, #19005, #28943, #43253, #8613, #35870, #12067, #36101, #28720, #15536, #4678, #29402, #43021, #4247, #8374, #11842, #25913, #5131, #18337, #29617, #4465, #32636, #32418, #43695, #14867, #32178, #541, #42800, #979, #40023, #40257, #22678, #36549, #11385, #26141, #25468, #25231, #14645, #39587, #22010, #36775, #15083, #21776, #7943, #11160, #39342, #7695, #18554, #29170, #11624, #39814, #8160, #22223, #36317, #18776, #32864, #43474, #1212, #15320, #34619, #5579, #12733, #17063, #1878, #38091, #26590, #33530, #9043, #24208, #20525, #27914, #23969, #30069, #45237, #19670, #27680, #12515, #22897, #37214, #33764, #16204, #2115, #15987, #31140, #44150, #36989, #41785, #26812, #2974, #15751, #3195, #10355, #13597, #40688, #5343, #10135, #26375, #30284, #17284, #41544, #44377, #9896, #6446, #1650, #23112, #38318, #6665, #33305, #20738, #34832, #31373, #19437, #45481, #13837, #42011, #24431, #38535, #19218, #29839, #43921, #12300, #8830, #40477, #14286, #42230, #21664, #14530, #35754, #45711, #17759, #29060, #10583, #3672, #28830, #28606, #10826, #21439, #32524, #194, #25353, #39467, #31823, #24661, #42910, #32301, #655, #25598, #38777, #21905, #24898, #7363, #7135, #7827, #21213, #6888, #20966, #3437, #35515, #14756, #14975, #43146, #11277, #35294, #35990, #28355, #28135, #35063, #42459, #39012, #11512, #3890, #17984, #32054, #17534, #4356, #31607, #425, #11055, #25120, #18446, #39234, #7587, #4133, #18225, #872, #5243, #15868, #19554, #8731, #26023, #33210, #36890, #22331, #12185, #1333, #8266, #29515, #44041, #40380, #2002, #43803, #4796, #19333, #40133, #1760, #32995, #43376, #11955, #8496, #36671, #22567, #36432, #33416, #18899, #11743, #29957, #1547, #22796, #36208, #23009, #30182, #12411, #15437, #25810, #26491, #1100, #5031, #37103, #15642, #19121, #29725, #26266, #22120, #43587, #40592, #8938, #8055, #5459, #33650, #16098, #39923, #44273, #12630, #39708, #4572, #18663, #32753, #15214, #29302, #12130, #43752, #29674, #15812, #26212, #23177, #16048, #37285, #1494, #19276, #30581, #40327, #5189, #30350, #30130, #12364, #22954, #34043, #1708, #44683, #16500, #29902, #43987, #8888, #8680, #44218, #37050, #12576, #36837, #26652, #5402, #5878, #5645, #26440, #26880, #13041, #40749, #33157, #9108, #19739, #37519, #33826, #33363, #23418, #40988, #1946, #22744, #44441, #9348, #19968, #40539, #19498, #27131, #33595, #2400, #2179, #4976, #8441, #16271, #12798, #22511, #36621, #19068, #15592, #2640, #34959, #31039, #30820, #13496, #24329, #23637, #17181, #20417, #31719, #3092, #31269, #86, #2871, #10033, #35194, #41906, #14179, #45371, #27572, #31504, #45609, #27350, #38433, #6334, #44914, #13733, #41444, #34512, #20638, #9795, #37747, #6561, #16737, #41220, #13955, #9577, #41676, #6097, #27810, #16962, #20187, #10251, #23863, #34732, #13272, #24099, #45138, #38213, #37980, #34266, #6784, #21111, #20860, #3331, #24550, #17426, #28030, #42124, #10475, #38665, #7022, #3571, #17658, #25713, #21556, #35638, #31942, #39824, #14417, #4475, #21789, #8170, #25245, #28733, #11173, #22233, #42813, #28496, #42346, #32649, #4012, #11635, #24795, #39354, #7953, #36330, #18788, #22021, #313, #43264, #18112, #21336, #28247, #32192, #554, #4690, #7709, #17876, #42594, #10713, #32878, #1223, #14657, #35883, #4258, #991, #38913, #18349, #10955, #32429, #25026, #39598, #18566, #7266, #43033, #778, #14878, #25482, #39135, #28954, #11397, #7486, #36111, #15096, #29183, #35414, #3784, #26156, #40698, #15762, #23120, #8625, #19015, #33314, #1660, #12313, #29851, #12078, #12525, #29625, #33108, #37225, #8839, #30080, #11852, #44385, #5827, #26599, #22689, #1445, #9054, #22457, #26386, #12741, #36998, #40488, #43934, #22907, #43484, #43705, #40271, #15999, #29414, #36786, #5590, #26821, #15546, #19681, #33774, #1889, #5353, #2126, #44161, #5142, #19228, #19446, #4918, #36562, #33541, #16213, #30292, #40928, #9294, #8387, #23363, #37464, #19912, #33988, #15330, #25923, #40033, #16910, #27975, #41392, #20803, #13222, #20130, #24275, #27750, #41852, #21045, #34206, #17361, #6273, #2818, #2579, #34900, #16682, #2340, #16440, #41169, #27298, #24496, #6039, #44859, #38381, #24040, #20359, #30989, #42070, #9740, #3266, #23806, #30768, #6729, #10197, #31445, #30521, #37917, #45550, #34456, #45086, #13442, #13901, #27512, #44624, #12988, #27075, #41612, #10420, #38603, #6960, #9521, #9971, #23586, #38160, #37691, #6510, #20588, #34682, #3040, #17128, #31213, #45308, #13669, #18511, #43209, #39077, #28434, #7426, #39542, #35130, #32130, #7205, #495, #38853, #723, #11341, #15037, #4201, #21499, #28673, #32369, #17819, #7649, #42531, #3731, #24964, #7899, #35823, #11581, #39295, #257, #14821, #35577, #42976, #10896, #21277, #3955, #18048, #14600, #42752, #31887, #28894, #14354, #35357, #25420, #11113, #18293, #31665, #32591, #25660, #21972, #25183, #21728, #36058, #42290, #4422, #934, #29125, #39773, #8121, #3509, #17594, #32, #14125, #28197, #10653, #24734, #44107, #19624, #39982, #26550, #15938, #8788, #8567, #12471, #36949, #22394, #36498, #25871, #11802, #43434, #29578, #8331, #5302, #29793, #19398, #33483, #15498, #40648, #44334, #40436, #1169, #22856, #1829, #5528, #30022, #33057, #37169, #9001, #15710, #4862, #23071, #33719, #2068, #18963, #33265, #12689, #1394, #16160, #26091, #18729, #30242, #26769, #40874, #22182, #36276, #4633, #32817, #29364, #15278, #12024, #43654, #40205, #22633, #36731, #43873, #5089, #19180, #12252, #26332, #1611, #16625, #23750, #3210, #9912, #45495, #45033, #27244, #45253, #13612, #41114, #6461, #20074, #44567, #27461, #9466, #2519, #34396, #23529, #37411, #20304, #16386, #27929, #27696, #23309, #41336, #5768, #30940, #30712, #19856, #23984, #37631, #2767, #30465, #9686, #34149, #37865, #27015, #13852, #44808, #34845, #9238, #6211, #38332, #33936, #16860, #13389, #2287, #41800, #20755, #41559, #5982, #6678, #13165, #38105, #12928, #17300, #20539, #31155, #34633, #31390, #2990, #17077, #10149, #24224, #10841, #42244, #10370, #672, #35309, #25370, #18460, #4370 ) ),
 .UNSPECIFIED., .T., .F., .T. ) 
 B_SPLINE_SURFACE_WITH_KNOTS ( ( 4, 3, 4 ),
 ( 3, 2, 2, 2, 2, 2, 2, 2, 2, 2, 2, 2, 2, 2, 2, 2, 2, 2, 2, 2, 2, 2, 2, 2, 2, 2, 2, 2, 2, 2, 2, 2, 2, 2, 2, 2, 2, 2, 2, 2, 2, 2, 2, 2, 2, 2, 2, 2, 2, 2, 2, 2, 2, 2, 2, 2, 2, 2, 2, 2, 2, 2, 2, 2, 2, 2, 2, 2, 2, 2, 2, 2, 2, 2, 2, 2, 2, 2, 2, 2, 2, 2, 2, 2, 2, 2, 2, 2, 2, 2, 2, 2, 2, 2, 2, 2, 2, 2, 2, 2, 2, 2, 2, 2, 2, 2, 2, 2, 2, 2, 2, 2, 2, 2, 2, 2, 2, 2, 2, 2, 2, 2, 2, 2, 2, 2, 2, 2, 2, 2, 2, 2, 2, 2, 2, 2, 2, 2, 2, 2, 2, 2, 2, 2, 2, 2, 2, 2, 2, 2, 2, 2, 2, 2, 2, 2, 2, 2, 2, 2, 2, 2, 2, 2, 2, 2, 2, 2, 2, 2, 2, 2, 2, 2, 2, 2, 2, 2, 2, 2, 2, 2, 2, 2, 2, 2, 2, 2, 2, 2, 2, 2, 2, 2, 2, 2, 2, 2, 2, 2, 2, 2, 2, 2, 2, 2, 2, 2, 2, 2, 2, 2, 2, 2, 2, 2, 2, 2, 2, 2, 2, 2, 2, 2, 2, 2, 2, 2, 2, 2, 2, 2, 2, 2, 2, 2, 2, 2, 2, 2, 2, 2, 2, 2, 2, 2, 2, 2, 2, 2, 2, 2, 2, 2, 2, 2, 2, 2, 2, 2, 2, 2, 2, 2, 2, 2, 2, 2, 2, 2, 2, 2, 2, 2, 2, 2, 2, 2, 2, 2, 2, 2, 2, 2, 2, 2, 2, 2, 2, 2, 2, 2, 2, 2, 2, 2, 2, 2, 2, 2, 2, 2, 2, 2, 2, 2, 2, 2, 2, 2, 2, 2, 2, 2, 2, 2, 2, 2, 2, 2, 2, 2, 2, 2, 2, 2, 2, 2, 2, 2, 2, 2, 2, 2, 2, 2, 2, 2, 2, 2, 2, 2, 2, 2, 2, 2, 2, 2, 2, 2, 2, 2, 2, 2, 2, 2, 2, 2, 2, 2, 2, 2, 2, 2, 2, 2, 2, 2, 2, 2, 2, 2, 2, 2, 2, 2, 2, 2, 2, 2, 2, 2, 2, 2, 2, 2, 2, 2, 2, 2, 2, 2, 2, 2, 2, 2, 2, 2, 2, 2, 2, 2, 2, 2, 2, 2, 2, 2, 2, 2, 2, 2, 2, 2, 2, 2, 2, 2, 2, 2, 2, 2, 2, 2, 2, 2, 2, 2, 2, 2, 2, 3 ),
 ( 0.000000000000000000, 0.5000000000000000000, 1.000000000000000000 ),
 ( 0.000000000000000000, 0.002272727272727272617, 0.004545454545454545234, 0.006818181818181817851, 0.009090909090909090468, 0.01136363636363636395, 0.01363636363636363570, 0.01590909090909090745, 0.01818181818181818094, 0.02045454545454545442, 0.02272727272727272790, 0.02500000000000000139, 0.02727272727272727140, 0.02954545454545454489, 0.03181818181818181490, 0.03409090909090908839, 0.03636363636363636187, 0.03863636363636363535, 0.04090909090909090884, 0.04318181818181818232, 0.04545454545454545581, 0.04772727272727272929, 0.05000000000000000278, 0.05227272727272726932, 0.05454545454545454281, 0.05681818181818181629, 0.05909090909090908977, 0.06136363636363636326, 0.06363636363636362980, 0.06590909090909090329, 0.06818181818181817677, 0.07045454545454545026, 0.07272727272727272374, 0.07499999999999999722, 0.07727272727272727071, 0.07954545454545454419, 0.08181818181818181768, 0.08409090909090909116, 0.08636363636363636465, 0.08863636363636363813, 0.09090909090909091161, 0.09318181818181818510, 0.09545454545454545858, 0.09772727272727273207, 0.1000000000000000056, 0.1022727272727272790, 0.1045454545454545386, 0.1068181818181818121, 0.1090909090909090856, 0.1113636363636363591, 0.1136363636363636326, 0.1159090909090909061, 0.1181818181818181795, 0.1204545454545454530, 0.1227272727272727265, 0.1250000000000000000, 0.1272727272727272596, 0.1295454545454545470, 0.1318181818181818066, 0.1340909090909090939, 0.1363636363636363535, 0.1386363636363636409, 0.1409090909090909005, 0.1431818181818181879, 0.1454545454545454475, 0.1477272727272727348, 0.1499999999999999944, 0.1522727272727272818, 0.1545454545454545414, 0.1568181818181818288, 0.1590909090909090884, 0.1613636363636363757, 0.1636363636363636354, 0.1659090909090909227, 0.1681818181818181823, 0.1704545454545454419, 0.1727272727272727293, 0.1749999999999999889, 0.1772727272727272763, 0.1795454545454545359, 0.1818181818181818232, 0.1840909090909090828, 0.1863636363636363702, 0.1886363636363636298, 0.1909090909090909172, 0.1931818181818181768, 0.1954545454545454641, 0.1977272727272727237, 0.2000000000000000111, 0.2022727272727272707, 0.2045454545454545581, 0.2068181818181818177, 0.2090909090909090773, 0.2113636363636363646, 0.2136363636363636243, 0.2159090909090909116, 0.2181818181818181712, 0.2204545454545454586, 0.2227272727272727182, 0.2250000000000000056, 0.2272727272727272652, 0.2295454545454545525, 0.2318181818181818121, 0.2340909090909090995, 0.2363636363636363591, 0.2386363636363636465, 0.2409090909090909061, 0.2431818181818181934, 0.2454545454545454530, 0.2477272727272727404, 0.2500000000000000000, 0.2522727272727272596, 0.2545454545454545192, 0.2568181818181818343, 0.2590909090909090939, 0.2613636363636363535, 0.2636363636363636131, 0.2659090909090909283, 0.2681818181818181879, 0.2704545454545454475, 0.2727272727272727071, 0.2750000000000000222, 0.2772727272727272818, 0.2795454545454545414, 0.2818181818181818010, 0.2840909090909091161, 0.2863636363636363757, 0.2886363636363636354, 0.2909090909090908950, 0.2931818181818181546, 0.2954545454545454697, 0.2977272727272727293, 0.2999999999999999889, 0.3022727272727272485, 0.3045454545454545636, 0.3068181818181818232, 0.3090909090909090828, 0.3113636363636363424, 0.3136363636363636576, 0.3159090909090909172, 0.3181818181818181768, 0.3204545454545454364, 0.3227272727272727515, 0.3250000000000000111, 0.3272727272727272707, 0.3295454545454545303, 0.3318181818181818454, 0.3340909090909091050, 0.3363636363636363646, 0.3386363636363636243, 0.3409090909090908839, 0.3431818181818181990, 0.3454545454545454586, 0.3477272727272727182, 0.3499999999999999778, 0.3522727272727272929, 0.3545454545454545525, 0.3568181818181818121, 0.3590909090909090717, 0.3613636363636363869, 0.3636363636363636465, 0.3659090909090909061, 0.3681818181818181657, 0.3704545454545454808, 0.3727272727272727404, 0.3750000000000000000, 0.3772727272727272596, 0.3795454545454545192, 0.3818181818181818343, 0.3840909090909090939, 0.3863636363636363535, 0.3886363636363636131, 0.3909090909090909283, 0.3931818181818181879, 0.3954545454545454475, 0.3977272727272727071, 0.4000000000000000222, 0.4022727272727272818, 0.4045454545454545414, 0.4068181818181818010, 0.4090909090909091161, 0.4113636363636363757, 0.4136363636363636354, 0.4159090909090908950, 0.4181818181818181546, 0.4204545454545454697, 0.4227272727272727293, 0.4249999999999999889, 0.4272727272727272485, 0.4295454545454545636, 0.4318181818181818232, 0.4340909090909090828, 0.4363636363636363424, 0.4386363636363636576, 0.4409090909090909172, 0.4431818181818181768, 0.4454545454545454364, 0.4477272727272727515, 0.4500000000000000111, 0.4522727272727272707, 0.4545454545454545303, 0.4568181818181818454, 0.4590909090909091050, 0.4613636363636363646, 0.4636363636363636243, 0.4659090909090908839, 0.4681818181818181990, 0.4704545454545454586, 0.4727272727272727182, 0.4749999999999999778, 0.4772727272727272929, 0.4795454545454545525, 0.4818181818181818121, 0.4840909090909090717, 0.4863636363636363869, 0.4886363636363636465, 0.4909090909090909061, 0.4931818181818181657, 0.4954545454545454808, 0.4977272727272727404, 0.5000000000000000000, 0.5022727272727273151, 0.5045454545454545192, 0.5068181818181818343, 0.5090909090909090384, 0.5113636363636363535, 0.5136363636363636687, 0.5159090909090908728, 0.5181818181818181879, 0.5204545454545455030, 0.5227272727272727071, 0.5250000000000000222, 0.5272727272727272263, 0.5295454545454545414, 0.5318181818181818565, 0.5340909090909090606, 0.5363636363636363757, 0.5386363636363636909, 0.5409090909090908950, 0.5431818181818182101, 0.5454545454545454142, 0.5477272727272727293, 0.5500000000000000444, 0.5522727272727272485, 0.5545454545454545636, 0.5568181818181817677, 0.5590909090909090828, 0.5613636363636363980, 0.5636363636363636020, 0.5659090909090909172, 0.5681818181818182323, 0.5704545454545454364, 0.5727272727272727515, 0.5749999999999999556, 0.5772727272727272707, 0.5795454545454545858, 0.5818181818181817899, 0.5840909090909091050, 0.5863636363636363091, 0.5886363636363636243, 0.5909090909090909394, 0.5931818181818181435, 0.5954545454545454586, 0.5977272727272727737, 0.5999999999999999778, 0.6022727272727272929, 0.6045454545454544970, 0.6068181818181818121, 0.6090909090909091272, 0.6113636363636363313, 0.6136363636363636465, 0.6159090909090909616, 0.6181818181818181657, 0.6204545454545454808, 0.6227272727272726849, 0.6250000000000000000, 0.6272727272727273151, 0.6295454545454545192, 0.6318181818181818343, 0.6340909090909090384, 0.6363636363636363535, 0.6386363636363636687, 0.6409090909090908728, 0.6431818181818181879, 0.6454545454545455030, 0.6477272727272727071, 0.6500000000000000222, 0.6522727272727272263, 0.6545454545454545414, 0.6568181818181818565, 0.6590909090909090606, 0.6613636363636363757, 0.6636363636363636909, 0.6659090909090908950, 0.6681818181818182101, 0.6704545454545454142, 0.6727272727272727293, 0.6750000000000000444, 0.6772727272727272485, 0.6795454545454545636, 0.6818181818181817677, 0.6840909090909090828, 0.6863636363636363980, 0.6886363636363636020, 0.6909090909090909172, 0.6931818181818182323, 0.6954545454545454364, 0.6977272727272727515, 0.6999999999999999556, 0.7022727272727272707, 0.7045454545454545858, 0.7068181818181817899, 0.7090909090909091050, 0.7113636363636363091, 0.7136363636363636243, 0.7159090909090909394, 0.7181818181818181435, 0.7204545454545454586, 0.7227272727272727737, 0.7249999999999999778, 0.7272727272727272929, 0.7295454545454544970, 0.7318181818181818121, 0.7340909090909091272, 0.7363636363636363313, 0.7386363636363636465, 0.7409090909090909616, 0.7431818181818181657, 0.7454545454545454808, 0.7477272727272726849, 0.7500000000000000000, 0.7522727272727273151, 0.7545454545454545192, 0.7568181818181818343, 0.7590909090909090384, 0.7613636363636363535, 0.7636363636363636687, 0.7659090909090908728, 0.7681818181818181879, 0.7704545454545455030, 0.7727272727272727071, 0.7750000000000000222, 0.7772727272727272263, 0.7795454545454545414, 0.7818181818181818565, 0.7840909090909090606, 0.7863636363636363757, 0.7886363636363636909, 0.7909090909090908950, 0.7931818181818182101, 0.7954545454545454142, 0.7977272727272727293, 0.8000000000000000444, 0.8022727272727272485, 0.8045454545454545636, 0.8068181818181817677, 0.8090909090909090828, 0.8113636363636363980, 0.8136363636363636020, 0.8159090909090909172, 0.8181818181818182323, 0.8204545454545454364, 0.8227272727272727515, 0.8249999999999999556, 0.8272727272727272707, 0.8295454545454545858, 0.8318181818181817899, 0.8340909090909091050, 0.8363636363636363091, 0.8386363636363636243, 0.8409090909090909394, 0.8431818181818181435, 0.8454545454545454586, 0.8477272727272727737, 0.8499999999999999778, 0.8522727272727272929, 0.8545454545454544970, 0.8568181818181818121, 0.8590909090909091272, 0.8613636363636363313, 0.8636363636363636465, 0.8659090909090909616, 0.8681818181818181657, 0.8704545454545454808, 0.8727272727272726849, 0.8750000000000000000, 0.8772727272727273151, 0.8795454545454545192, 0.8818181818181818343, 0.8840909090909090384, 0.8863636363636363535, 0.8886363636363636687, 0.8909090909090908728, 0.8931818181818181879, 0.8954545454545455030, 0.8977272727272727071, 0.9000000000000000222, 0.9022727272727272263, 0.9045454545454545414, 0.9068181818181818565, 0.9090909090909090606, 0.9113636363636363757, 0.9136363636363636909, 0.9159090909090908950, 0.9181818181818182101, 0.9204545454545454142, 0.9227272727272727293, 0.9250000000000000444, 0.9272727272727272485, 0.9295454545454545636, 0.9318181818181817677, 0.9340909090909090828, 0.9363636363636363980, 0.9386363636363636020, 0.9409090909090909172, 0.9431818181818182323, 0.9454545454545454364, 0.9477272727272727515, 0.9499999999999999556, 0.9522727272727272707, 0.9545454545454545858, 0.9568181818181817899, 0.9590909090909091050, 0.9613636363636363091, 0.9636363636363636243, 0.9659090909090909394, 0.9681818181818181435, 0.9704545454545454586, 0.9727272727272727737, 0.9749999999999999778, 0.9772727272727272929, 0.9781254700864303597 ),
 .UNSPECIFIED. ) 
 GEOMETRIC_REPRESENTATION_ITEM ( )  RATIONAL_B_SPLINE_SURFACE ( (
 ( 1.000000000000000000, 0.9898214418809326842, 1.000000000000000000, 0.9898214418809326842, 1.000000000000000000, 0.9898214418809326842, 1.000000000000000000, 0.9898214418809326842, 1.000000000000000000, 0.9898214418809326842, 1.000000000000000000, 0.9898214418809326842, 1.000000000000000000, 0.9898214418809326842, 1.000000000000000000, 0.9898214418809326842, 1.000000000000000000, 0.9898214418809326842, 1.000000000000000000, 0.9898214418809326842, 1.000000000000000000, 0.9898214418809326842, 1.000000000000000000, 0.9898214418809326842, 1.000000000000000000, 0.9898214418809326842, 1.000000000000000000, 0.9898214418809326842, 1.000000000000000000, 0.9898214418809326842, 1.000000000000000000, 0.9898214418809326842, 1.000000000000000000, 0.9898214418809326842, 1.000000000000000000, 0.9898214418809326842, 1.000000000000000000, 0.9898214418809326842, 1.000000000000000000, 0.9898214418809326842, 1.000000000000000000, 0.9898214418809326842, 1.000000000000000000, 0.9898214418809326842, 1.000000000000000000, 0.9898214418809326842, 1.000000000000000000, 0.9898214418809326842, 1.000000000000000000, 0.9898214418809326842, 1.000000000000000000, 0.9898214418809326842, 1.000000000000000000, 0.9898214418809326842, 1.000000000000000000, 0.9898214418809326842, 1.000000000000000000, 0.9898214418809326842, 1.000000000000000000, 0.9898214418809326842, 1.000000000000000000, 0.9898214418809326842, 1.000000000000000000, 0.9898214418809326842, 1.000000000000000000, 0.9898214418809326842, 1.000000000000000000, 0.9898214418809326842, 1.000000000000000000, 0.9898214418809326842, 1.000000000000000000, 0.9898214418809326842, 1.000000000000000000, 0.9898214418809326842, 1.000000000000000000, 0.9898214418809326842, 1.000000000000000000, 0.9898214418809326842, 1.000000000000000000, 0.9898214418809326842, 1.000000000000000000, 0.9898214418809326842, 1.000000000000000000, 0.9898214418809326842, 1.000000000000000000, 0.9898214418809326842, 1.000000000000000000, 0.9898214418809326842, 1.000000000000000000, 0.9898214418809326842, 1.000000000000000000, 0.9898214418809326842, 1.000000000000000000, 0.9898214418809326842, 1.000000000000000000, 0.9898214418809326842, 1.000000000000000000, 0.9898214418809326842, 1.000000000000000000, 0.9898214418809326842, 1.000000000000000000, 0.9898214418809326842, 1.000000000000000000, 0.9898214418809326842, 1.000000000000000000, 0.9898214418809326842, 1.000000000000000000, 0.9898214418809326842, 1.000000000000000000, 0.9898214418809326842, 1.000000000000000000, 0.9898214418809326842, 1.000000000000000000, 0.9898214418809326842, 1.000000000000000000, 0.9898214418809326842, 1.000000000000000000, 0.9898214418809326842, 1.000000000000000000, 0.9898214418809326842, 1.000000000000000000, 0.9898214418809326842, 1.000000000000000000, 0.9898214418809326842, 1.000000000000000000, 0.9898214418809326842, 1.000000000000000000, 0.9898214418809326842, 1.000000000000000000, 0.9898214418809326842, 1.000000000000000000, 0.9898214418809326842, 1.000000000000000000, 0.9898214418809326842, 1.000000000000000000, 0.9898214418809326842, 1.000000000000000000, 0.9898214418809326842, 1.000000000000000000, 0.9898214418809326842, 1.000000000000000000, 0.9898214418809326842, 1.000000000000000000, 0.9898214418809326842, 1.000000000000000000, 0.9898214418809326842, 1.000000000000000000, 0.9898214418809326842, 1.000000000000000000, 0.9898214418809326842, 1.000000000000000000, 0.9898214418809326842, 1.000000000000000000, 0.9898214418809326842, 1.000000000000000000, 0.9898214418809326842, 1.000000000000000000, 0.9898214418809326842, 1.000000000000000000, 0.9898214418809326842, 1.000000000000000000, 0.9898214418809326842, 1.000000000000000000, 0.9898214418809326842, 1.000000000000000000, 0.9898214418809326842, 1.000000000000000000, 0.9898214418809326842, 1.000000000000000000, 0.9898214418809326842, 1.000000000000000000, 0.9898214418809326842, 1.000000000000000000, 0.9898214418809326842, 1.000000000000000000, 0.9898214418809326842, 1.000000000000000000, 0.9898214418809326842, 1.000000000000000000, 0.9898214418809326842, 1.000000000000000000, 0.9898214418809326842, 1.000000000000000000, 0.9898214418809326842, 1.000000000000000000, 0.9898214418809326842, 1.000000000000000000, 0.9898214418809326842, 1.000000000000000000, 0.9898214418809326842, 1.000000000000000000, 0.9898214418809326842, 1.000000000000000000, 0.9898214418809326842, 1.000000000000000000, 0.9898214418809326842, 1.000000000000000000, 0.9898214418809326842, 1.000000000000000000, 0.9898214418809326842, 1.000000000000000000, 0.9898214418809326842, 1.000000000000000000, 0.9898214418809326842, 1.000000000000000000, 0.9898214418809326842, 1.000000000000000000, 0.9898214418809326842, 1.000000000000000000, 0.9898214418809326842, 1.000000000000000000, 0.9898214418809326842, 1.000000000000000000, 0.9898214418809326842, 1.000000000000000000, 0.9898214418809326842, 1.000000000000000000, 0.9898214418809326842, 1.000000000000000000, 0.9898214418809326842, 1.000000000000000000, 0.9898214418809326842, 1.000000000000000000, 0.9898214418809326842, 1.000000000000000000, 0.9898214418809326842, 1.000000000000000000, 0.9898214418809326842, 1.000000000000000000, 0.9898214418809326842, 1.000000000000000000, 0.9898214418809326842, 1.000000000000000000, 0.9898214418809326842, 1.000000000000000000, 0.9898214418809326842, 1.000000000000000000, 0.9898214418809326842, 1.000000000000000000, 0.9898214418809326842, 1.000000000000000000, 0.9898214418809326842, 1.000000000000000000, 0.9898214418809326842, 1.000000000000000000, 0.9898214418809326842, 1.000000000000000000, 0.9898214418809326842, 1.000000000000000000, 0.9898214418809326842, 1.000000000000000000, 0.9898214418809326842, 1.000000000000000000, 0.9898214418809326842, 1.000000000000000000, 0.9898214418809326842, 1.000000000000000000, 0.9898214418809326842, 1.000000000000000000, 0.9898214418809326842, 1.000000000000000000, 0.9898214418809326842, 1.000000000000000000, 0.9898214418809326842, 1.000000000000000000, 0.9898214418809326842, 1.000000000000000000, 0.9898214418809326842, 1.000000000000000000, 0.9898214418809326842, 1.000000000000000000, 0.9898214418809326842, 1.000000000000000000, 0.9898214418809326842, 1.000000000000000000, 0.9898214418809326842, 1.000000000000000000, 0.9898214418809326842, 1.000000000000000000, 0.9898214418809326842, 1.000000000000000000, 0.9898214418809326842, 1.000000000000000000, 0.9898214418809326842, 1.000000000000000000, 0.9898214418809326842, 1.000000000000000000, 0.9898214418809326842, 1.000000000000000000, 0.9898214418809326842, 1.000000000000000000, 0.9898214418809326842, 1.000000000000000000, 0.9898214418809326842, 1.000000000000000000, 0.9898214418809326842, 1.000000000000000000, 0.9898214418809326842, 1.000000000000000000, 0.9898214418809326842, 1.000000000000000000, 0.9898214418809326842, 1.000000000000000000, 0.9898214418809326842, 1.000000000000000000, 0.9898214418809326842, 1.000000000000000000, 0.9898214418809326842, 1.000000000000000000, 0.9898214418809326842, 1.000000000000000000, 0.9898214418809326842, 1.000000000000000000, 0.9898214418809326842, 1.000000000000000000, 0.9898214418809326842, 1.000000000000000000, 0.9898214418809326842, 1.000000000000000000, 0.9898214418809326842, 1.000000000000000000, 0.9898214418809326842, 1.000000000000000000, 0.9898214418809326842, 1.000000000000000000, 0.9898214418809326842, 1.000000000000000000, 0.9898214418809326842, 1.000000000000000000, 0.9898214418809326842, 1.000000000000000000, 0.9898214418809326842, 1.000000000000000000, 0.9898214418809326842, 1.000000000000000000, 0.9898214418809326842, 1.000000000000000000, 0.9898214418809326842, 1.000000000000000000, 0.9898214418809326842, 1.000000000000000000, 0.9898214418809326842, 1.000000000000000000, 0.9898214418809326842, 1.000000000000000000, 0.9898214418809326842, 1.000000000000000000, 0.9898214418809326842, 1.000000000000000000, 0.9898214418809326842, 1.000000000000000000, 0.9898214418809326842, 1.000000000000000000, 0.9898214418809326842, 1.000000000000000000, 0.9898214418809326842, 1.000000000000000000, 0.9898214418809326842, 1.000000000000000000, 0.9898214418809326842, 1.000000000000000000, 0.9898214418809326842, 1.000000000000000000, 0.9898214418809326842, 1.000000000000000000, 0.9898214418809326842, 1.000000000000000000, 0.9898214418809326842, 1.000000000000000000, 0.9898214418809326842, 1.000000000000000000, 0.9898214418809326842, 1.000000000000000000, 0.9898214418809326842, 1.000000000000000000, 0.9898214418809326842, 1.000000000000000000, 0.9898214418809326842, 1.000000000000000000, 0.9898214418809326842, 1.000000000000000000, 0.9898214418809326842, 1.000000000000000000, 0.9898214418809326842, 1.000000000000000000, 0.9898214418809326842, 1.000000000000000000, 0.9898214418809326842, 1.000000000000000000, 0.9898214418809326842, 1.000000000000000000, 0.9898214418809326842, 1.000000000000000000, 0.9898214418809326842, 1.000000000000000000, 0.9898214418809326842, 1.000000000000000000, 0.9898214418809326842, 1.000000000000000000, 0.9898214418809326842, 1.000000000000000000, 0.9898214418809326842, 1.000000000000000000, 0.9898214418809326842, 1.000000000000000000, 0.9898214418809326842, 1.000000000000000000, 0.9898214418809326842, 1.000000000000000000, 0.9898214418809326842, 1.000000000000000000, 0.9898214418809326842, 1.000000000000000000, 0.9898214418809326842, 1.000000000000000000, 0.9898214418809326842, 1.000000000000000000, 0.9898214418809326842, 1.000000000000000000, 0.9898214418809326842, 1.000000000000000000, 0.9898214418809326842, 1.000000000000000000, 0.9898214418809326842, 1.000000000000000000, 0.9898214418809326842, 1.000000000000000000, 0.9898214418809326842, 1.000000000000000000, 0.9898214418809326842, 1.000000000000000000, 0.9898214418809326842, 1.000000000000000000, 0.9898214418809326842, 1.000000000000000000, 0.9898214418809326842, 1.000000000000000000, 0.9898214418809326842, 1.000000000000000000, 0.9898214418809326842, 1.000000000000000000, 0.9898214418809326842, 1.000000000000000000, 0.9898214418809326842, 1.000000000000000000, 0.9898214418809326842, 1.000000000000000000, 0.9898214418809326842, 1.000000000000000000, 0.9898214418809326842, 1.000000000000000000, 0.9898214418809326842, 1.000000000000000000, 0.9898214418809326842, 1.000000000000000000, 0.9898214418809326842, 1.000000000000000000, 0.9898214418809326842, 1.000000000000000000, 0.9898214418809326842, 1.000000000000000000, 0.9898214418809326842, 1.000000000000000000, 0.9898214418809326842, 1.000000000000000000, 0.9898214418809326842, 1.000000000000000000, 0.9898214418809326842, 1.000000000000000000, 0.9898214418809326842, 1.000000000000000000, 0.9898214418809326842, 1.000000000000000000, 0.9898214418809326842, 1.000000000000000000, 0.9898214418809326842, 1.000000000000000000, 0.9898214418809326842, 1.000000000000000000, 0.9898214418809326842, 1.000000000000000000, 0.9898214418809326842, 1.000000000000000000, 0.9898214418809326842, 1.000000000000000000, 0.9898214418809326842, 1.000000000000000000, 0.9898214418809326842, 1.000000000000000000, 0.9898214418809326842, 1.000000000000000000, 0.9898214418809326842, 1.000000000000000000, 0.9898214418809326842, 1.000000000000000000, 0.9898214418809326842, 1.000000000000000000, 0.9898214418809326842, 1.000000000000000000, 0.9898214418809326842, 1.000000000000000000, 0.9898214418809326842, 1.000000000000000000, 0.9898214418809326842, 1.000000000000000000, 0.9898214418809326842, 1.000000000000000000, 0.9898214418809326842, 1.000000000000000000, 0.9898214418809326842, 1.000000000000000000, 0.9898214418809326842, 1.000000000000000000, 0.9898214418809326842, 1.000000000000000000, 0.9898214418809326842, 1.000000000000000000, 0.9898214418809326842, 1.000000000000000000, 0.9898214418809326842, 1.000000000000000000, 0.9898214418809326842, 1.000000000000000000, 0.9898214418809326842, 1.000000000000000000, 0.9898214418809326842, 1.000000000000000000, 0.9898214418809326842, 1.000000000000000000, 0.9898214418809326842, 1.000000000000000000, 0.9898214418809326842, 1.000000000000000000, 0.9898214418809326842, 1.000000000000000000, 0.9898214418809326842, 1.000000000000000000, 0.9898214418809326842, 1.000000000000000000, 0.9898214418809326842, 1.000000000000000000, 0.9898214418809326842, 1.000000000000000000, 0.9898214418809326842, 1.000000000000000000, 0.9898214418809326842, 1.000000000000000000, 0.9898214418809326842, 1.000000000000000000, 0.9898214418809326842, 1.000000000000000000, 0.9898214418809326842, 1.000000000000000000, 0.9898214418809326842, 1.000000000000000000, 0.9898214418809326842, 1.000000000000000000, 0.9898214418809326842, 1.000000000000000000, 0.9898214418809326842, 1.000000000000000000, 0.9898214418809326842, 1.000000000000000000, 0.9898214418809326842, 1.000000000000000000, 0.9898214418809326842, 1.000000000000000000, 0.9898214418809326842, 1.000000000000000000, 0.9898214418809326842, 1.000000000000000000, 0.9898214418809326842, 1.000000000000000000, 0.9898214418809326842, 1.000000000000000000, 0.9898214418809326842, 1.000000000000000000, 0.9898214418809326842, 1.000000000000000000, 0.9898214418809326842, 1.000000000000000000, 0.9898214418809326842, 1.000000000000000000, 0.9898214418809326842, 1.000000000000000000, 0.9898214418809326842, 1.000000000000000000, 0.9898214418809326842, 1.000000000000000000, 0.9898214418809326842, 1.000000000000000000, 0.9898214418809326842, 1.000000000000000000, 0.9898214418809326842, 1.000000000000000000, 0.9898214418809326842, 1.000000000000000000, 0.9898214418809326842, 1.000000000000000000, 0.9898214418809326842, 1.000000000000000000, 0.9898214418809326842, 1.000000000000000000, 0.9898214418809326842, 1.000000000000000000, 0.9898214418809326842, 1.000000000000000000, 0.9898214418809326842, 1.000000000000000000, 0.9898214418809326842, 1.000000000000000000, 0.9898214418809326842, 1.000000000000000000, 0.9898214418809326842, 1.000000000000000000, 0.9898214418809326842, 1.000000000000000000, 0.9898214418809326842, 1.000000000000000000, 0.9898214418809326842, 1.000000000000000000, 0.9898214418809326842, 1.000000000000000000, 0.9898214418809326842, 1.000000000000000000, 0.9898214418809326842, 1.000000000000000000, 0.9898214418809326842, 1.000000000000000000, 0.9898214418809326842, 1.000000000000000000, 0.9898214418809326842, 1.000000000000000000, 0.9898214418809326842, 1.000000000000000000, 0.9898214418809326842, 1.000000000000000000, 0.9898214418809326842, 1.000000000000000000, 0.9898214418809326842, 1.000000000000000000, 0.9898214418809326842, 1.000000000000000000, 0.9898214418809326842, 1.000000000000000000, 0.9898214418809326842, 1.000000000000000000, 0.9898214418809326842, 1.000000000000000000, 0.9898214418809326842, 1.000000000000000000, 0.9898214418809326842, 1.000000000000000000, 0.9898214418809326842, 1.000000000000000000, 0.9898214418809326842, 1.000000000000000000, 0.9898214418809326842, 1.000000000000000000, 0.9898214418809326842, 1.000000000000000000, 0.9898214418809326842, 1.000000000000000000, 0.9898214418809326842, 1.000000000000000000, 0.9898214418809326842, 1.000000000000000000, 0.9898214418809326842, 1.000000000000000000, 0.9898214418809326842, 1.000000000000000000, 0.9898214418809326842, 1.000000000000000000, 0.9898214418809326842, 1.000000000000000000, 0.9898214418809326842, 1.000000000000000000, 0.9898214418809326842, 1.000000000000000000, 0.9898214418809326842, 1.000000000000000000, 0.9898214418809326842, 1.000000000000000000, 0.9898214418809326842, 1.000000000000000000, 0.9898214418809326842, 1.000000000000000000, 0.9898214418809326842, 1.000000000000000000, 0.9898214418809326842, 1.000000000000000000, 0.9898214418809326842, 1.000000000000000000, 0.9898214418809326842, 1.000000000000000000, 0.9898214418809326842, 1.000000000000000000, 0.9898214418809326842, 1.000000000000000000, 0.9898214418809326842, 1.000000000000000000, 0.9898214418809326842, 1.000000000000000000, 0.9898214418809326842, 1.000000000000000000, 0.9898214418809326842, 1.000000000000000000, 0.9898214418809326842, 1.000000000000000000, 0.9898214418809326842, 1.000000000000000000, 0.9898214418809326842, 1.000000000000000000, 0.9898214418809326842, 1.000000000000000000, 0.9898214418809326842, 1.000000000000000000, 0.9898214418809326842, 1.000000000000000000, 0.9898214418809326842, 1.000000000000000000, 0.9898214418809326842, 1.000000000000000000, 0.9898214418809326842, 1.000000000000000000, 0.9898214418809326842, 1.000000000000000000, 0.9898214418809326842, 1.000000000000000000, 0.9898214418809326842, 1.000000000000000000, 0.9898214418809326842, 1.000000000000000000, 0.9898214418809326842, 1.000000000000000000, 0.9898214418809326842, 1.000000000000000000, 0.9898214418809326842, 1.000000000000000000, 0.9898214418809326842, 1.000000000000000000, 0.9898214418809326842, 1.000000000000000000, 0.9898214418809326842, 1.000000000000000000, 0.9898214418809326842, 1.000000000000000000, 0.9898214418809326842, 1.000000000000000000, 0.9898214418809326842, 1.000000000000000000, 0.9898214418809326842, 1.000000000000000000, 0.9898214418809326842, 1.000000000000000000, 0.9898214418809326842, 1.000000000000000000, 0.9898214418809326842, 1.000000000000000000, 0.9898214418809326842, 1.000000000000000000, 0.9898214418809326842, 1.000000000000000000, 0.9898214418809326842, 1.000000000000000000, 0.9898214418809326842, 1.000000000000000000, 0.9898214418809326842, 1.000000000000000000, 0.9898214418809326842, 1.000000000000000000, 0.9898214418809326842, 1.000000000000000000, 0.9898214418809326842, 1.000000000000000000, 0.9898214418809326842, 1.000000000000000000, 0.9898214418809326842, 1.000000000000000000, 0.9898214418809326842, 1.000000000000000000, 0.9898214418809326842, 1.000000000000000000, 0.9898214418809326842, 1.000000000000000000, 0.9898214418809326842, 1.000000000000000000, 0.9898214418809326842, 1.000000000000000000, 0.9898214418809326842, 1.000000000000000000, 0.9898214418809326842, 1.000000000000000000, 0.9898214418809326842, 1.000000000000000000, 0.9898214418809326842, 1.000000000000000000, 0.9898214418809326842, 1.000000000000000000, 0.9898214418809326842, 1.000000000000000000, 0.9898214418809326842, 1.000000000000000000, 0.9898214418809326842, 1.000000000000000000, 0.9898214418809326842, 1.000000000000000000, 0.9898214418809326842, 1.000000000000000000, 0.9898214418809326842, 1.000000000000000000, 0.9898214418809326842, 1.000000000000000000, 0.9898214418809326842, 1.000000000000000000, 0.9898214418809326842, 1.000000000000000000, 0.9898214418809326842, 1.000000000000000000, 0.9898214418809326842, 1.000000000000000000, 0.9898214418809326842, 1.000000000000000000, 0.9898214418809326842, 1.000000000000000000, 0.9898214418809326842, 1.000000000000000000, 0.9898214418809326842, 1.000000000000000000, 0.9898214418809326842, 1.000000000000000000, 0.9898214418809326842, 1.000000000000000000, 0.9898214418809326842, 1.000000000000000000, 0.9898214418809326842, 1.000000000000000000, 0.9898214418809326842, 1.000000000000000000, 0.9898214418809326842, 1.000000000000000000, 0.9898214418809326842, 1.000000000000000000, 0.9898214418809326842, 1.000000000000000000, 0.9898214418809326842, 1.000000000000000000, 0.9898214418809326842, 1.000000000000000000, 0.9898214418809326842, 1.000000000000000000, 0.9898214418809326842, 1.000000000000000000, 0.9898214418809326842, 1.000000000000000000, 0.9898214418809326842, 1.000000000000000000, 0.9898214418809326842, 1.000000000000000000, 0.9898214418809326842, 1.000000000000000000, 0.9961809353924466759, 0.9952277490961531914),
 ( 0.3333333333333333703, 0.3299404806269776169, 0.3333333333333333703, 0.3299404806269776169, 0.3333333333333333703, 0.3299404806269776169, 0.3333333333333333703, 0.3299404806269776169, 0.3333333333333333703, 0.3299404806269776169, 0.3333333333333333703, 0.3299404806269776169, 0.3333333333333333703, 0.3299404806269776169, 0.3333333333333333703, 0.3299404806269776169, 0.3333333333333333703, 0.3299404806269776169, 0.3333333333333333703, 0.3299404806269776169, 0.3333333333333333703, 0.3299404806269776169, 0.3333333333333333703, 0.3299404806269776169, 0.3333333333333333703, 0.3299404806269776169, 0.3333333333333333703, 0.3299404806269776169, 0.3333333333333333703, 0.3299404806269776169, 0.3333333333333333703, 0.3299404806269776169, 0.3333333333333333703, 0.3299404806269776169, 0.3333333333333333703, 0.3299404806269776169, 0.3333333333333333703, 0.3299404806269776169, 0.3333333333333333703, 0.3299404806269776169, 0.3333333333333333703, 0.3299404806269776169, 0.3333333333333333703, 0.3299404806269776169, 0.3333333333333333703, 0.3299404806269776169, 0.3333333333333333703, 0.3299404806269776169, 0.3333333333333333703, 0.3299404806269776169, 0.3333333333333333703, 0.3299404806269776169, 0.3333333333333333703, 0.3299404806269776169, 0.3333333333333333703, 0.3299404806269776169, 0.3333333333333333703, 0.3299404806269776169, 0.3333333333333333703, 0.3299404806269776169, 0.3333333333333333703, 0.3299404806269776169, 0.3333333333333333703, 0.3299404806269776169, 0.3333333333333333703, 0.3299404806269776169, 0.3333333333333333703, 0.3299404806269776169, 0.3333333333333333703, 0.3299404806269776169, 0.3333333333333333703, 0.3299404806269776169, 0.3333333333333333703, 0.3299404806269776169, 0.3333333333333333703, 0.3299404806269776169, 0.3333333333333333703, 0.3299404806269776169, 0.3333333333333333703, 0.3299404806269776169, 0.3333333333333333703, 0.3299404806269776169, 0.3333333333333333703, 0.3299404806269776169, 0.3333333333333333703, 0.3299404806269776169, 0.3333333333333333703, 0.3299404806269776169, 0.3333333333333333703, 0.3299404806269776169, 0.3333333333333333703, 0.3299404806269776169, 0.3333333333333333703, 0.3299404806269776169, 0.3333333333333333703, 0.3299404806269776169, 0.3333333333333333703, 0.3299404806269776169, 0.3333333333333333703, 0.3299404806269776169, 0.3333333333333333703, 0.3299404806269776169, 0.3333333333333333703, 0.3299404806269776169, 0.3333333333333333703, 0.3299404806269776169, 0.3333333333333333703, 0.3299404806269776169, 0.3333333333333333703, 0.3299404806269776169, 0.3333333333333333703, 0.3299404806269776169, 0.3333333333333333703, 0.3299404806269776169, 0.3333333333333333703, 0.3299404806269776169, 0.3333333333333333703, 0.3299404806269776169, 0.3333333333333333703, 0.3299404806269776169, 0.3333333333333333703, 0.3299404806269776169, 0.3333333333333333703, 0.3299404806269776169, 0.3333333333333333703, 0.3299404806269776169, 0.3333333333333333703, 0.3299404806269776169, 0.3333333333333333703, 0.3299404806269776169, 0.3333333333333333703, 0.3299404806269776169, 0.3333333333333333703, 0.3299404806269776169, 0.3333333333333333703, 0.3299404806269776169, 0.3333333333333333703, 0.3299404806269776169, 0.3333333333333333703, 0.3299404806269776169, 0.3333333333333333703, 0.3299404806269776169, 0.3333333333333333703, 0.3299404806269776169, 0.3333333333333333703, 0.3299404806269776169, 0.3333333333333333703, 0.3299404806269776169, 0.3333333333333333703, 0.3299404806269776169, 0.3333333333333333703, 0.3299404806269776169, 0.3333333333333333703, 0.3299404806269776169, 0.3333333333333333703, 0.3299404806269776169, 0.3333333333333333703, 0.3299404806269776169, 0.3333333333333333703, 0.3299404806269776169, 0.3333333333333333703, 0.3299404806269776169, 0.3333333333333333703, 0.3299404806269776169, 0.3333333333333333703, 0.3299404806269776169, 0.3333333333333333703, 0.3299404806269776169, 0.3333333333333333703, 0.3299404806269776169, 0.3333333333333333703, 0.3299404806269776169, 0.3333333333333333703, 0.3299404806269776169, 0.3333333333333333703, 0.3299404806269776169, 0.3333333333333333703, 0.3299404806269776169, 0.3333333333333333703, 0.3299404806269776169, 0.3333333333333333703, 0.3299404806269776169, 0.3333333333333333703, 0.3299404806269776169, 0.3333333333333333703, 0.3299404806269776169, 0.3333333333333333703, 0.3299404806269776169, 0.3333333333333333703, 0.3299404806269776169, 0.3333333333333333703, 0.3299404806269776169, 0.3333333333333333703, 0.3299404806269776169, 0.3333333333333333703, 0.3299404806269776169, 0.3333333333333333703, 0.3299404806269776169, 0.3333333333333333703, 0.3299404806269776169, 0.3333333333333333703, 0.3299404806269776169, 0.3333333333333333703, 0.3299404806269776169, 0.3333333333333333703, 0.3299404806269776169, 0.3333333333333333703, 0.3299404806269776169, 0.3333333333333333703, 0.3299404806269776169, 0.3333333333333333703, 0.3299404806269776169, 0.3333333333333333703, 0.3299404806269776169, 0.3333333333333333703, 0.3299404806269776169, 0.3333333333333333703, 0.3299404806269776169, 0.3333333333333333703, 0.3299404806269776169, 0.3333333333333333703, 0.3299404806269776169, 0.3333333333333333703, 0.3299404806269776169, 0.3333333333333333703, 0.3299404806269776169, 0.3333333333333333703, 0.3299404806269776169, 0.3333333333333333703, 0.3299404806269776169, 0.3333333333333333703, 0.3299404806269776169, 0.3333333333333333703, 0.3299404806269776169, 0.3333333333333333703, 0.3299404806269776169, 0.3333333333333333703, 0.3299404806269776169, 0.3333333333333333703, 0.3299404806269776169, 0.3333333333333333703, 0.3299404806269776169, 0.3333333333333333703, 0.3299404806269776169, 0.3333333333333333703, 0.3299404806269776169, 0.3333333333333333703, 0.3299404806269776169, 0.3333333333333333703, 0.3299404806269776169, 0.3333333333333333703, 0.3299404806269776169, 0.3333333333333333703, 0.3299404806269776169, 0.3333333333333333703, 0.3299404806269776169, 0.3333333333333333703, 0.3299404806269776169, 0.3333333333333333703, 0.3299404806269776169, 0.3333333333333333703, 0.3299404806269776169, 0.3333333333333333703, 0.3299404806269776169, 0.3333333333333333703, 0.3299404806269776169, 0.3333333333333333703, 0.3299404806269776169, 0.3333333333333333703, 0.3299404806269776169, 0.3333333333333333703, 0.3299404806269776169, 0.3333333333333333703, 0.3299404806269776169, 0.3333333333333333703, 0.3299404806269776169, 0.3333333333333333703, 0.3299404806269776169, 0.3333333333333333703, 0.3299404806269776169, 0.3333333333333333703, 0.3299404806269776169, 0.3333333333333333703, 0.3299404806269776169, 0.3333333333333333703, 0.3299404806269776169, 0.3333333333333333703, 0.3299404806269776169, 0.3333333333333333703, 0.3299404806269776169, 0.3333333333333333703, 0.3299404806269776169, 0.3333333333333333703, 0.3299404806269776169, 0.3333333333333333703, 0.3299404806269776169, 0.3333333333333333703, 0.3299404806269776169, 0.3333333333333333703, 0.3299404806269776169, 0.3333333333333333703, 0.3299404806269776169, 0.3333333333333333703, 0.3299404806269776169, 0.3333333333333333703, 0.3299404806269776169, 0.3333333333333333703, 0.3299404806269776169, 0.3333333333333333703, 0.3299404806269776169, 0.3333333333333333703, 0.3299404806269776169, 0.3333333333333333703, 0.3299404806269776169, 0.3333333333333333703, 0.3299404806269776169, 0.3333333333333333703, 0.3299404806269776169, 0.3333333333333333703, 0.3299404806269776169, 0.3333333333333333703, 0.3299404806269776169, 0.3333333333333333703, 0.3299404806269776169, 0.3333333333333333703, 0.3299404806269776169, 0.3333333333333333703, 0.3299404806269776169, 0.3333333333333333703, 0.3299404806269776169, 0.3333333333333333703, 0.3299404806269776169, 0.3333333333333333703, 0.3299404806269776169, 0.3333333333333333703, 0.3299404806269776169, 0.3333333333333333703, 0.3299404806269776169, 0.3333333333333333703, 0.3299404806269776169, 0.3333333333333333703, 0.3299404806269776169, 0.3333333333333333703, 0.3299404806269776169, 0.3333333333333333703, 0.3299404806269776169, 0.3333333333333333703, 0.3299404806269776169, 0.3333333333333333703, 0.3299404806269776169, 0.3333333333333333703, 0.3299404806269776169, 0.3333333333333333703, 0.3299404806269776169, 0.3333333333333333703, 0.3299404806269776169, 0.3333333333333333703, 0.3299404806269776169, 0.3333333333333333703, 0.3299404806269776169, 0.3333333333333333703, 0.3299404806269776169, 0.3333333333333333703, 0.3299404806269776169, 0.3333333333333333703, 0.3299404806269776169, 0.3333333333333333703, 0.3299404806269776169, 0.3333333333333333703, 0.3299404806269776169, 0.3333333333333333703, 0.3299404806269776169, 0.3333333333333333703, 0.3299404806269776169, 0.3333333333333333703, 0.3299404806269776169, 0.3333333333333333703, 0.3299404806269776169, 0.3333333333333333703, 0.3299404806269776169, 0.3333333333333333703, 0.3299404806269776169, 0.3333333333333333703, 0.3299404806269776169, 0.3333333333333333703, 0.3299404806269776169, 0.3333333333333333703, 0.3299404806269776169, 0.3333333333333333703, 0.3299404806269776169, 0.3333333333333333703, 0.3299404806269776169, 0.3333333333333333703, 0.3299404806269776169, 0.3333333333333333703, 0.3299404806269776169, 0.3333333333333333703, 0.3299404806269776169, 0.3333333333333333703, 0.3299404806269776169, 0.3333333333333333703, 0.3299404806269776169, 0.3333333333333333703, 0.3299404806269776169, 0.3333333333333333703, 0.3299404806269776169, 0.3333333333333333703, 0.3299404806269776169, 0.3333333333333333703, 0.3299404806269776169, 0.3333333333333333703, 0.3299404806269776169, 0.3333333333333333703, 0.3299404806269776169, 0.3333333333333333703, 0.3299404806269776169, 0.3333333333333333703, 0.3299404806269776169, 0.3333333333333333703, 0.3299404806269776169, 0.3333333333333333703, 0.3299404806269776169, 0.3333333333333333703, 0.3299404806269776169, 0.3333333333333333703, 0.3299404806269776169, 0.3333333333333333703, 0.3299404806269776169, 0.3333333333333333703, 0.3299404806269776169, 0.3333333333333333703, 0.3299404806269776169, 0.3333333333333333703, 0.3299404806269776169, 0.3333333333333333703, 0.3299404806269776169, 0.3333333333333333703, 0.3299404806269776169, 0.3333333333333333703, 0.3299404806269776169, 0.3333333333333333703, 0.3299404806269776169, 0.3333333333333333703, 0.3299404806269776169, 0.3333333333333333703, 0.3299404806269776169, 0.3333333333333333703, 0.3299404806269776169, 0.3333333333333333703, 0.3299404806269776169, 0.3333333333333333703, 0.3299404806269776169, 0.3333333333333333703, 0.3299404806269776169, 0.3333333333333333703, 0.3299404806269776169, 0.3333333333333333703, 0.3299404806269776169, 0.3333333333333333703, 0.3299404806269776169, 0.3333333333333333703, 0.3299404806269776169, 0.3333333333333333703, 0.3299404806269776169, 0.3333333333333333703, 0.3299404806269776169, 0.3333333333333333703, 0.3299404806269776169, 0.3333333333333333703, 0.3299404806269776169, 0.3333333333333333703, 0.3299404806269776169, 0.3333333333333333703, 0.3299404806269776169, 0.3333333333333333703, 0.3299404806269776169, 0.3333333333333333703, 0.3299404806269776169, 0.3333333333333333703, 0.3299404806269776169, 0.3333333333333333703, 0.3299404806269776169, 0.3333333333333333703, 0.3299404806269776169, 0.3333333333333333703, 0.3299404806269776169, 0.3333333333333333703, 0.3299404806269776169, 0.3333333333333333703, 0.3299404806269776169, 0.3333333333333333703, 0.3299404806269776169, 0.3333333333333333703, 0.3299404806269776169, 0.3333333333333333703, 0.3299404806269776169, 0.3333333333333333703, 0.3299404806269776169, 0.3333333333333333703, 0.3299404806269776169, 0.3333333333333333703, 0.3299404806269776169, 0.3333333333333333703, 0.3299404806269776169, 0.3333333333333333703, 0.3299404806269776169, 0.3333333333333333703, 0.3299404806269776169, 0.3333333333333333703, 0.3299404806269776169, 0.3333333333333333703, 0.3299404806269776169, 0.3333333333333333703, 0.3299404806269776169, 0.3333333333333333703, 0.3299404806269776169, 0.3333333333333333703, 0.3299404806269776169, 0.3333333333333333703, 0.3299404806269776169, 0.3333333333333333703, 0.3299404806269776169, 0.3333333333333333703, 0.3299404806269776169, 0.3333333333333333703, 0.3299404806269776169, 0.3333333333333333703, 0.3299404806269776169, 0.3333333333333333703, 0.3299404806269776169, 0.3333333333333333703, 0.3299404806269776169, 0.3333333333333333703, 0.3299404806269776169, 0.3333333333333333703, 0.3299404806269776169, 0.3333333333333333703, 0.3299404806269776169, 0.3333333333333333703, 0.3299404806269776169, 0.3333333333333333703, 0.3299404806269776169, 0.3333333333333333703, 0.3299404806269776169, 0.3333333333333333703, 0.3299404806269776169, 0.3333333333333333703, 0.3299404806269776169, 0.3333333333333333703, 0.3299404806269776169, 0.3333333333333333703, 0.3299404806269776169, 0.3333333333333333703, 0.3299404806269776169, 0.3333333333333333703, 0.3299404806269776169, 0.3333333333333333703, 0.3299404806269776169, 0.3333333333333333703, 0.3299404806269776169, 0.3333333333333333703, 0.3299404806269776169, 0.3333333333333333703, 0.3299404806269776169, 0.3333333333333333703, 0.3299404806269776169, 0.3333333333333333703, 0.3299404806269776169, 0.3333333333333333703, 0.3299404806269776169, 0.3333333333333333703, 0.3299404806269776169, 0.3333333333333333703, 0.3299404806269776169, 0.3333333333333333703, 0.3299404806269776169, 0.3333333333333333703, 0.3299404806269776169, 0.3333333333333333703, 0.3299404806269776169, 0.3333333333333333703, 0.3299404806269776169, 0.3333333333333333703, 0.3299404806269776169, 0.3333333333333333703, 0.3299404806269776169, 0.3333333333333333703, 0.3299404806269776169, 0.3333333333333333703, 0.3299404806269776169, 0.3333333333333333703, 0.3299404806269776169, 0.3333333333333333703, 0.3299404806269776169, 0.3333333333333333703, 0.3299404806269776169, 0.3333333333333333703, 0.3299404806269776169, 0.3333333333333333703, 0.3299404806269776169, 0.3333333333333333703, 0.3299404806269776169, 0.3333333333333333703, 0.3299404806269776169, 0.3333333333333333703, 0.3299404806269776169, 0.3333333333333333703, 0.3299404806269776169, 0.3333333333333333703, 0.3299404806269776169, 0.3333333333333333703, 0.3299404806269776169, 0.3333333333333333703, 0.3299404806269776169, 0.3333333333333333703, 0.3299404806269776169, 0.3333333333333333703, 0.3299404806269776169, 0.3333333333333333703, 0.3299404806269776169, 0.3333333333333333703, 0.3299404806269776169, 0.3333333333333333703, 0.3299404806269776169, 0.3333333333333333703, 0.3299404806269776169, 0.3333333333333333703, 0.3299404806269776169, 0.3333333333333333703, 0.3299404806269776169, 0.3333333333333333703, 0.3299404806269776169, 0.3333333333333333703, 0.3299404806269776169, 0.3333333333333333703, 0.3299404806269776169, 0.3333333333333333703, 0.3299404806269776169, 0.3333333333333333703, 0.3299404806269776169, 0.3333333333333333703, 0.3299404806269776169, 0.3333333333333333703, 0.3299404806269776169, 0.3333333333333333703, 0.3299404806269776169, 0.3333333333333333703, 0.3299404806269776169, 0.3333333333333333703, 0.3299404806269776169, 0.3333333333333333703, 0.3299404806269776169, 0.3333333333333333703, 0.3299404806269776169, 0.3333333333333333703, 0.3299404806269776169, 0.3333333333333333703, 0.3299404806269776169, 0.3333333333333333703, 0.3299404806269776169, 0.3333333333333333703, 0.3299404806269776169, 0.3333333333333333703, 0.3299404806269776169, 0.3333333333333333703, 0.3299404806269776169, 0.3333333333333333703, 0.3299404806269776169, 0.3333333333333333703, 0.3299404806269776169, 0.3333333333333333703, 0.3299404806269776169, 0.3333333333333333703, 0.3299404806269776169, 0.3333333333333333703, 0.3299404806269776169, 0.3333333333333333703, 0.3299404806269776169, 0.3333333333333333703, 0.3299404806269776169, 0.3333333333333333703, 0.3299404806269776169, 0.3333333333333333703, 0.3299404806269776169, 0.3333333333333333703, 0.3299404806269776169, 0.3333333333333333703, 0.3299404806269776169, 0.3333333333333333703, 0.3299404806269776169, 0.3333333333333333703, 0.3299404806269776169, 0.3333333333333333703, 0.3299404806269776169, 0.3333333333333333703, 0.3299404806269776169, 0.3333333333333333703, 0.3299404806269776169, 0.3333333333333333703, 0.3299404806269776169, 0.3333333333333333703, 0.3299404806269776169, 0.3333333333333333703, 0.3299404806269776169, 0.3333333333333333703, 0.3299404806269776169, 0.3333333333333333703, 0.3299404806269776169, 0.3333333333333333703, 0.3299404806269776169, 0.3333333333333333703, 0.3299404806269776169, 0.3333333333333333703, 0.3299404806269776169, 0.3333333333333333703, 0.3299404806269776169, 0.3333333333333333703, 0.3299404806269776169, 0.3333333333333333703, 0.3299404806269776169, 0.3333333333333333703, 0.3299404806269776169, 0.3333333333333333703, 0.3299404806269776169, 0.3333333333333333703, 0.3299404806269776169, 0.3333333333333333703, 0.3299404806269776169, 0.3333333333333333703, 0.3299404806269776169, 0.3333333333333333703, 0.3299404806269776169, 0.3333333333333333703, 0.3299404806269776169, 0.3333333333333333703, 0.3299404806269776169, 0.3333333333333333703, 0.3299404806269776169, 0.3333333333333333703, 0.3299404806269776169, 0.3333333333333333703, 0.3299404806269776169, 0.3333333333333333703, 0.3299404806269776169, 0.3333333333333333703, 0.3299404806269776169, 0.3333333333333333703, 0.3299404806269776169, 0.3333333333333333703, 0.3299404806269776169, 0.3333333333333333703, 0.3299404806269776169, 0.3333333333333333703, 0.3299404806269776169, 0.3333333333333333703, 0.3299404806269776169, 0.3333333333333333703, 0.3299404806269776169, 0.3333333333333333703, 0.3299404806269776169, 0.3333333333333333703, 0.3299404806269776169, 0.3333333333333333703, 0.3299404806269776169, 0.3333333333333333703, 0.3299404806269776169, 0.3333333333333333703, 0.3299404806269776169, 0.3333333333333333703, 0.3299404806269776169, 0.3333333333333333703, 0.3299404806269776169, 0.3333333333333333703, 0.3299404806269776169, 0.3333333333333333703, 0.3299404806269776169, 0.3333333333333333703, 0.3299404806269776169, 0.3333333333333333703, 0.3299404806269776169, 0.3333333333333333703, 0.3299404806269776169, 0.3333333333333333703, 0.3299404806269776169, 0.3333333333333333703, 0.3299404806269776169, 0.3333333333333333703, 0.3299404806269776169, 0.3333333333333333703, 0.3299404806269776169, 0.3333333333333333703, 0.3299404806269776169, 0.3333333333333333703, 0.3299404806269776169, 0.3333333333333333703, 0.3299404806269776169, 0.3333333333333333703, 0.3299404806269776169, 0.3333333333333333703, 0.3299404806269776169, 0.3333333333333333703, 0.3299404806269776169, 0.3333333333333333703, 0.3299404806269776169, 0.3333333333333333703, 0.3299404806269776169, 0.3333333333333333703, 0.3299404806269776169, 0.3333333333333333703, 0.3299404806269776169, 0.3333333333333333703, 0.3299404806269776169, 0.3333333333333333703, 0.3299404806269776169, 0.3333333333333333703, 0.3299404806269776169, 0.3333333333333333703, 0.3299404806269776169, 0.3333333333333333703, 0.3299404806269776169, 0.3333333333333333703, 0.3299404806269776169, 0.3333333333333333703, 0.3299404806269776169, 0.3333333333333333703, 0.3299404806269776169, 0.3333333333333333703, 0.3299404806269776169, 0.3333333333333333703, 0.3299404806269776169, 0.3333333333333333703, 0.3299404806269776169, 0.3333333333333333703, 0.3299404806269776169, 0.3333333333333333703, 0.3299404806269776169, 0.3333333333333333703, 0.3299404806269776169, 0.3333333333333333703, 0.3299404806269776169, 0.3333333333333333703, 0.3299404806269776169, 0.3333333333333333703, 0.3299404806269776169, 0.3333333333333333703, 0.3299404806269776169, 0.3333333333333333703, 0.3299404806269776169, 0.3333333333333333703, 0.3299404806269776169, 0.3333333333333333703, 0.3299404806269776169, 0.3333333333333333703, 0.3299404806269776169, 0.3333333333333333703, 0.3299404806269776169, 0.3333333333333333703, 0.3299404806269776169, 0.3333333333333333703, 0.3299404806269776169, 0.3333333333333333703, 0.3320603117974822438, 0.3317425830320511193),
 ( 0.3333333333333333703, 0.3299404806269776169, 0.3333333333333333703, 0.3299404806269776169, 0.3333333333333333703, 0.3299404806269776169, 0.3333333333333333703, 0.3299404806269776169, 0.3333333333333333703, 0.3299404806269776169, 0.3333333333333333703, 0.3299404806269776169, 0.3333333333333333703, 0.3299404806269776169, 0.3333333333333333703, 0.3299404806269776169, 0.3333333333333333703, 0.3299404806269776169, 0.3333333333333333703, 0.3299404806269776169, 0.3333333333333333703, 0.3299404806269776169, 0.3333333333333333703, 0.3299404806269776169, 0.3333333333333333703, 0.3299404806269776169, 0.3333333333333333703, 0.3299404806269776169, 0.3333333333333333703, 0.3299404806269776169, 0.3333333333333333703, 0.3299404806269776169, 0.3333333333333333703, 0.3299404806269776169, 0.3333333333333333703, 0.3299404806269776169, 0.3333333333333333703, 0.3299404806269776169, 0.3333333333333333703, 0.3299404806269776169, 0.3333333333333333703, 0.3299404806269776169, 0.3333333333333333703, 0.3299404806269776169, 0.3333333333333333703, 0.3299404806269776169, 0.3333333333333333703, 0.3299404806269776169, 0.3333333333333333703, 0.3299404806269776169, 0.3333333333333333703, 0.3299404806269776169, 0.3333333333333333703, 0.3299404806269776169, 0.3333333333333333703, 0.3299404806269776169, 0.3333333333333333703, 0.3299404806269776169, 0.3333333333333333703, 0.3299404806269776169, 0.3333333333333333703, 0.3299404806269776169, 0.3333333333333333703, 0.3299404806269776169, 0.3333333333333333703, 0.3299404806269776169, 0.3333333333333333703, 0.3299404806269776169, 0.3333333333333333703, 0.3299404806269776169, 0.3333333333333333703, 0.3299404806269776169, 0.3333333333333333703, 0.3299404806269776169, 0.3333333333333333703, 0.3299404806269776169, 0.3333333333333333703, 0.3299404806269776169, 0.3333333333333333703, 0.3299404806269776169, 0.3333333333333333703, 0.3299404806269776169, 0.3333333333333333703, 0.3299404806269776169, 0.3333333333333333703, 0.3299404806269776169, 0.3333333333333333703, 0.3299404806269776169, 0.3333333333333333703, 0.3299404806269776169, 0.3333333333333333703, 0.3299404806269776169, 0.3333333333333333703, 0.3299404806269776169, 0.3333333333333333703, 0.3299404806269776169, 0.3333333333333333703, 0.3299404806269776169, 0.3333333333333333703, 0.3299404806269776169, 0.3333333333333333703, 0.3299404806269776169, 0.3333333333333333703, 0.3299404806269776169, 0.3333333333333333703, 0.3299404806269776169, 0.3333333333333333703, 0.3299404806269776169, 0.3333333333333333703, 0.3299404806269776169, 0.3333333333333333703, 0.3299404806269776169, 0.3333333333333333703, 0.3299404806269776169, 0.3333333333333333703, 0.3299404806269776169, 0.3333333333333333703, 0.3299404806269776169, 0.3333333333333333703, 0.3299404806269776169, 0.3333333333333333703, 0.3299404806269776169, 0.3333333333333333703, 0.3299404806269776169, 0.3333333333333333703, 0.3299404806269776169, 0.3333333333333333703, 0.3299404806269776169, 0.3333333333333333703, 0.3299404806269776169, 0.3333333333333333703, 0.3299404806269776169, 0.3333333333333333703, 0.3299404806269776169, 0.3333333333333333703, 0.3299404806269776169, 0.3333333333333333703, 0.3299404806269776169, 0.3333333333333333703, 0.3299404806269776169, 0.3333333333333333703, 0.3299404806269776169, 0.3333333333333333703, 0.3299404806269776169, 0.3333333333333333703, 0.3299404806269776169, 0.3333333333333333703, 0.3299404806269776169, 0.3333333333333333703, 0.3299404806269776169, 0.3333333333333333703, 0.3299404806269776169, 0.3333333333333333703, 0.3299404806269776169, 0.3333333333333333703, 0.3299404806269776169, 0.3333333333333333703, 0.3299404806269776169, 0.3333333333333333703, 0.3299404806269776169, 0.3333333333333333703, 0.3299404806269776169, 0.3333333333333333703, 0.3299404806269776169, 0.3333333333333333703, 0.3299404806269776169, 0.3333333333333333703, 0.3299404806269776169, 0.3333333333333333703, 0.3299404806269776169, 0.3333333333333333703, 0.3299404806269776169, 0.3333333333333333703, 0.3299404806269776169, 0.3333333333333333703, 0.3299404806269776169, 0.3333333333333333703, 0.3299404806269776169, 0.3333333333333333703, 0.3299404806269776169, 0.3333333333333333703, 0.3299404806269776169, 0.3333333333333333703, 0.3299404806269776169, 0.3333333333333333703, 0.3299404806269776169, 0.3333333333333333703, 0.3299404806269776169, 0.3333333333333333703, 0.3299404806269776169, 0.3333333333333333703, 0.3299404806269776169, 0.3333333333333333703, 0.3299404806269776169, 0.3333333333333333703, 0.3299404806269776169, 0.3333333333333333703, 0.3299404806269776169, 0.3333333333333333703, 0.3299404806269776169, 0.3333333333333333703, 0.3299404806269776169, 0.3333333333333333703, 0.3299404806269776169, 0.3333333333333333703, 0.3299404806269776169, 0.3333333333333333703, 0.3299404806269776169, 0.3333333333333333703, 0.3299404806269776169, 0.3333333333333333703, 0.3299404806269776169, 0.3333333333333333703, 0.3299404806269776169, 0.3333333333333333703, 0.3299404806269776169, 0.3333333333333333703, 0.3299404806269776169, 0.3333333333333333703, 0.3299404806269776169, 0.3333333333333333703, 0.3299404806269776169, 0.3333333333333333703, 0.3299404806269776169, 0.3333333333333333703, 0.3299404806269776169, 0.3333333333333333703, 0.3299404806269776169, 0.3333333333333333703, 0.3299404806269776169, 0.3333333333333333703, 0.3299404806269776169, 0.3333333333333333703, 0.3299404806269776169, 0.3333333333333333703, 0.3299404806269776169, 0.3333333333333333703, 0.3299404806269776169, 0.3333333333333333703, 0.3299404806269776169, 0.3333333333333333703, 0.3299404806269776169, 0.3333333333333333703, 0.3299404806269776169, 0.3333333333333333703, 0.3299404806269776169, 0.3333333333333333703, 0.3299404806269776169, 0.3333333333333333703, 0.3299404806269776169, 0.3333333333333333703, 0.3299404806269776169, 0.3333333333333333703, 0.3299404806269776169, 0.3333333333333333703, 0.3299404806269776169, 0.3333333333333333703, 0.3299404806269776169, 0.3333333333333333703, 0.3299404806269776169, 0.3333333333333333703, 0.3299404806269776169, 0.3333333333333333703, 0.3299404806269776169, 0.3333333333333333703, 0.3299404806269776169, 0.3333333333333333703, 0.3299404806269776169, 0.3333333333333333703, 0.3299404806269776169, 0.3333333333333333703, 0.3299404806269776169, 0.3333333333333333703, 0.3299404806269776169, 0.3333333333333333703, 0.3299404806269776169, 0.3333333333333333703, 0.3299404806269776169, 0.3333333333333333703, 0.3299404806269776169, 0.3333333333333333703, 0.3299404806269776169, 0.3333333333333333703, 0.3299404806269776169, 0.3333333333333333703, 0.3299404806269776169, 0.3333333333333333703, 0.3299404806269776169, 0.3333333333333333703, 0.3299404806269776169, 0.3333333333333333703, 0.3299404806269776169, 0.3333333333333333703, 0.3299404806269776169, 0.3333333333333333703, 0.3299404806269776169, 0.3333333333333333703, 0.3299404806269776169, 0.3333333333333333703, 0.3299404806269776169, 0.3333333333333333703, 0.3299404806269776169, 0.3333333333333333703, 0.3299404806269776169, 0.3333333333333333703, 0.3299404806269776169, 0.3333333333333333703, 0.3299404806269776169, 0.3333333333333333703, 0.3299404806269776169, 0.3333333333333333703, 0.3299404806269776169, 0.3333333333333333703, 0.3299404806269776169, 0.3333333333333333703, 0.3299404806269776169, 0.3333333333333333703, 0.3299404806269776169, 0.3333333333333333703, 0.3299404806269776169, 0.3333333333333333703, 0.3299404806269776169, 0.3333333333333333703, 0.3299404806269776169, 0.3333333333333333703, 0.3299404806269776169, 0.3333333333333333703, 0.3299404806269776169, 0.3333333333333333703, 0.3299404806269776169, 0.3333333333333333703, 0.3299404806269776169, 0.3333333333333333703, 0.3299404806269776169, 0.3333333333333333703, 0.3299404806269776169, 0.3333333333333333703, 0.3299404806269776169, 0.3333333333333333703, 0.3299404806269776169, 0.3333333333333333703, 0.3299404806269776169, 0.3333333333333333703, 0.3299404806269776169, 0.3333333333333333703, 0.3299404806269776169, 0.3333333333333333703, 0.3299404806269776169, 0.3333333333333333703, 0.3299404806269776169, 0.3333333333333333703, 0.3299404806269776169, 0.3333333333333333703, 0.3299404806269776169, 0.3333333333333333703, 0.3299404806269776169, 0.3333333333333333703, 0.3299404806269776169, 0.3333333333333333703, 0.3299404806269776169, 0.3333333333333333703, 0.3299404806269776169, 0.3333333333333333703, 0.3299404806269776169, 0.3333333333333333703, 0.3299404806269776169, 0.3333333333333333703, 0.3299404806269776169, 0.3333333333333333703, 0.3299404806269776169, 0.3333333333333333703, 0.3299404806269776169, 0.3333333333333333703, 0.3299404806269776169, 0.3333333333333333703, 0.3299404806269776169, 0.3333333333333333703, 0.3299404806269776169, 0.3333333333333333703, 0.3299404806269776169, 0.3333333333333333703, 0.3299404806269776169, 0.3333333333333333703, 0.3299404806269776169, 0.3333333333333333703, 0.3299404806269776169, 0.3333333333333333703, 0.3299404806269776169, 0.3333333333333333703, 0.3299404806269776169, 0.3333333333333333703, 0.3299404806269776169, 0.3333333333333333703, 0.3299404806269776169, 0.3333333333333333703, 0.3299404806269776169, 0.3333333333333333703, 0.3299404806269776169, 0.3333333333333333703, 0.3299404806269776169, 0.3333333333333333703, 0.3299404806269776169, 0.3333333333333333703, 0.3299404806269776169, 0.3333333333333333703, 0.3299404806269776169, 0.3333333333333333703, 0.3299404806269776169, 0.3333333333333333703, 0.3299404806269776169, 0.3333333333333333703, 0.3299404806269776169, 0.3333333333333333703, 0.3299404806269776169, 0.3333333333333333703, 0.3299404806269776169, 0.3333333333333333703, 0.3299404806269776169, 0.3333333333333333703, 0.3299404806269776169, 0.3333333333333333703, 0.3299404806269776169, 0.3333333333333333703, 0.3299404806269776169, 0.3333333333333333703, 0.3299404806269776169, 0.3333333333333333703, 0.3299404806269776169, 0.3333333333333333703, 0.3299404806269776169, 0.3333333333333333703, 0.3299404806269776169, 0.3333333333333333703, 0.3299404806269776169, 0.3333333333333333703, 0.3299404806269776169, 0.3333333333333333703, 0.3299404806269776169, 0.3333333333333333703, 0.3299404806269776169, 0.3333333333333333703, 0.3299404806269776169, 0.3333333333333333703, 0.3299404806269776169, 0.3333333333333333703, 0.3299404806269776169, 0.3333333333333333703, 0.3299404806269776169, 0.3333333333333333703, 0.3299404806269776169, 0.3333333333333333703, 0.3299404806269776169, 0.3333333333333333703, 0.3299404806269776169, 0.3333333333333333703, 0.3299404806269776169, 0.3333333333333333703, 0.3299404806269776169, 0.3333333333333333703, 0.3299404806269776169, 0.3333333333333333703, 0.3299404806269776169, 0.3333333333333333703, 0.3299404806269776169, 0.3333333333333333703, 0.3299404806269776169, 0.3333333333333333703, 0.3299404806269776169, 0.3333333333333333703, 0.3299404806269776169, 0.3333333333333333703, 0.3299404806269776169, 0.3333333333333333703, 0.3299404806269776169, 0.3333333333333333703, 0.3299404806269776169, 0.3333333333333333703, 0.3299404806269776169, 0.3333333333333333703, 0.3299404806269776169, 0.3333333333333333703, 0.3299404806269776169, 0.3333333333333333703, 0.3299404806269776169, 0.3333333333333333703, 0.3299404806269776169, 0.3333333333333333703, 0.3299404806269776169, 0.3333333333333333703, 0.3299404806269776169, 0.3333333333333333703, 0.3299404806269776169, 0.3333333333333333703, 0.3299404806269776169, 0.3333333333333333703, 0.3299404806269776169, 0.3333333333333333703, 0.3299404806269776169, 0.3333333333333333703, 0.3299404806269776169, 0.3333333333333333703, 0.3299404806269776169, 0.3333333333333333703, 0.3299404806269776169, 0.3333333333333333703, 0.3299404806269776169, 0.3333333333333333703, 0.3299404806269776169, 0.3333333333333333703, 0.3299404806269776169, 0.3333333333333333703, 0.3299404806269776169, 0.3333333333333333703, 0.3299404806269776169, 0.3333333333333333703, 0.3299404806269776169, 0.3333333333333333703, 0.3299404806269776169, 0.3333333333333333703, 0.3299404806269776169, 0.3333333333333333703, 0.3299404806269776169, 0.3333333333333333703, 0.3299404806269776169, 0.3333333333333333703, 0.3299404806269776169, 0.3333333333333333703, 0.3299404806269776169, 0.3333333333333333703, 0.3299404806269776169, 0.3333333333333333703, 0.3299404806269776169, 0.3333333333333333703, 0.3299404806269776169, 0.3333333333333333703, 0.3299404806269776169, 0.3333333333333333703, 0.3299404806269776169, 0.3333333333333333703, 0.3299404806269776169, 0.3333333333333333703, 0.3299404806269776169, 0.3333333333333333703, 0.3299404806269776169, 0.3333333333333333703, 0.3299404806269776169, 0.3333333333333333703, 0.3299404806269776169, 0.3333333333333333703, 0.3299404806269776169, 0.3333333333333333703, 0.3299404806269776169, 0.3333333333333333703, 0.3299404806269776169, 0.3333333333333333703, 0.3299404806269776169, 0.3333333333333333703, 0.3299404806269776169, 0.3333333333333333703, 0.3299404806269776169, 0.3333333333333333703, 0.3299404806269776169, 0.3333333333333333703, 0.3299404806269776169, 0.3333333333333333703, 0.3299404806269776169, 0.3333333333333333703, 0.3299404806269776169, 0.3333333333333333703, 0.3299404806269776169, 0.3333333333333333703, 0.3299404806269776169, 0.3333333333333333703, 0.3299404806269776169, 0.3333333333333333703, 0.3299404806269776169, 0.3333333333333333703, 0.3299404806269776169, 0.3333333333333333703, 0.3299404806269776169, 0.3333333333333333703, 0.3299404806269776169, 0.3333333333333333703, 0.3299404806269776169, 0.3333333333333333703, 0.3299404806269776169, 0.3333333333333333703, 0.3299404806269776169, 0.3333333333333333703, 0.3299404806269776169, 0.3333333333333333703, 0.3299404806269776169, 0.3333333333333333703, 0.3299404806269776169, 0.3333333333333333703, 0.3299404806269776169, 0.3333333333333333703, 0.3299404806269776169, 0.3333333333333333703, 0.3299404806269776169, 0.3333333333333333703, 0.3299404806269776169, 0.3333333333333333703, 0.3299404806269776169, 0.3333333333333333703, 0.3299404806269776169, 0.3333333333333333703, 0.3299404806269776169, 0.3333333333333333703, 0.3299404806269776169, 0.3333333333333333703, 0.3299404806269776169, 0.3333333333333333703, 0.3299404806269776169, 0.3333333333333333703, 0.3299404806269776169, 0.3333333333333333703, 0.3299404806269776169, 0.3333333333333333703, 0.3299404806269776169, 0.3333333333333333703, 0.3299404806269776169, 0.3333333333333333703, 0.3299404806269776169, 0.3333333333333333703, 0.3299404806269776169, 0.3333333333333333703, 0.3299404806269776169, 0.3333333333333333703, 0.3299404806269776169, 0.3333333333333333703, 0.3299404806269776169, 0.3333333333333333703, 0.3299404806269776169, 0.3333333333333333703, 0.3299404806269776169, 0.3333333333333333703, 0.3299404806269776169, 0.3333333333333333703, 0.3299404806269776169, 0.3333333333333333703, 0.3299404806269776169, 0.3333333333333333703, 0.3299404806269776169, 0.3333333333333333703, 0.3299404806269776169, 0.3333333333333333703, 0.3299404806269776169, 0.3333333333333333703, 0.3299404806269776169, 0.3333333333333333703, 0.3299404806269776169, 0.3333333333333333703, 0.3299404806269776169, 0.3333333333333333703, 0.3299404806269776169, 0.3333333333333333703, 0.3299404806269776169, 0.3333333333333333703, 0.3299404806269776169, 0.3333333333333333703, 0.3299404806269776169, 0.3333333333333333703, 0.3299404806269776169, 0.3333333333333333703, 0.3299404806269776169, 0.3333333333333333703, 0.3299404806269776169, 0.3333333333333333703, 0.3299404806269776169, 0.3333333333333333703, 0.3299404806269776169, 0.3333333333333333703, 0.3299404806269776169, 0.3333333333333333703, 0.3299404806269776169, 0.3333333333333333703, 0.3299404806269776169, 0.3333333333333333703, 0.3299404806269776169, 0.3333333333333333703, 0.3299404806269776169, 0.3333333333333333703, 0.3299404806269776169, 0.3333333333333333703, 0.3299404806269776169, 0.3333333333333333703, 0.3299404806269776169, 0.3333333333333333703, 0.3299404806269776169, 0.3333333333333333703, 0.3299404806269776169, 0.3333333333333333703, 0.3299404806269776169, 0.3333333333333333703, 0.3299404806269776169, 0.3333333333333333703, 0.3299404806269776169, 0.3333333333333333703, 0.3299404806269776169, 0.3333333333333333703, 0.3299404806269776169, 0.3333333333333333703, 0.3299404806269776169, 0.3333333333333333703, 0.3299404806269776169, 0.3333333333333333703, 0.3299404806269776169, 0.3333333333333333703, 0.3299404806269776169, 0.3333333333333333703, 0.3299404806269776169, 0.3333333333333333703, 0.3299404806269776169, 0.3333333333333333703, 0.3299404806269776169, 0.3333333333333333703, 0.3299404806269776169, 0.3333333333333333703, 0.3299404806269776169, 0.3333333333333333703, 0.3299404806269776169, 0.3333333333333333703, 0.3299404806269776169, 0.3333333333333333703, 0.3299404806269776169, 0.3333333333333333703, 0.3299404806269776169, 0.3333333333333333703, 0.3299404806269776169, 0.3333333333333333703, 0.3299404806269776169, 0.3333333333333333703, 0.3299404806269776169, 0.3333333333333333703, 0.3299404806269776169, 0.3333333333333333703, 0.3299404806269776169, 0.3333333333333333703, 0.3299404806269776169, 0.3333333333333333703, 0.3299404806269776169, 0.3333333333333333703, 0.3299404806269776169, 0.3333333333333333703, 0.3299404806269776169, 0.3333333333333333703, 0.3299404806269776169, 0.3333333333333333703, 0.3299404806269776169, 0.3333333333333333703, 0.3299404806269776169, 0.3333333333333333703, 0.3299404806269776169, 0.3333333333333333703, 0.3299404806269776169, 0.3333333333333333703, 0.3299404806269776169, 0.3333333333333333703, 0.3299404806269776169, 0.3333333333333333703, 0.3299404806269776169, 0.3333333333333333703, 0.3299404806269776169, 0.3333333333333333703, 0.3299404806269776169, 0.3333333333333333703, 0.3299404806269776169, 0.3333333333333333703, 0.3299404806269776169, 0.3333333333333333703, 0.3299404806269776169, 0.3333333333333333703, 0.3299404806269776169, 0.3333333333333333703, 0.3299404806269776169, 0.3333333333333333703, 0.3299404806269776169, 0.3333333333333333703, 0.3299404806269776169, 0.3333333333333333703, 0.3299404806269776169, 0.3333333333333333703, 0.3299404806269776169, 0.3333333333333333703, 0.3299404806269776169, 0.3333333333333333703, 0.3299404806269776169, 0.3333333333333333703, 0.3299404806269776169, 0.3333333333333333703, 0.3299404806269776169, 0.3333333333333333703, 0.3299404806269776169, 0.3333333333333333703, 0.3299404806269776169, 0.3333333333333333703, 0.3299404806269776169, 0.3333333333333333703, 0.3299404806269776169, 0.3333333333333333703, 0.3299404806269776169, 0.3333333333333333703, 0.3299404806269776169, 0.3333333333333333703, 0.3299404806269776169, 0.3333333333333333703, 0.3299404806269776169, 0.3333333333333333703, 0.3299404806269776169, 0.3333333333333333703, 0.3299404806269776169, 0.3333333333333333703, 0.3299404806269776169, 0.3333333333333333703, 0.3299404806269776169, 0.3333333333333333703, 0.3299404806269776169, 0.3333333333333333703, 0.3299404806269776169, 0.3333333333333333703, 0.3299404806269776169, 0.3333333333333333703, 0.3299404806269776169, 0.3333333333333333703, 0.3299404806269776169, 0.3333333333333333703, 0.3299404806269776169, 0.3333333333333333703, 0.3299404806269776169, 0.3333333333333333703, 0.3299404806269776169, 0.3333333333333333703, 0.3299404806269776169, 0.3333333333333333703, 0.3299404806269776169, 0.3333333333333333703, 0.3299404806269776169, 0.3333333333333333703, 0.3299404806269776169, 0.3333333333333333703, 0.3299404806269776169, 0.3333333333333333703, 0.3299404806269776169, 0.3333333333333333703, 0.3299404806269776169, 0.3333333333333333703, 0.3299404806269776169, 0.3333333333333333703, 0.3299404806269776169, 0.3333333333333333703, 0.3299404806269776169, 0.3333333333333333703, 0.3299404806269776169, 0.3333333333333333703, 0.3299404806269776169, 0.3333333333333333703, 0.3299404806269776169, 0.3333333333333333703, 0.3299404806269776169, 0.3333333333333333703, 0.3320603117974822438, 0.3317425830320511193),
 ( 1.000000000000000000, 0.9898214418809326842, 1.000000000000000000, 0.9898214418809326842, 1.000000000000000000, 0.9898214418809326842, 1.000000000000000000, 0.9898214418809326842, 1.000000000000000000, 0.9898214418809326842, 1.000000000000000000, 0.9898214418809326842, 1.000000000000000000, 0.9898214418809326842, 1.000000000000000000, 0.9898214418809326842, 1.000000000000000000, 0.9898214418809326842, 1.000000000000000000, 0.9898214418809326842, 1.000000000000000000, 0.9898214418809326842, 1.000000000000000000, 0.9898214418809326842, 1.000000000000000000, 0.9898214418809326842, 1.000000000000000000, 0.9898214418809326842, 1.000000000000000000, 0.9898214418809326842, 1.000000000000000000, 0.9898214418809326842, 1.000000000000000000, 0.9898214418809326842, 1.000000000000000000, 0.9898214418809326842, 1.000000000000000000, 0.9898214418809326842, 1.000000000000000000, 0.9898214418809326842, 1.000000000000000000, 0.9898214418809326842, 1.000000000000000000, 0.9898214418809326842, 1.000000000000000000, 0.9898214418809326842, 1.000000000000000000, 0.9898214418809326842, 1.000000000000000000, 0.9898214418809326842, 1.000000000000000000, 0.9898214418809326842, 1.000000000000000000, 0.9898214418809326842, 1.000000000000000000, 0.9898214418809326842, 1.000000000000000000, 0.9898214418809326842, 1.000000000000000000, 0.9898214418809326842, 1.000000000000000000, 0.9898214418809326842, 1.000000000000000000, 0.9898214418809326842, 1.000000000000000000, 0.9898214418809326842, 1.000000000000000000, 0.9898214418809326842, 1.000000000000000000, 0.9898214418809326842, 1.000000000000000000, 0.9898214418809326842, 1.000000000000000000, 0.9898214418809326842, 1.000000000000000000, 0.9898214418809326842, 1.000000000000000000, 0.9898214418809326842, 1.000000000000000000, 0.9898214418809326842, 1.000000000000000000, 0.9898214418809326842, 1.000000000000000000, 0.9898214418809326842, 1.000000000000000000, 0.9898214418809326842, 1.000000000000000000, 0.9898214418809326842, 1.000000000000000000, 0.9898214418809326842, 1.000000000000000000, 0.9898214418809326842, 1.000000000000000000, 0.9898214418809326842, 1.000000000000000000, 0.9898214418809326842, 1.000000000000000000, 0.9898214418809326842, 1.000000000000000000, 0.9898214418809326842, 1.000000000000000000, 0.9898214418809326842, 1.000000000000000000, 0.9898214418809326842, 1.000000000000000000, 0.9898214418809326842, 1.000000000000000000, 0.9898214418809326842, 1.000000000000000000, 0.9898214418809326842, 1.000000000000000000, 0.9898214418809326842, 1.000000000000000000, 0.9898214418809326842, 1.000000000000000000, 0.9898214418809326842, 1.000000000000000000, 0.9898214418809326842, 1.000000000000000000, 0.9898214418809326842, 1.000000000000000000, 0.9898214418809326842, 1.000000000000000000, 0.9898214418809326842, 1.000000000000000000, 0.9898214418809326842, 1.000000000000000000, 0.9898214418809326842, 1.000000000000000000, 0.9898214418809326842, 1.000000000000000000, 0.9898214418809326842, 1.000000000000000000, 0.9898214418809326842, 1.000000000000000000, 0.9898214418809326842, 1.000000000000000000, 0.9898214418809326842, 1.000000000000000000, 0.9898214418809326842, 1.000000000000000000, 0.9898214418809326842, 1.000000000000000000, 0.9898214418809326842, 1.000000000000000000, 0.9898214418809326842, 1.000000000000000000, 0.9898214418809326842, 1.000000000000000000, 0.9898214418809326842, 1.000000000000000000, 0.9898214418809326842, 1.000000000000000000, 0.9898214418809326842, 1.000000000000000000, 0.9898214418809326842, 1.000000000000000000, 0.9898214418809326842, 1.000000000000000000, 0.9898214418809326842, 1.000000000000000000, 0.9898214418809326842, 1.000000000000000000, 0.9898214418809326842, 1.000000000000000000, 0.9898214418809326842, 1.000000000000000000, 0.9898214418809326842, 1.000000000000000000, 0.9898214418809326842, 1.000000000000000000, 0.9898214418809326842, 1.000000000000000000, 0.9898214418809326842, 1.000000000000000000, 0.9898214418809326842, 1.000000000000000000, 0.9898214418809326842, 1.000000000000000000, 0.9898214418809326842, 1.000000000000000000, 0.9898214418809326842, 1.000000000000000000, 0.9898214418809326842, 1.000000000000000000, 0.9898214418809326842, 1.000000000000000000, 0.9898214418809326842, 1.000000000000000000, 0.9898214418809326842, 1.000000000000000000, 0.9898214418809326842, 1.000000000000000000, 0.9898214418809326842, 1.000000000000000000, 0.9898214418809326842, 1.000000000000000000, 0.9898214418809326842, 1.000000000000000000, 0.9898214418809326842, 1.000000000000000000, 0.9898214418809326842, 1.000000000000000000, 0.9898214418809326842, 1.000000000000000000, 0.9898214418809326842, 1.000000000000000000, 0.9898214418809326842, 1.000000000000000000, 0.9898214418809326842, 1.000000000000000000, 0.9898214418809326842, 1.000000000000000000, 0.9898214418809326842, 1.000000000000000000, 0.9898214418809326842, 1.000000000000000000, 0.9898214418809326842, 1.000000000000000000, 0.9898214418809326842, 1.000000000000000000, 0.9898214418809326842, 1.000000000000000000, 0.9898214418809326842, 1.000000000000000000, 0.9898214418809326842, 1.000000000000000000, 0.9898214418809326842, 1.000000000000000000, 0.9898214418809326842, 1.000000000000000000, 0.9898214418809326842, 1.000000000000000000, 0.9898214418809326842, 1.000000000000000000, 0.9898214418809326842, 1.000000000000000000, 0.9898214418809326842, 1.000000000000000000, 0.9898214418809326842, 1.000000000000000000, 0.9898214418809326842, 1.000000000000000000, 0.9898214418809326842, 1.000000000000000000, 0.9898214418809326842, 1.000000000000000000, 0.9898214418809326842, 1.000000000000000000, 0.9898214418809326842, 1.000000000000000000, 0.9898214418809326842, 1.000000000000000000, 0.9898214418809326842, 1.000000000000000000, 0.9898214418809326842, 1.000000000000000000, 0.9898214418809326842, 1.000000000000000000, 0.9898214418809326842, 1.000000000000000000, 0.9898214418809326842, 1.000000000000000000, 0.9898214418809326842, 1.000000000000000000, 0.9898214418809326842, 1.000000000000000000, 0.9898214418809326842, 1.000000000000000000, 0.9898214418809326842, 1.000000000000000000, 0.9898214418809326842, 1.000000000000000000, 0.9898214418809326842, 1.000000000000000000, 0.9898214418809326842, 1.000000000000000000, 0.9898214418809326842, 1.000000000000000000, 0.9898214418809326842, 1.000000000000000000, 0.9898214418809326842, 1.000000000000000000, 0.9898214418809326842, 1.000000000000000000, 0.9898214418809326842, 1.000000000000000000, 0.9898214418809326842, 1.000000000000000000, 0.9898214418809326842, 1.000000000000000000, 0.9898214418809326842, 1.000000000000000000, 0.9898214418809326842, 1.000000000000000000, 0.9898214418809326842, 1.000000000000000000, 0.9898214418809326842, 1.000000000000000000, 0.9898214418809326842, 1.000000000000000000, 0.9898214418809326842, 1.000000000000000000, 0.9898214418809326842, 1.000000000000000000, 0.9898214418809326842, 1.000000000000000000, 0.9898214418809326842, 1.000000000000000000, 0.9898214418809326842, 1.000000000000000000, 0.9898214418809326842, 1.000000000000000000, 0.9898214418809326842, 1.000000000000000000, 0.9898214418809326842, 1.000000000000000000, 0.9898214418809326842, 1.000000000000000000, 0.9898214418809326842, 1.000000000000000000, 0.9898214418809326842, 1.000000000000000000, 0.9898214418809326842, 1.000000000000000000, 0.9898214418809326842, 1.000000000000000000, 0.9898214418809326842, 1.000000000000000000, 0.9898214418809326842, 1.000000000000000000, 0.9898214418809326842, 1.000000000000000000, 0.9898214418809326842, 1.000000000000000000, 0.9898214418809326842, 1.000000000000000000, 0.9898214418809326842, 1.000000000000000000, 0.9898214418809326842, 1.000000000000000000, 0.9898214418809326842, 1.000000000000000000, 0.9898214418809326842, 1.000000000000000000, 0.9898214418809326842, 1.000000000000000000, 0.9898214418809326842, 1.000000000000000000, 0.9898214418809326842, 1.000000000000000000, 0.9898214418809326842, 1.000000000000000000, 0.9898214418809326842, 1.000000000000000000, 0.9898214418809326842, 1.000000000000000000, 0.9898214418809326842, 1.000000000000000000, 0.9898214418809326842, 1.000000000000000000, 0.9898214418809326842, 1.000000000000000000, 0.9898214418809326842, 1.000000000000000000, 0.9898214418809326842, 1.000000000000000000, 0.9898214418809326842, 1.000000000000000000, 0.9898214418809326842, 1.000000000000000000, 0.9898214418809326842, 1.000000000000000000, 0.9898214418809326842, 1.000000000000000000, 0.9898214418809326842, 1.000000000000000000, 0.9898214418809326842, 1.000000000000000000, 0.9898214418809326842, 1.000000000000000000, 0.9898214418809326842, 1.000000000000000000, 0.9898214418809326842, 1.000000000000000000, 0.9898214418809326842, 1.000000000000000000, 0.9898214418809326842, 1.000000000000000000, 0.9898214418809326842, 1.000000000000000000, 0.9898214418809326842, 1.000000000000000000, 0.9898214418809326842, 1.000000000000000000, 0.9898214418809326842, 1.000000000000000000, 0.9898214418809326842, 1.000000000000000000, 0.9898214418809326842, 1.000000000000000000, 0.9898214418809326842, 1.000000000000000000, 0.9898214418809326842, 1.000000000000000000, 0.9898214418809326842, 1.000000000000000000, 0.9898214418809326842, 1.000000000000000000, 0.9898214418809326842, 1.000000000000000000, 0.9898214418809326842, 1.000000000000000000, 0.9898214418809326842, 1.000000000000000000, 0.9898214418809326842, 1.000000000000000000, 0.9898214418809326842, 1.000000000000000000, 0.9898214418809326842, 1.000000000000000000, 0.9898214418809326842, 1.000000000000000000, 0.9898214418809326842, 1.000000000000000000, 0.9898214418809326842, 1.000000000000000000, 0.9898214418809326842, 1.000000000000000000, 0.9898214418809326842, 1.000000000000000000, 0.9898214418809326842, 1.000000000000000000, 0.9898214418809326842, 1.000000000000000000, 0.9898214418809326842, 1.000000000000000000, 0.9898214418809326842, 1.000000000000000000, 0.9898214418809326842, 1.000000000000000000, 0.9898214418809326842, 1.000000000000000000, 0.9898214418809326842, 1.000000000000000000, 0.9898214418809326842, 1.000000000000000000, 0.9898214418809326842, 1.000000000000000000, 0.9898214418809326842, 1.000000000000000000, 0.9898214418809326842, 1.000000000000000000, 0.9898214418809326842, 1.000000000000000000, 0.9898214418809326842, 1.000000000000000000, 0.9898214418809326842, 1.000000000000000000, 0.9898214418809326842, 1.000000000000000000, 0.9898214418809326842, 1.000000000000000000, 0.9898214418809326842, 1.000000000000000000, 0.9898214418809326842, 1.000000000000000000, 0.9898214418809326842, 1.000000000000000000, 0.9898214418809326842, 1.000000000000000000, 0.9898214418809326842, 1.000000000000000000, 0.9898214418809326842, 1.000000000000000000, 0.9898214418809326842, 1.000000000000000000, 0.9898214418809326842, 1.000000000000000000, 0.9898214418809326842, 1.000000000000000000, 0.9898214418809326842, 1.000000000000000000, 0.9898214418809326842, 1.000000000000000000, 0.9898214418809326842, 1.000000000000000000, 0.9898214418809326842, 1.000000000000000000, 0.9898214418809326842, 1.000000000000000000, 0.9898214418809326842, 1.000000000000000000, 0.9898214418809326842, 1.000000000000000000, 0.9898214418809326842, 1.000000000000000000, 0.9898214418809326842, 1.000000000000000000, 0.9898214418809326842, 1.000000000000000000, 0.9898214418809326842, 1.000000000000000000, 0.9898214418809326842, 1.000000000000000000, 0.9898214418809326842, 1.000000000000000000, 0.9898214418809326842, 1.000000000000000000, 0.9898214418809326842, 1.000000000000000000, 0.9898214418809326842, 1.000000000000000000, 0.9898214418809326842, 1.000000000000000000, 0.9898214418809326842, 1.000000000000000000, 0.9898214418809326842, 1.000000000000000000, 0.9898214418809326842, 1.000000000000000000, 0.9898214418809326842, 1.000000000000000000, 0.9898214418809326842, 1.000000000000000000, 0.9898214418809326842, 1.000000000000000000, 0.9898214418809326842, 1.000000000000000000, 0.9898214418809326842, 1.000000000000000000, 0.9898214418809326842, 1.000000000000000000, 0.9898214418809326842, 1.000000000000000000, 0.9898214418809326842, 1.000000000000000000, 0.9898214418809326842, 1.000000000000000000, 0.9898214418809326842, 1.000000000000000000, 0.9898214418809326842, 1.000000000000000000, 0.9898214418809326842, 1.000000000000000000, 0.9898214418809326842, 1.000000000000000000, 0.9898214418809326842, 1.000000000000000000, 0.9898214418809326842, 1.000000000000000000, 0.9898214418809326842, 1.000000000000000000, 0.9898214418809326842, 1.000000000000000000, 0.9898214418809326842, 1.000000000000000000, 0.9898214418809326842, 1.000000000000000000, 0.9898214418809326842, 1.000000000000000000, 0.9898214418809326842, 1.000000000000000000, 0.9898214418809326842, 1.000000000000000000, 0.9898214418809326842, 1.000000000000000000, 0.9898214418809326842, 1.000000000000000000, 0.9898214418809326842, 1.000000000000000000, 0.9898214418809326842, 1.000000000000000000, 0.9898214418809326842, 1.000000000000000000, 0.9898214418809326842, 1.000000000000000000, 0.9898214418809326842, 1.000000000000000000, 0.9898214418809326842, 1.000000000000000000, 0.9898214418809326842, 1.000000000000000000, 0.9898214418809326842, 1.000000000000000000, 0.9898214418809326842, 1.000000000000000000, 0.9898214418809326842, 1.000000000000000000, 0.9898214418809326842, 1.000000000000000000, 0.9898214418809326842, 1.000000000000000000, 0.9898214418809326842, 1.000000000000000000, 0.9898214418809326842, 1.000000000000000000, 0.9898214418809326842, 1.000000000000000000, 0.9898214418809326842, 1.000000000000000000, 0.9898214418809326842, 1.000000000000000000, 0.9898214418809326842, 1.000000000000000000, 0.9898214418809326842, 1.000000000000000000, 0.9898214418809326842, 1.000000000000000000, 0.9898214418809326842, 1.000000000000000000, 0.9898214418809326842, 1.000000000000000000, 0.9898214418809326842, 1.000000000000000000, 0.9898214418809326842, 1.000000000000000000, 0.9898214418809326842, 1.000000000000000000, 0.9898214418809326842, 1.000000000000000000, 0.9898214418809326842, 1.000000000000000000, 0.9898214418809326842, 1.000000000000000000, 0.9898214418809326842, 1.000000000000000000, 0.9898214418809326842, 1.000000000000000000, 0.9898214418809326842, 1.000000000000000000, 0.9898214418809326842, 1.000000000000000000, 0.9898214418809326842, 1.000000000000000000, 0.9898214418809326842, 1.000000000000000000, 0.9898214418809326842, 1.000000000000000000, 0.9898214418809326842, 1.000000000000000000, 0.9898214418809326842, 1.000000000000000000, 0.9898214418809326842, 1.000000000000000000, 0.9898214418809326842, 1.000000000000000000, 0.9898214418809326842, 1.000000000000000000, 0.9898214418809326842, 1.000000000000000000, 0.9898214418809326842, 1.000000000000000000, 0.9898214418809326842, 1.000000000000000000, 0.9898214418809326842, 1.000000000000000000, 0.9898214418809326842, 1.000000000000000000, 0.9898214418809326842, 1.000000000000000000, 0.9898214418809326842, 1.000000000000000000, 0.9898214418809326842, 1.000000000000000000, 0.9898214418809326842, 1.000000000000000000, 0.9898214418809326842, 1.000000000000000000, 0.9898214418809326842, 1.000000000000000000, 0.9898214418809326842, 1.000000000000000000, 0.9898214418809326842, 1.000000000000000000, 0.9898214418809326842, 1.000000000000000000, 0.9898214418809326842, 1.000000000000000000, 0.9898214418809326842, 1.000000000000000000, 0.9898214418809326842, 1.000000000000000000, 0.9898214418809326842, 1.000000000000000000, 0.9898214418809326842, 1.000000000000000000, 0.9898214418809326842, 1.000000000000000000, 0.9898214418809326842, 1.000000000000000000, 0.9898214418809326842, 1.000000000000000000, 0.9898214418809326842, 1.000000000000000000, 0.9898214418809326842, 1.000000000000000000, 0.9898214418809326842, 1.000000000000000000, 0.9898214418809326842, 1.000000000000000000, 0.9898214418809326842, 1.000000000000000000, 0.9898214418809326842, 1.000000000000000000, 0.9898214418809326842, 1.000000000000000000, 0.9898214418809326842, 1.000000000000000000, 0.9898214418809326842, 1.000000000000000000, 0.9898214418809326842, 1.000000000000000000, 0.9898214418809326842, 1.000000000000000000, 0.9898214418809326842, 1.000000000000000000, 0.9898214418809326842, 1.000000000000000000, 0.9898214418809326842, 1.000000000000000000, 0.9898214418809326842, 1.000000000000000000, 0.9898214418809326842, 1.000000000000000000, 0.9898214418809326842, 1.000000000000000000, 0.9898214418809326842, 1.000000000000000000, 0.9898214418809326842, 1.000000000000000000, 0.9898214418809326842, 1.000000000000000000, 0.9898214418809326842, 1.000000000000000000, 0.9898214418809326842, 1.000000000000000000, 0.9898214418809326842, 1.000000000000000000, 0.9898214418809326842, 1.000000000000000000, 0.9898214418809326842, 1.000000000000000000, 0.9898214418809326842, 1.000000000000000000, 0.9898214418809326842, 1.000000000000000000, 0.9898214418809326842, 1.000000000000000000, 0.9898214418809326842, 1.000000000000000000, 0.9898214418809326842, 1.000000000000000000, 0.9898214418809326842, 1.000000000000000000, 0.9898214418809326842, 1.000000000000000000, 0.9898214418809326842, 1.000000000000000000, 0.9898214418809326842, 1.000000000000000000, 0.9898214418809326842, 1.000000000000000000, 0.9898214418809326842, 1.000000000000000000, 0.9898214418809326842, 1.000000000000000000, 0.9898214418809326842, 1.000000000000000000, 0.9898214418809326842, 1.000000000000000000, 0.9898214418809326842, 1.000000000000000000, 0.9898214418809326842, 1.000000000000000000, 0.9898214418809326842, 1.000000000000000000, 0.9898214418809326842, 1.000000000000000000, 0.9898214418809326842, 1.000000000000000000, 0.9898214418809326842, 1.000000000000000000, 0.9898214418809326842, 1.000000000000000000, 0.9898214418809326842, 1.000000000000000000, 0.9898214418809326842, 1.000000000000000000, 0.9898214418809326842, 1.000000000000000000, 0.9898214418809326842, 1.000000000000000000, 0.9898214418809326842, 1.000000000000000000, 0.9898214418809326842, 1.000000000000000000, 0.9898214418809326842, 1.000000000000000000, 0.9898214418809326842, 1.000000000000000000, 0.9898214418809326842, 1.000000000000000000, 0.9898214418809326842, 1.000000000000000000, 0.9898214418809326842, 1.000000000000000000, 0.9898214418809326842, 1.000000000000000000, 0.9898214418809326842, 1.000000000000000000, 0.9898214418809326842, 1.000000000000000000, 0.9898214418809326842, 1.000000000000000000, 0.9898214418809326842, 1.000000000000000000, 0.9898214418809326842, 1.000000000000000000, 0.9898214418809326842, 1.000000000000000000, 0.9898214418809326842, 1.000000000000000000, 0.9898214418809326842, 1.000000000000000000, 0.9898214418809326842, 1.000000000000000000, 0.9898214418809326842, 1.000000000000000000, 0.9898214418809326842, 1.000000000000000000, 0.9898214418809326842, 1.000000000000000000, 0.9898214418809326842, 1.000000000000000000, 0.9898214418809326842, 1.000000000000000000, 0.9898214418809326842, 1.000000000000000000, 0.9898214418809326842, 1.000000000000000000, 0.9898214418809326842, 1.000000000000000000, 0.9898214418809326842, 1.000000000000000000, 0.9898214418809326842, 1.000000000000000000, 0.9898214418809326842, 1.000000000000000000, 0.9898214418809326842, 1.000000000000000000, 0.9898214418809326842, 1.000000000000000000, 0.9898214418809326842, 1.000000000000000000, 0.9898214418809326842, 1.000000000000000000, 0.9898214418809326842, 1.000000000000000000, 0.9898214418809326842, 1.000000000000000000, 0.9961809353924466759, 0.9952277490961531914),
 ( 0.3333333333333333703, 0.3299404806269776169, 0.3333333333333333703, 0.3299404806269776169, 0.3333333333333333703, 0.3299404806269776169, 0.3333333333333333703, 0.3299404806269776169, 0.3333333333333333703, 0.3299404806269776169, 0.3333333333333333703, 0.3299404806269776169, 0.3333333333333333703, 0.3299404806269776169, 0.3333333333333333703, 0.3299404806269776169, 0.3333333333333333703, 0.3299404806269776169, 0.3333333333333333703, 0.3299404806269776169, 0.3333333333333333703, 0.3299404806269776169, 0.3333333333333333703, 0.3299404806269776169, 0.3333333333333333703, 0.3299404806269776169, 0.3333333333333333703, 0.3299404806269776169, 0.3333333333333333703, 0.3299404806269776169, 0.3333333333333333703, 0.3299404806269776169, 0.3333333333333333703, 0.3299404806269776169, 0.3333333333333333703, 0.3299404806269776169, 0.3333333333333333703, 0.3299404806269776169, 0.3333333333333333703, 0.3299404806269776169, 0.3333333333333333703, 0.3299404806269776169, 0.3333333333333333703, 0.3299404806269776169, 0.3333333333333333703, 0.3299404806269776169, 0.3333333333333333703, 0.3299404806269776169, 0.3333333333333333703, 0.3299404806269776169, 0.3333333333333333703, 0.3299404806269776169, 0.3333333333333333703, 0.3299404806269776169, 0.3333333333333333703, 0.3299404806269776169, 0.3333333333333333703, 0.3299404806269776169, 0.3333333333333333703, 0.3299404806269776169, 0.3333333333333333703, 0.3299404806269776169, 0.3333333333333333703, 0.3299404806269776169, 0.3333333333333333703, 0.3299404806269776169, 0.3333333333333333703, 0.3299404806269776169, 0.3333333333333333703, 0.3299404806269776169, 0.3333333333333333703, 0.3299404806269776169, 0.3333333333333333703, 0.3299404806269776169, 0.3333333333333333703, 0.3299404806269776169, 0.3333333333333333703, 0.3299404806269776169, 0.3333333333333333703, 0.3299404806269776169, 0.3333333333333333703, 0.3299404806269776169, 0.3333333333333333703, 0.3299404806269776169, 0.3333333333333333703, 0.3299404806269776169, 0.3333333333333333703, 0.3299404806269776169, 0.3333333333333333703, 0.3299404806269776169, 0.3333333333333333703, 0.3299404806269776169, 0.3333333333333333703, 0.3299404806269776169, 0.3333333333333333703, 0.3299404806269776169, 0.3333333333333333703, 0.3299404806269776169, 0.3333333333333333703, 0.3299404806269776169, 0.3333333333333333703, 0.3299404806269776169, 0.3333333333333333703, 0.3299404806269776169, 0.3333333333333333703, 0.3299404806269776169, 0.3333333333333333703, 0.3299404806269776169, 0.3333333333333333703, 0.3299404806269776169, 0.3333333333333333703, 0.3299404806269776169, 0.3333333333333333703, 0.3299404806269776169, 0.3333333333333333703, 0.3299404806269776169, 0.3333333333333333703, 0.3299404806269776169, 0.3333333333333333703, 0.3299404806269776169, 0.3333333333333333703, 0.3299404806269776169, 0.3333333333333333703, 0.3299404806269776169, 0.3333333333333333703, 0.3299404806269776169, 0.3333333333333333703, 0.3299404806269776169, 0.3333333333333333703, 0.3299404806269776169, 0.3333333333333333703, 0.3299404806269776169, 0.3333333333333333703, 0.3299404806269776169, 0.3333333333333333703, 0.3299404806269776169, 0.3333333333333333703, 0.3299404806269776169, 0.3333333333333333703, 0.3299404806269776169, 0.3333333333333333703, 0.3299404806269776169, 0.3333333333333333703, 0.3299404806269776169, 0.3333333333333333703, 0.3299404806269776169, 0.3333333333333333703, 0.3299404806269776169, 0.3333333333333333703, 0.3299404806269776169, 0.3333333333333333703, 0.3299404806269776169, 0.3333333333333333703, 0.3299404806269776169, 0.3333333333333333703, 0.3299404806269776169, 0.3333333333333333703, 0.3299404806269776169, 0.3333333333333333703, 0.3299404806269776169, 0.3333333333333333703, 0.3299404806269776169, 0.3333333333333333703, 0.3299404806269776169, 0.3333333333333333703, 0.3299404806269776169, 0.3333333333333333703, 0.3299404806269776169, 0.3333333333333333703, 0.3299404806269776169, 0.3333333333333333703, 0.3299404806269776169, 0.3333333333333333703, 0.3299404806269776169, 0.3333333333333333703, 0.3299404806269776169, 0.3333333333333333703, 0.3299404806269776169, 0.3333333333333333703, 0.3299404806269776169, 0.3333333333333333703, 0.3299404806269776169, 0.3333333333333333703, 0.3299404806269776169, 0.3333333333333333703, 0.3299404806269776169, 0.3333333333333333703, 0.3299404806269776169, 0.3333333333333333703, 0.3299404806269776169, 0.3333333333333333703, 0.3299404806269776169, 0.3333333333333333703, 0.3299404806269776169, 0.3333333333333333703, 0.3299404806269776169, 0.3333333333333333703, 0.3299404806269776169, 0.3333333333333333703, 0.3299404806269776169, 0.3333333333333333703, 0.3299404806269776169, 0.3333333333333333703, 0.3299404806269776169, 0.3333333333333333703, 0.3299404806269776169, 0.3333333333333333703, 0.3299404806269776169, 0.3333333333333333703, 0.3299404806269776169, 0.3333333333333333703, 0.3299404806269776169, 0.3333333333333333703, 0.3299404806269776169, 0.3333333333333333703, 0.3299404806269776169, 0.3333333333333333703, 0.3299404806269776169, 0.3333333333333333703, 0.3299404806269776169, 0.3333333333333333703, 0.3299404806269776169, 0.3333333333333333703, 0.3299404806269776169, 0.3333333333333333703, 0.3299404806269776169, 0.3333333333333333703, 0.3299404806269776169, 0.3333333333333333703, 0.3299404806269776169, 0.3333333333333333703, 0.3299404806269776169, 0.3333333333333333703, 0.3299404806269776169, 0.3333333333333333703, 0.3299404806269776169, 0.3333333333333333703, 0.3299404806269776169, 0.3333333333333333703, 0.3299404806269776169, 0.3333333333333333703, 0.3299404806269776169, 0.3333333333333333703, 0.3299404806269776169, 0.3333333333333333703, 0.3299404806269776169, 0.3333333333333333703, 0.3299404806269776169, 0.3333333333333333703, 0.3299404806269776169, 0.3333333333333333703, 0.3299404806269776169, 0.3333333333333333703, 0.3299404806269776169, 0.3333333333333333703, 0.3299404806269776169, 0.3333333333333333703, 0.3299404806269776169, 0.3333333333333333703, 0.3299404806269776169, 0.3333333333333333703, 0.3299404806269776169, 0.3333333333333333703, 0.3299404806269776169, 0.3333333333333333703, 0.3299404806269776169, 0.3333333333333333703, 0.3299404806269776169, 0.3333333333333333703, 0.3299404806269776169, 0.3333333333333333703, 0.3299404806269776169, 0.3333333333333333703, 0.3299404806269776169, 0.3333333333333333703, 0.3299404806269776169, 0.3333333333333333703, 0.3299404806269776169, 0.3333333333333333703, 0.3299404806269776169, 0.3333333333333333703, 0.3299404806269776169, 0.3333333333333333703, 0.3299404806269776169, 0.3333333333333333703, 0.3299404806269776169, 0.3333333333333333703, 0.3299404806269776169, 0.3333333333333333703, 0.3299404806269776169, 0.3333333333333333703, 0.3299404806269776169, 0.3333333333333333703, 0.3299404806269776169, 0.3333333333333333703, 0.3299404806269776169, 0.3333333333333333703, 0.3299404806269776169, 0.3333333333333333703, 0.3299404806269776169, 0.3333333333333333703, 0.3299404806269776169, 0.3333333333333333703, 0.3299404806269776169, 0.3333333333333333703, 0.3299404806269776169, 0.3333333333333333703, 0.3299404806269776169, 0.3333333333333333703, 0.3299404806269776169, 0.3333333333333333703, 0.3299404806269776169, 0.3333333333333333703, 0.3299404806269776169, 0.3333333333333333703, 0.3299404806269776169, 0.3333333333333333703, 0.3299404806269776169, 0.3333333333333333703, 0.3299404806269776169, 0.3333333333333333703, 0.3299404806269776169, 0.3333333333333333703, 0.3299404806269776169, 0.3333333333333333703, 0.3299404806269776169, 0.3333333333333333703, 0.3299404806269776169, 0.3333333333333333703, 0.3299404806269776169, 0.3333333333333333703, 0.3299404806269776169, 0.3333333333333333703, 0.3299404806269776169, 0.3333333333333333703, 0.3299404806269776169, 0.3333333333333333703, 0.3299404806269776169, 0.3333333333333333703, 0.3299404806269776169, 0.3333333333333333703, 0.3299404806269776169, 0.3333333333333333703, 0.3299404806269776169, 0.3333333333333333703, 0.3299404806269776169, 0.3333333333333333703, 0.3299404806269776169, 0.3333333333333333703, 0.3299404806269776169, 0.3333333333333333703, 0.3299404806269776169, 0.3333333333333333703, 0.3299404806269776169, 0.3333333333333333703, 0.3299404806269776169, 0.3333333333333333703, 0.3299404806269776169, 0.3333333333333333703, 0.3299404806269776169, 0.3333333333333333703, 0.3299404806269776169, 0.3333333333333333703, 0.3299404806269776169, 0.3333333333333333703, 0.3299404806269776169, 0.3333333333333333703, 0.3299404806269776169, 0.3333333333333333703, 0.3299404806269776169, 0.3333333333333333703, 0.3299404806269776169, 0.3333333333333333703, 0.3299404806269776169, 0.3333333333333333703, 0.3299404806269776169, 0.3333333333333333703, 0.3299404806269776169, 0.3333333333333333703, 0.3299404806269776169, 0.3333333333333333703, 0.3299404806269776169, 0.3333333333333333703, 0.3299404806269776169, 0.3333333333333333703, 0.3299404806269776169, 0.3333333333333333703, 0.3299404806269776169, 0.3333333333333333703, 0.3299404806269776169, 0.3333333333333333703, 0.3299404806269776169, 0.3333333333333333703, 0.3299404806269776169, 0.3333333333333333703, 0.3299404806269776169, 0.3333333333333333703, 0.3299404806269776169, 0.3333333333333333703, 0.3299404806269776169, 0.3333333333333333703, 0.3299404806269776169, 0.3333333333333333703, 0.3299404806269776169, 0.3333333333333333703, 0.3299404806269776169, 0.3333333333333333703, 0.3299404806269776169, 0.3333333333333333703, 0.3299404806269776169, 0.3333333333333333703, 0.3299404806269776169, 0.3333333333333333703, 0.3299404806269776169, 0.3333333333333333703, 0.3299404806269776169, 0.3333333333333333703, 0.3299404806269776169, 0.3333333333333333703, 0.3299404806269776169, 0.3333333333333333703, 0.3299404806269776169, 0.3333333333333333703, 0.3299404806269776169, 0.3333333333333333703, 0.3299404806269776169, 0.3333333333333333703, 0.3299404806269776169, 0.3333333333333333703, 0.3299404806269776169, 0.3333333333333333703, 0.3299404806269776169, 0.3333333333333333703, 0.3299404806269776169, 0.3333333333333333703, 0.3299404806269776169, 0.3333333333333333703, 0.3299404806269776169, 0.3333333333333333703, 0.3299404806269776169, 0.3333333333333333703, 0.3299404806269776169, 0.3333333333333333703, 0.3299404806269776169, 0.3333333333333333703, 0.3299404806269776169, 0.3333333333333333703, 0.3299404806269776169, 0.3333333333333333703, 0.3299404806269776169, 0.3333333333333333703, 0.3299404806269776169, 0.3333333333333333703, 0.3299404806269776169, 0.3333333333333333703, 0.3299404806269776169, 0.3333333333333333703, 0.3299404806269776169, 0.3333333333333333703, 0.3299404806269776169, 0.3333333333333333703, 0.3299404806269776169, 0.3333333333333333703, 0.3299404806269776169, 0.3333333333333333703, 0.3299404806269776169, 0.3333333333333333703, 0.3299404806269776169, 0.3333333333333333703, 0.3299404806269776169, 0.3333333333333333703, 0.3299404806269776169, 0.3333333333333333703, 0.3299404806269776169, 0.3333333333333333703, 0.3299404806269776169, 0.3333333333333333703, 0.3299404806269776169, 0.3333333333333333703, 0.3299404806269776169, 0.3333333333333333703, 0.3299404806269776169, 0.3333333333333333703, 0.3299404806269776169, 0.3333333333333333703, 0.3299404806269776169, 0.3333333333333333703, 0.3299404806269776169, 0.3333333333333333703, 0.3299404806269776169, 0.3333333333333333703, 0.3299404806269776169, 0.3333333333333333703, 0.3299404806269776169, 0.3333333333333333703, 0.3299404806269776169, 0.3333333333333333703, 0.3299404806269776169, 0.3333333333333333703, 0.3299404806269776169, 0.3333333333333333703, 0.3299404806269776169, 0.3333333333333333703, 0.3299404806269776169, 0.3333333333333333703, 0.3299404806269776169, 0.3333333333333333703, 0.3299404806269776169, 0.3333333333333333703, 0.3299404806269776169, 0.3333333333333333703, 0.3299404806269776169, 0.3333333333333333703, 0.3299404806269776169, 0.3333333333333333703, 0.3299404806269776169, 0.3333333333333333703, 0.3299404806269776169, 0.3333333333333333703, 0.3299404806269776169, 0.3333333333333333703, 0.3299404806269776169, 0.3333333333333333703, 0.3299404806269776169, 0.3333333333333333703, 0.3299404806269776169, 0.3333333333333333703, 0.3299404806269776169, 0.3333333333333333703, 0.3299404806269776169, 0.3333333333333333703, 0.3299404806269776169, 0.3333333333333333703, 0.3299404806269776169, 0.3333333333333333703, 0.3299404806269776169, 0.3333333333333333703, 0.3299404806269776169, 0.3333333333333333703, 0.3299404806269776169, 0.3333333333333333703, 0.3299404806269776169, 0.3333333333333333703, 0.3299404806269776169, 0.3333333333333333703, 0.3299404806269776169, 0.3333333333333333703, 0.3299404806269776169, 0.3333333333333333703, 0.3299404806269776169, 0.3333333333333333703, 0.3299404806269776169, 0.3333333333333333703, 0.3299404806269776169, 0.3333333333333333703, 0.3299404806269776169, 0.3333333333333333703, 0.3299404806269776169, 0.3333333333333333703, 0.3299404806269776169, 0.3333333333333333703, 0.3299404806269776169, 0.3333333333333333703, 0.3299404806269776169, 0.3333333333333333703, 0.3299404806269776169, 0.3333333333333333703, 0.3299404806269776169, 0.3333333333333333703, 0.3299404806269776169, 0.3333333333333333703, 0.3299404806269776169, 0.3333333333333333703, 0.3299404806269776169, 0.3333333333333333703, 0.3299404806269776169, 0.3333333333333333703, 0.3299404806269776169, 0.3333333333333333703, 0.3299404806269776169, 0.3333333333333333703, 0.3299404806269776169, 0.3333333333333333703, 0.3299404806269776169, 0.3333333333333333703, 0.3299404806269776169, 0.3333333333333333703, 0.3299404806269776169, 0.3333333333333333703, 0.3299404806269776169, 0.3333333333333333703, 0.3299404806269776169, 0.3333333333333333703, 0.3299404806269776169, 0.3333333333333333703, 0.3299404806269776169, 0.3333333333333333703, 0.3299404806269776169, 0.3333333333333333703, 0.3299404806269776169, 0.3333333333333333703, 0.3299404806269776169, 0.3333333333333333703, 0.3299404806269776169, 0.3333333333333333703, 0.3299404806269776169, 0.3333333333333333703, 0.3299404806269776169, 0.3333333333333333703, 0.3299404806269776169, 0.3333333333333333703, 0.3299404806269776169, 0.3333333333333333703, 0.3299404806269776169, 0.3333333333333333703, 0.3299404806269776169, 0.3333333333333333703, 0.3299404806269776169, 0.3333333333333333703, 0.3299404806269776169, 0.3333333333333333703, 0.3299404806269776169, 0.3333333333333333703, 0.3299404806269776169, 0.3333333333333333703, 0.3299404806269776169, 0.3333333333333333703, 0.3299404806269776169, 0.3333333333333333703, 0.3299404806269776169, 0.3333333333333333703, 0.3299404806269776169, 0.3333333333333333703, 0.3299404806269776169, 0.3333333333333333703, 0.3299404806269776169, 0.3333333333333333703, 0.3299404806269776169, 0.3333333333333333703, 0.3299404806269776169, 0.3333333333333333703, 0.3299404806269776169, 0.3333333333333333703, 0.3299404806269776169, 0.3333333333333333703, 0.3299404806269776169, 0.3333333333333333703, 0.3299404806269776169, 0.3333333333333333703, 0.3299404806269776169, 0.3333333333333333703, 0.3299404806269776169, 0.3333333333333333703, 0.3299404806269776169, 0.3333333333333333703, 0.3299404806269776169, 0.3333333333333333703, 0.3299404806269776169, 0.3333333333333333703, 0.3299404806269776169, 0.3333333333333333703, 0.3299404806269776169, 0.3333333333333333703, 0.3299404806269776169, 0.3333333333333333703, 0.3299404806269776169, 0.3333333333333333703, 0.3299404806269776169, 0.3333333333333333703, 0.3299404806269776169, 0.3333333333333333703, 0.3299404806269776169, 0.3333333333333333703, 0.3299404806269776169, 0.3333333333333333703, 0.3299404806269776169, 0.3333333333333333703, 0.3299404806269776169, 0.3333333333333333703, 0.3299404806269776169, 0.3333333333333333703, 0.3299404806269776169, 0.3333333333333333703, 0.3299404806269776169, 0.3333333333333333703, 0.3299404806269776169, 0.3333333333333333703, 0.3299404806269776169, 0.3333333333333333703, 0.3299404806269776169, 0.3333333333333333703, 0.3299404806269776169, 0.3333333333333333703, 0.3299404806269776169, 0.3333333333333333703, 0.3299404806269776169, 0.3333333333333333703, 0.3299404806269776169, 0.3333333333333333703, 0.3299404806269776169, 0.3333333333333333703, 0.3299404806269776169, 0.3333333333333333703, 0.3299404806269776169, 0.3333333333333333703, 0.3299404806269776169, 0.3333333333333333703, 0.3299404806269776169, 0.3333333333333333703, 0.3299404806269776169, 0.3333333333333333703, 0.3299404806269776169, 0.3333333333333333703, 0.3299404806269776169, 0.3333333333333333703, 0.3299404806269776169, 0.3333333333333333703, 0.3299404806269776169, 0.3333333333333333703, 0.3299404806269776169, 0.3333333333333333703, 0.3299404806269776169, 0.3333333333333333703, 0.3299404806269776169, 0.3333333333333333703, 0.3299404806269776169, 0.3333333333333333703, 0.3299404806269776169, 0.3333333333333333703, 0.3299404806269776169, 0.3333333333333333703, 0.3299404806269776169, 0.3333333333333333703, 0.3299404806269776169, 0.3333333333333333703, 0.3299404806269776169, 0.3333333333333333703, 0.3299404806269776169, 0.3333333333333333703, 0.3299404806269776169, 0.3333333333333333703, 0.3299404806269776169, 0.3333333333333333703, 0.3299404806269776169, 0.3333333333333333703, 0.3299404806269776169, 0.3333333333333333703, 0.3299404806269776169, 0.3333333333333333703, 0.3299404806269776169, 0.3333333333333333703, 0.3299404806269776169, 0.3333333333333333703, 0.3299404806269776169, 0.3333333333333333703, 0.3299404806269776169, 0.3333333333333333703, 0.3299404806269776169, 0.3333333333333333703, 0.3299404806269776169, 0.3333333333333333703, 0.3299404806269776169, 0.3333333333333333703, 0.3299404806269776169, 0.3333333333333333703, 0.3299404806269776169, 0.3333333333333333703, 0.3299404806269776169, 0.3333333333333333703, 0.3299404806269776169, 0.3333333333333333703, 0.3299404806269776169, 0.3333333333333333703, 0.3299404806269776169, 0.3333333333333333703, 0.3299404806269776169, 0.3333333333333333703, 0.3299404806269776169, 0.3333333333333333703, 0.3299404806269776169, 0.3333333333333333703, 0.3299404806269776169, 0.3333333333333333703, 0.3299404806269776169, 0.3333333333333333703, 0.3299404806269776169, 0.3333333333333333703, 0.3299404806269776169, 0.3333333333333333703, 0.3299404806269776169, 0.3333333333333333703, 0.3299404806269776169, 0.3333333333333333703, 0.3299404806269776169, 0.3333333333333333703, 0.3299404806269776169, 0.3333333333333333703, 0.3299404806269776169, 0.3333333333333333703, 0.3299404806269776169, 0.3333333333333333703, 0.3299404806269776169, 0.3333333333333333703, 0.3299404806269776169, 0.3333333333333333703, 0.3299404806269776169, 0.3333333333333333703, 0.3299404806269776169, 0.3333333333333333703, 0.3299404806269776169, 0.3333333333333333703, 0.3299404806269776169, 0.3333333333333333703, 0.3299404806269776169, 0.3333333333333333703, 0.3299404806269776169, 0.3333333333333333703, 0.3299404806269776169, 0.3333333333333333703, 0.3299404806269776169, 0.3333333333333333703, 0.3299404806269776169, 0.3333333333333333703, 0.3299404806269776169, 0.3333333333333333703, 0.3299404806269776169, 0.3333333333333333703, 0.3299404806269776169, 0.3333333333333333703, 0.3299404806269776169, 0.3333333333333333703, 0.3299404806269776169, 0.3333333333333333703, 0.3299404806269776169, 0.3333333333333333703, 0.3299404806269776169, 0.3333333333333333703, 0.3299404806269776169, 0.3333333333333333703, 0.3299404806269776169, 0.3333333333333333703, 0.3299404806269776169, 0.3333333333333333703, 0.3299404806269776169, 0.3333333333333333703, 0.3299404806269776169, 0.3333333333333333703, 0.3299404806269776169, 0.3333333333333333703, 0.3299404806269776169, 0.3333333333333333703, 0.3299404806269776169, 0.3333333333333333703, 0.3299404806269776169, 0.3333333333333333703, 0.3299404806269776169, 0.3333333333333333703, 0.3299404806269776169, 0.3333333333333333703, 0.3299404806269776169, 0.3333333333333333703, 0.3320603117974822438, 0.3317425830320511193),
 ( 0.3333333333333333703, 0.3299404806269776169, 0.3333333333333333703, 0.3299404806269776169, 0.3333333333333333703, 0.3299404806269776169, 0.3333333333333333703, 0.3299404806269776169, 0.3333333333333333703, 0.3299404806269776169, 0.3333333333333333703, 0.3299404806269776169, 0.3333333333333333703, 0.3299404806269776169, 0.3333333333333333703, 0.3299404806269776169, 0.3333333333333333703, 0.3299404806269776169, 0.3333333333333333703, 0.3299404806269776169, 0.3333333333333333703, 0.3299404806269776169, 0.3333333333333333703, 0.3299404806269776169, 0.3333333333333333703, 0.3299404806269776169, 0.3333333333333333703, 0.3299404806269776169, 0.3333333333333333703, 0.3299404806269776169, 0.3333333333333333703, 0.3299404806269776169, 0.3333333333333333703, 0.3299404806269776169, 0.3333333333333333703, 0.3299404806269776169, 0.3333333333333333703, 0.3299404806269776169, 0.3333333333333333703, 0.3299404806269776169, 0.3333333333333333703, 0.3299404806269776169, 0.3333333333333333703, 0.3299404806269776169, 0.3333333333333333703, 0.3299404806269776169, 0.3333333333333333703, 0.3299404806269776169, 0.3333333333333333703, 0.3299404806269776169, 0.3333333333333333703, 0.3299404806269776169, 0.3333333333333333703, 0.3299404806269776169, 0.3333333333333333703, 0.3299404806269776169, 0.3333333333333333703, 0.3299404806269776169, 0.3333333333333333703, 0.3299404806269776169, 0.3333333333333333703, 0.3299404806269776169, 0.3333333333333333703, 0.3299404806269776169, 0.3333333333333333703, 0.3299404806269776169, 0.3333333333333333703, 0.3299404806269776169, 0.3333333333333333703, 0.3299404806269776169, 0.3333333333333333703, 0.3299404806269776169, 0.3333333333333333703, 0.3299404806269776169, 0.3333333333333333703, 0.3299404806269776169, 0.3333333333333333703, 0.3299404806269776169, 0.3333333333333333703, 0.3299404806269776169, 0.3333333333333333703, 0.3299404806269776169, 0.3333333333333333703, 0.3299404806269776169, 0.3333333333333333703, 0.3299404806269776169, 0.3333333333333333703, 0.3299404806269776169, 0.3333333333333333703, 0.3299404806269776169, 0.3333333333333333703, 0.3299404806269776169, 0.3333333333333333703, 0.3299404806269776169, 0.3333333333333333703, 0.3299404806269776169, 0.3333333333333333703, 0.3299404806269776169, 0.3333333333333333703, 0.3299404806269776169, 0.3333333333333333703, 0.3299404806269776169, 0.3333333333333333703, 0.3299404806269776169, 0.3333333333333333703, 0.3299404806269776169, 0.3333333333333333703, 0.3299404806269776169, 0.3333333333333333703, 0.3299404806269776169, 0.3333333333333333703, 0.3299404806269776169, 0.3333333333333333703, 0.3299404806269776169, 0.3333333333333333703, 0.3299404806269776169, 0.3333333333333333703, 0.3299404806269776169, 0.3333333333333333703, 0.3299404806269776169, 0.3333333333333333703, 0.3299404806269776169, 0.3333333333333333703, 0.3299404806269776169, 0.3333333333333333703, 0.3299404806269776169, 0.3333333333333333703, 0.3299404806269776169, 0.3333333333333333703, 0.3299404806269776169, 0.3333333333333333703, 0.3299404806269776169, 0.3333333333333333703, 0.3299404806269776169, 0.3333333333333333703, 0.3299404806269776169, 0.3333333333333333703, 0.3299404806269776169, 0.3333333333333333703, 0.3299404806269776169, 0.3333333333333333703, 0.3299404806269776169, 0.3333333333333333703, 0.3299404806269776169, 0.3333333333333333703, 0.3299404806269776169, 0.3333333333333333703, 0.3299404806269776169, 0.3333333333333333703, 0.3299404806269776169, 0.3333333333333333703, 0.3299404806269776169, 0.3333333333333333703, 0.3299404806269776169, 0.3333333333333333703, 0.3299404806269776169, 0.3333333333333333703, 0.3299404806269776169, 0.3333333333333333703, 0.3299404806269776169, 0.3333333333333333703, 0.3299404806269776169, 0.3333333333333333703, 0.3299404806269776169, 0.3333333333333333703, 0.3299404806269776169, 0.3333333333333333703, 0.3299404806269776169, 0.3333333333333333703, 0.3299404806269776169, 0.3333333333333333703, 0.3299404806269776169, 0.3333333333333333703, 0.3299404806269776169, 0.3333333333333333703, 0.3299404806269776169, 0.3333333333333333703, 0.3299404806269776169, 0.3333333333333333703, 0.3299404806269776169, 0.3333333333333333703, 0.3299404806269776169, 0.3333333333333333703, 0.3299404806269776169, 0.3333333333333333703, 0.3299404806269776169, 0.3333333333333333703, 0.3299404806269776169, 0.3333333333333333703, 0.3299404806269776169, 0.3333333333333333703, 0.3299404806269776169, 0.3333333333333333703, 0.3299404806269776169, 0.3333333333333333703, 0.3299404806269776169, 0.3333333333333333703, 0.3299404806269776169, 0.3333333333333333703, 0.3299404806269776169, 0.3333333333333333703, 0.3299404806269776169, 0.3333333333333333703, 0.3299404806269776169, 0.3333333333333333703, 0.3299404806269776169, 0.3333333333333333703, 0.3299404806269776169, 0.3333333333333333703, 0.3299404806269776169, 0.3333333333333333703, 0.3299404806269776169, 0.3333333333333333703, 0.3299404806269776169, 0.3333333333333333703, 0.3299404806269776169, 0.3333333333333333703, 0.3299404806269776169, 0.3333333333333333703, 0.3299404806269776169, 0.3333333333333333703, 0.3299404806269776169, 0.3333333333333333703, 0.3299404806269776169, 0.3333333333333333703, 0.3299404806269776169, 0.3333333333333333703, 0.3299404806269776169, 0.3333333333333333703, 0.3299404806269776169, 0.3333333333333333703, 0.3299404806269776169, 0.3333333333333333703, 0.3299404806269776169, 0.3333333333333333703, 0.3299404806269776169, 0.3333333333333333703, 0.3299404806269776169, 0.3333333333333333703, 0.3299404806269776169, 0.3333333333333333703, 0.3299404806269776169, 0.3333333333333333703, 0.3299404806269776169, 0.3333333333333333703, 0.3299404806269776169, 0.3333333333333333703, 0.3299404806269776169, 0.3333333333333333703, 0.3299404806269776169, 0.3333333333333333703, 0.3299404806269776169, 0.3333333333333333703, 0.3299404806269776169, 0.3333333333333333703, 0.3299404806269776169, 0.3333333333333333703, 0.3299404806269776169, 0.3333333333333333703, 0.3299404806269776169, 0.3333333333333333703, 0.3299404806269776169, 0.3333333333333333703, 0.3299404806269776169, 0.3333333333333333703, 0.3299404806269776169, 0.3333333333333333703, 0.3299404806269776169, 0.3333333333333333703, 0.3299404806269776169, 0.3333333333333333703, 0.3299404806269776169, 0.3333333333333333703, 0.3299404806269776169, 0.3333333333333333703, 0.3299404806269776169, 0.3333333333333333703, 0.3299404806269776169, 0.3333333333333333703, 0.3299404806269776169, 0.3333333333333333703, 0.3299404806269776169, 0.3333333333333333703, 0.3299404806269776169, 0.3333333333333333703, 0.3299404806269776169, 0.3333333333333333703, 0.3299404806269776169, 0.3333333333333333703, 0.3299404806269776169, 0.3333333333333333703, 0.3299404806269776169, 0.3333333333333333703, 0.3299404806269776169, 0.3333333333333333703, 0.3299404806269776169, 0.3333333333333333703, 0.3299404806269776169, 0.3333333333333333703, 0.3299404806269776169, 0.3333333333333333703, 0.3299404806269776169, 0.3333333333333333703, 0.3299404806269776169, 0.3333333333333333703, 0.3299404806269776169, 0.3333333333333333703, 0.3299404806269776169, 0.3333333333333333703, 0.3299404806269776169, 0.3333333333333333703, 0.3299404806269776169, 0.3333333333333333703, 0.3299404806269776169, 0.3333333333333333703, 0.3299404806269776169, 0.3333333333333333703, 0.3299404806269776169, 0.3333333333333333703, 0.3299404806269776169, 0.3333333333333333703, 0.3299404806269776169, 0.3333333333333333703, 0.3299404806269776169, 0.3333333333333333703, 0.3299404806269776169, 0.3333333333333333703, 0.3299404806269776169, 0.3333333333333333703, 0.3299404806269776169, 0.3333333333333333703, 0.3299404806269776169, 0.3333333333333333703, 0.3299404806269776169, 0.3333333333333333703, 0.3299404806269776169, 0.3333333333333333703, 0.3299404806269776169, 0.3333333333333333703, 0.3299404806269776169, 0.3333333333333333703, 0.3299404806269776169, 0.3333333333333333703, 0.3299404806269776169, 0.3333333333333333703, 0.3299404806269776169, 0.3333333333333333703, 0.3299404806269776169, 0.3333333333333333703, 0.3299404806269776169, 0.3333333333333333703, 0.3299404806269776169, 0.3333333333333333703, 0.3299404806269776169, 0.3333333333333333703, 0.3299404806269776169, 0.3333333333333333703, 0.3299404806269776169, 0.3333333333333333703, 0.3299404806269776169, 0.3333333333333333703, 0.3299404806269776169, 0.3333333333333333703, 0.3299404806269776169, 0.3333333333333333703, 0.3299404806269776169, 0.3333333333333333703, 0.3299404806269776169, 0.3333333333333333703, 0.3299404806269776169, 0.3333333333333333703, 0.3299404806269776169, 0.3333333333333333703, 0.3299404806269776169, 0.3333333333333333703, 0.3299404806269776169, 0.3333333333333333703, 0.3299404806269776169, 0.3333333333333333703, 0.3299404806269776169, 0.3333333333333333703, 0.3299404806269776169, 0.3333333333333333703, 0.3299404806269776169, 0.3333333333333333703, 0.3299404806269776169, 0.3333333333333333703, 0.3299404806269776169, 0.3333333333333333703, 0.3299404806269776169, 0.3333333333333333703, 0.3299404806269776169, 0.3333333333333333703, 0.3299404806269776169, 0.3333333333333333703, 0.3299404806269776169, 0.3333333333333333703, 0.3299404806269776169, 0.3333333333333333703, 0.3299404806269776169, 0.3333333333333333703, 0.3299404806269776169, 0.3333333333333333703, 0.3299404806269776169, 0.3333333333333333703, 0.3299404806269776169, 0.3333333333333333703, 0.3299404806269776169, 0.3333333333333333703, 0.3299404806269776169, 0.3333333333333333703, 0.3299404806269776169, 0.3333333333333333703, 0.3299404806269776169, 0.3333333333333333703, 0.3299404806269776169, 0.3333333333333333703, 0.3299404806269776169, 0.3333333333333333703, 0.3299404806269776169, 0.3333333333333333703, 0.3299404806269776169, 0.3333333333333333703, 0.3299404806269776169, 0.3333333333333333703, 0.3299404806269776169, 0.3333333333333333703, 0.3299404806269776169, 0.3333333333333333703, 0.3299404806269776169, 0.3333333333333333703, 0.3299404806269776169, 0.3333333333333333703, 0.3299404806269776169, 0.3333333333333333703, 0.3299404806269776169, 0.3333333333333333703, 0.3299404806269776169, 0.3333333333333333703, 0.3299404806269776169, 0.3333333333333333703, 0.3299404806269776169, 0.3333333333333333703, 0.3299404806269776169, 0.3333333333333333703, 0.3299404806269776169, 0.3333333333333333703, 0.3299404806269776169, 0.3333333333333333703, 0.3299404806269776169, 0.3333333333333333703, 0.3299404806269776169, 0.3333333333333333703, 0.3299404806269776169, 0.3333333333333333703, 0.3299404806269776169, 0.3333333333333333703, 0.3299404806269776169, 0.3333333333333333703, 0.3299404806269776169, 0.3333333333333333703, 0.3299404806269776169, 0.3333333333333333703, 0.3299404806269776169, 0.3333333333333333703, 0.3299404806269776169, 0.3333333333333333703, 0.3299404806269776169, 0.3333333333333333703, 0.3299404806269776169, 0.3333333333333333703, 0.3299404806269776169, 0.3333333333333333703, 0.3299404806269776169, 0.3333333333333333703, 0.3299404806269776169, 0.3333333333333333703, 0.3299404806269776169, 0.3333333333333333703, 0.3299404806269776169, 0.3333333333333333703, 0.3299404806269776169, 0.3333333333333333703, 0.3299404806269776169, 0.3333333333333333703, 0.3299404806269776169, 0.3333333333333333703, 0.3299404806269776169, 0.3333333333333333703, 0.3299404806269776169, 0.3333333333333333703, 0.3299404806269776169, 0.3333333333333333703, 0.3299404806269776169, 0.3333333333333333703, 0.3299404806269776169, 0.3333333333333333703, 0.3299404806269776169, 0.3333333333333333703, 0.3299404806269776169, 0.3333333333333333703, 0.3299404806269776169, 0.3333333333333333703, 0.3299404806269776169, 0.3333333333333333703, 0.3299404806269776169, 0.3333333333333333703, 0.3299404806269776169, 0.3333333333333333703, 0.3299404806269776169, 0.3333333333333333703, 0.3299404806269776169, 0.3333333333333333703, 0.3299404806269776169, 0.3333333333333333703, 0.3299404806269776169, 0.3333333333333333703, 0.3299404806269776169, 0.3333333333333333703, 0.3299404806269776169, 0.3333333333333333703, 0.3299404806269776169, 0.3333333333333333703, 0.3299404806269776169, 0.3333333333333333703, 0.3299404806269776169, 0.3333333333333333703, 0.3299404806269776169, 0.3333333333333333703, 0.3299404806269776169, 0.3333333333333333703, 0.3299404806269776169, 0.3333333333333333703, 0.3299404806269776169, 0.3333333333333333703, 0.3299404806269776169, 0.3333333333333333703, 0.3299404806269776169, 0.3333333333333333703, 0.3299404806269776169, 0.3333333333333333703, 0.3299404806269776169, 0.3333333333333333703, 0.3299404806269776169, 0.3333333333333333703, 0.3299404806269776169, 0.3333333333333333703, 0.3299404806269776169, 0.3333333333333333703, 0.3299404806269776169, 0.3333333333333333703, 0.3299404806269776169, 0.3333333333333333703, 0.3299404806269776169, 0.3333333333333333703, 0.3299404806269776169, 0.3333333333333333703, 0.3299404806269776169, 0.3333333333333333703, 0.3299404806269776169, 0.3333333333333333703, 0.3299404806269776169, 0.3333333333333333703, 0.3299404806269776169, 0.3333333333333333703, 0.3299404806269776169, 0.3333333333333333703, 0.3299404806269776169, 0.3333333333333333703, 0.3299404806269776169, 0.3333333333333333703, 0.3299404806269776169, 0.3333333333333333703, 0.3299404806269776169, 0.3333333333333333703, 0.3299404806269776169, 0.3333333333333333703, 0.3299404806269776169, 0.3333333333333333703, 0.3299404806269776169, 0.3333333333333333703, 0.3299404806269776169, 0.3333333333333333703, 0.3299404806269776169, 0.3333333333333333703, 0.3299404806269776169, 0.3333333333333333703, 0.3299404806269776169, 0.3333333333333333703, 0.3299404806269776169, 0.3333333333333333703, 0.3299404806269776169, 0.3333333333333333703, 0.3299404806269776169, 0.3333333333333333703, 0.3299404806269776169, 0.3333333333333333703, 0.3299404806269776169, 0.3333333333333333703, 0.3299404806269776169, 0.3333333333333333703, 0.3299404806269776169, 0.3333333333333333703, 0.3299404806269776169, 0.3333333333333333703, 0.3299404806269776169, 0.3333333333333333703, 0.3299404806269776169, 0.3333333333333333703, 0.3299404806269776169, 0.3333333333333333703, 0.3299404806269776169, 0.3333333333333333703, 0.3299404806269776169, 0.3333333333333333703, 0.3299404806269776169, 0.3333333333333333703, 0.3299404806269776169, 0.3333333333333333703, 0.3299404806269776169, 0.3333333333333333703, 0.3299404806269776169, 0.3333333333333333703, 0.3299404806269776169, 0.3333333333333333703, 0.3299404806269776169, 0.3333333333333333703, 0.3299404806269776169, 0.3333333333333333703, 0.3299404806269776169, 0.3333333333333333703, 0.3299404806269776169, 0.3333333333333333703, 0.3299404806269776169, 0.3333333333333333703, 0.3299404806269776169, 0.3333333333333333703, 0.3299404806269776169, 0.3333333333333333703, 0.3299404806269776169, 0.3333333333333333703, 0.3299404806269776169, 0.3333333333333333703, 0.3299404806269776169, 0.3333333333333333703, 0.3299404806269776169, 0.3333333333333333703, 0.3299404806269776169, 0.3333333333333333703, 0.3299404806269776169, 0.3333333333333333703, 0.3299404806269776169, 0.3333333333333333703, 0.3299404806269776169, 0.3333333333333333703, 0.3299404806269776169, 0.3333333333333333703, 0.3299404806269776169, 0.3333333333333333703, 0.3299404806269776169, 0.3333333333333333703, 0.3299404806269776169, 0.3333333333333333703, 0.3299404806269776169, 0.3333333333333333703, 0.3299404806269776169, 0.3333333333333333703, 0.3299404806269776169, 0.3333333333333333703, 0.3299404806269776169, 0.3333333333333333703, 0.3299404806269776169, 0.3333333333333333703, 0.3299404806269776169, 0.3333333333333333703, 0.3299404806269776169, 0.3333333333333333703, 0.3299404806269776169, 0.3333333333333333703, 0.3299404806269776169, 0.3333333333333333703, 0.3299404806269776169, 0.3333333333333333703, 0.3299404806269776169, 0.3333333333333333703, 0.3299404806269776169, 0.3333333333333333703, 0.3299404806269776169, 0.3333333333333333703, 0.3299404806269776169, 0.3333333333333333703, 0.3299404806269776169, 0.3333333333333333703, 0.3299404806269776169, 0.3333333333333333703, 0.3299404806269776169, 0.3333333333333333703, 0.3299404806269776169, 0.3333333333333333703, 0.3299404806269776169, 0.3333333333333333703, 0.3299404806269776169, 0.3333333333333333703, 0.3299404806269776169, 0.3333333333333333703, 0.3299404806269776169, 0.3333333333333333703, 0.3299404806269776169, 0.3333333333333333703, 0.3299404806269776169, 0.3333333333333333703, 0.3299404806269776169, 0.3333333333333333703, 0.3299404806269776169, 0.3333333333333333703, 0.3299404806269776169, 0.3333333333333333703, 0.3299404806269776169, 0.3333333333333333703, 0.3299404806269776169, 0.3333333333333333703, 0.3299404806269776169, 0.3333333333333333703, 0.3299404806269776169, 0.3333333333333333703, 0.3299404806269776169, 0.3333333333333333703, 0.3299404806269776169, 0.3333333333333333703, 0.3299404806269776169, 0.3333333333333333703, 0.3299404806269776169, 0.3333333333333333703, 0.3299404806269776169, 0.3333333333333333703, 0.3299404806269776169, 0.3333333333333333703, 0.3299404806269776169, 0.3333333333333333703, 0.3299404806269776169, 0.3333333333333333703, 0.3299404806269776169, 0.3333333333333333703, 0.3299404806269776169, 0.3333333333333333703, 0.3299404806269776169, 0.3333333333333333703, 0.3299404806269776169, 0.3333333333333333703, 0.3299404806269776169, 0.3333333333333333703, 0.3299404806269776169, 0.3333333333333333703, 0.3299404806269776169, 0.3333333333333333703, 0.3299404806269776169, 0.3333333333333333703, 0.3299404806269776169, 0.3333333333333333703, 0.3299404806269776169, 0.3333333333333333703, 0.3299404806269776169, 0.3333333333333333703, 0.3299404806269776169, 0.3333333333333333703, 0.3299404806269776169, 0.3333333333333333703, 0.3299404806269776169, 0.3333333333333333703, 0.3299404806269776169, 0.3333333333333333703, 0.3299404806269776169, 0.3333333333333333703, 0.3299404806269776169, 0.3333333333333333703, 0.3299404806269776169, 0.3333333333333333703, 0.3299404806269776169, 0.3333333333333333703, 0.3299404806269776169, 0.3333333333333333703, 0.3299404806269776169, 0.3333333333333333703, 0.3299404806269776169, 0.3333333333333333703, 0.3299404806269776169, 0.3333333333333333703, 0.3299404806269776169, 0.3333333333333333703, 0.3299404806269776169, 0.3333333333333333703, 0.3299404806269776169, 0.3333333333333333703, 0.3299404806269776169, 0.3333333333333333703, 0.3299404806269776169, 0.3333333333333333703, 0.3299404806269776169, 0.3333333333333333703, 0.3299404806269776169, 0.3333333333333333703, 0.3299404806269776169, 0.3333333333333333703, 0.3299404806269776169, 0.3333333333333333703, 0.3299404806269776169, 0.3333333333333333703, 0.3299404806269776169, 0.3333333333333333703, 0.3299404806269776169, 0.3333333333333333703, 0.3299404806269776169, 0.3333333333333333703, 0.3299404806269776169, 0.3333333333333333703, 0.3299404806269776169, 0.3333333333333333703, 0.3299404806269776169, 0.3333333333333333703, 0.3299404806269776169, 0.3333333333333333703, 0.3299404806269776169, 0.3333333333333333703, 0.3299404806269776169, 0.3333333333333333703, 0.3299404806269776169, 0.3333333333333333703, 0.3299404806269776169, 0.3333333333333333703, 0.3299404806269776169, 0.3333333333333333703, 0.3299404806269776169, 0.3333333333333333703, 0.3299404806269776169, 0.3333333333333333703, 0.3299404806269776169, 0.3333333333333333703, 0.3299404806269776169, 0.3333333333333333703, 0.3299404806269776169, 0.3333333333333333703, 0.3299404806269776169, 0.3333333333333333703, 0.3299404806269776169, 0.3333333333333333703, 0.3299404806269776169, 0.3333333333333333703, 0.3299404806269776169, 0.3333333333333333703, 0.3299404806269776169, 0.3333333333333333703, 0.3299404806269776169, 0.3333333333333333703, 0.3299404806269776169, 0.3333333333333333703, 0.3299404806269776169, 0.3333333333333333703, 0.3299404806269776169, 0.3333333333333333703, 0.3299404806269776169, 0.3333333333333333703, 0.3320603117974822438, 0.3317425830320511193),
 ( 1.000000000000000000, 0.9898214418809326842, 1.000000000000000000, 0.9898214418809326842, 1.000000000000000000, 0.9898214418809326842, 1.000000000000000000, 0.9898214418809326842, 1.000000000000000000, 0.9898214418809326842, 1.000000000000000000, 0.9898214418809326842, 1.000000000000000000, 0.9898214418809326842, 1.000000000000000000, 0.9898214418809326842, 1.000000000000000000, 0.9898214418809326842, 1.000000000000000000, 0.9898214418809326842, 1.000000000000000000, 0.9898214418809326842, 1.000000000000000000, 0.9898214418809326842, 1.000000000000000000, 0.9898214418809326842, 1.000000000000000000, 0.9898214418809326842, 1.000000000000000000, 0.9898214418809326842, 1.000000000000000000, 0.9898214418809326842, 1.000000000000000000, 0.9898214418809326842, 1.000000000000000000, 0.9898214418809326842, 1.000000000000000000, 0.9898214418809326842, 1.000000000000000000, 0.9898214418809326842, 1.000000000000000000, 0.9898214418809326842, 1.000000000000000000, 0.9898214418809326842, 1.000000000000000000, 0.9898214418809326842, 1.000000000000000000, 0.9898214418809326842, 1.000000000000000000, 0.9898214418809326842, 1.000000000000000000, 0.9898214418809326842, 1.000000000000000000, 0.9898214418809326842, 1.000000000000000000, 0.9898214418809326842, 1.000000000000000000, 0.9898214418809326842, 1.000000000000000000, 0.9898214418809326842, 1.000000000000000000, 0.9898214418809326842, 1.000000000000000000, 0.9898214418809326842, 1.000000000000000000, 0.9898214418809326842, 1.000000000000000000, 0.9898214418809326842, 1.000000000000000000, 0.9898214418809326842, 1.000000000000000000, 0.9898214418809326842, 1.000000000000000000, 0.9898214418809326842, 1.000000000000000000, 0.9898214418809326842, 1.000000000000000000, 0.9898214418809326842, 1.000000000000000000, 0.9898214418809326842, 1.000000000000000000, 0.9898214418809326842, 1.000000000000000000, 0.9898214418809326842, 1.000000000000000000, 0.9898214418809326842, 1.000000000000000000, 0.9898214418809326842, 1.000000000000000000, 0.9898214418809326842, 1.000000000000000000, 0.9898214418809326842, 1.000000000000000000, 0.9898214418809326842, 1.000000000000000000, 0.9898214418809326842, 1.000000000000000000, 0.9898214418809326842, 1.000000000000000000, 0.9898214418809326842, 1.000000000000000000, 0.9898214418809326842, 1.000000000000000000, 0.9898214418809326842, 1.000000000000000000, 0.9898214418809326842, 1.000000000000000000, 0.9898214418809326842, 1.000000000000000000, 0.9898214418809326842, 1.000000000000000000, 0.9898214418809326842, 1.000000000000000000, 0.9898214418809326842, 1.000000000000000000, 0.9898214418809326842, 1.000000000000000000, 0.9898214418809326842, 1.000000000000000000, 0.9898214418809326842, 1.000000000000000000, 0.9898214418809326842, 1.000000000000000000, 0.9898214418809326842, 1.000000000000000000, 0.9898214418809326842, 1.000000000000000000, 0.9898214418809326842, 1.000000000000000000, 0.9898214418809326842, 1.000000000000000000, 0.9898214418809326842, 1.000000000000000000, 0.9898214418809326842, 1.000000000000000000, 0.9898214418809326842, 1.000000000000000000, 0.9898214418809326842, 1.000000000000000000, 0.9898214418809326842, 1.000000000000000000, 0.9898214418809326842, 1.000000000000000000, 0.9898214418809326842, 1.000000000000000000, 0.9898214418809326842, 1.000000000000000000, 0.9898214418809326842, 1.000000000000000000, 0.9898214418809326842, 1.000000000000000000, 0.9898214418809326842, 1.000000000000000000, 0.9898214418809326842, 1.000000000000000000, 0.9898214418809326842, 1.000000000000000000, 0.9898214418809326842, 1.000000000000000000, 0.9898214418809326842, 1.000000000000000000, 0.9898214418809326842, 1.000000000000000000, 0.9898214418809326842, 1.000000000000000000, 0.9898214418809326842, 1.000000000000000000, 0.9898214418809326842, 1.000000000000000000, 0.9898214418809326842, 1.000000000000000000, 0.9898214418809326842, 1.000000000000000000, 0.9898214418809326842, 1.000000000000000000, 0.9898214418809326842, 1.000000000000000000, 0.9898214418809326842, 1.000000000000000000, 0.9898214418809326842, 1.000000000000000000, 0.9898214418809326842, 1.000000000000000000, 0.9898214418809326842, 1.000000000000000000, 0.9898214418809326842, 1.000000000000000000, 0.9898214418809326842, 1.000000000000000000, 0.9898214418809326842, 1.000000000000000000, 0.9898214418809326842, 1.000000000000000000, 0.9898214418809326842, 1.000000000000000000, 0.9898214418809326842, 1.000000000000000000, 0.9898214418809326842, 1.000000000000000000, 0.9898214418809326842, 1.000000000000000000, 0.9898214418809326842, 1.000000000000000000, 0.9898214418809326842, 1.000000000000000000, 0.9898214418809326842, 1.000000000000000000, 0.9898214418809326842, 1.000000000000000000, 0.9898214418809326842, 1.000000000000000000, 0.9898214418809326842, 1.000000000000000000, 0.9898214418809326842, 1.000000000000000000, 0.9898214418809326842, 1.000000000000000000, 0.9898214418809326842, 1.000000000000000000, 0.9898214418809326842, 1.000000000000000000, 0.9898214418809326842, 1.000000000000000000, 0.9898214418809326842, 1.000000000000000000, 0.9898214418809326842, 1.000000000000000000, 0.9898214418809326842, 1.000000000000000000, 0.9898214418809326842, 1.000000000000000000, 0.9898214418809326842, 1.000000000000000000, 0.9898214418809326842, 1.000000000000000000, 0.9898214418809326842, 1.000000000000000000, 0.9898214418809326842, 1.000000000000000000, 0.9898214418809326842, 1.000000000000000000, 0.9898214418809326842, 1.000000000000000000, 0.9898214418809326842, 1.000000000000000000, 0.9898214418809326842, 1.000000000000000000, 0.9898214418809326842, 1.000000000000000000, 0.9898214418809326842, 1.000000000000000000, 0.9898214418809326842, 1.000000000000000000, 0.9898214418809326842, 1.000000000000000000, 0.9898214418809326842, 1.000000000000000000, 0.9898214418809326842, 1.000000000000000000, 0.9898214418809326842, 1.000000000000000000, 0.9898214418809326842, 1.000000000000000000, 0.9898214418809326842, 1.000000000000000000, 0.9898214418809326842, 1.000000000000000000, 0.9898214418809326842, 1.000000000000000000, 0.9898214418809326842, 1.000000000000000000, 0.9898214418809326842, 1.000000000000000000, 0.9898214418809326842, 1.000000000000000000, 0.9898214418809326842, 1.000000000000000000, 0.9898214418809326842, 1.000000000000000000, 0.9898214418809326842, 1.000000000000000000, 0.9898214418809326842, 1.000000000000000000, 0.9898214418809326842, 1.000000000000000000, 0.9898214418809326842, 1.000000000000000000, 0.9898214418809326842, 1.000000000000000000, 0.9898214418809326842, 1.000000000000000000, 0.9898214418809326842, 1.000000000000000000, 0.9898214418809326842, 1.000000000000000000, 0.9898214418809326842, 1.000000000000000000, 0.9898214418809326842, 1.000000000000000000, 0.9898214418809326842, 1.000000000000000000, 0.9898214418809326842, 1.000000000000000000, 0.9898214418809326842, 1.000000000000000000, 0.9898214418809326842, 1.000000000000000000, 0.9898214418809326842, 1.000000000000000000, 0.9898214418809326842, 1.000000000000000000, 0.9898214418809326842, 1.000000000000000000, 0.9898214418809326842, 1.000000000000000000, 0.9898214418809326842, 1.000000000000000000, 0.9898214418809326842, 1.000000000000000000, 0.9898214418809326842, 1.000000000000000000, 0.9898214418809326842, 1.000000000000000000, 0.9898214418809326842, 1.000000000000000000, 0.9898214418809326842, 1.000000000000000000, 0.9898214418809326842, 1.000000000000000000, 0.9898214418809326842, 1.000000000000000000, 0.9898214418809326842, 1.000000000000000000, 0.9898214418809326842, 1.000000000000000000, 0.9898214418809326842, 1.000000000000000000, 0.9898214418809326842, 1.000000000000000000, 0.9898214418809326842, 1.000000000000000000, 0.9898214418809326842, 1.000000000000000000, 0.9898214418809326842, 1.000000000000000000, 0.9898214418809326842, 1.000000000000000000, 0.9898214418809326842, 1.000000000000000000, 0.9898214418809326842, 1.000000000000000000, 0.9898214418809326842, 1.000000000000000000, 0.9898214418809326842, 1.000000000000000000, 0.9898214418809326842, 1.000000000000000000, 0.9898214418809326842, 1.000000000000000000, 0.9898214418809326842, 1.000000000000000000, 0.9898214418809326842, 1.000000000000000000, 0.9898214418809326842, 1.000000000000000000, 0.9898214418809326842, 1.000000000000000000, 0.9898214418809326842, 1.000000000000000000, 0.9898214418809326842, 1.000000000000000000, 0.9898214418809326842, 1.000000000000000000, 0.9898214418809326842, 1.000000000000000000, 0.9898214418809326842, 1.000000000000000000, 0.9898214418809326842, 1.000000000000000000, 0.9898214418809326842, 1.000000000000000000, 0.9898214418809326842, 1.000000000000000000, 0.9898214418809326842, 1.000000000000000000, 0.9898214418809326842, 1.000000000000000000, 0.9898214418809326842, 1.000000000000000000, 0.9898214418809326842, 1.000000000000000000, 0.9898214418809326842, 1.000000000000000000, 0.9898214418809326842, 1.000000000000000000, 0.9898214418809326842, 1.000000000000000000, 0.9898214418809326842, 1.000000000000000000, 0.9898214418809326842, 1.000000000000000000, 0.9898214418809326842, 1.000000000000000000, 0.9898214418809326842, 1.000000000000000000, 0.9898214418809326842, 1.000000000000000000, 0.9898214418809326842, 1.000000000000000000, 0.9898214418809326842, 1.000000000000000000, 0.9898214418809326842, 1.000000000000000000, 0.9898214418809326842, 1.000000000000000000, 0.9898214418809326842, 1.000000000000000000, 0.9898214418809326842, 1.000000000000000000, 0.9898214418809326842, 1.000000000000000000, 0.9898214418809326842, 1.000000000000000000, 0.9898214418809326842, 1.000000000000000000, 0.9898214418809326842, 1.000000000000000000, 0.9898214418809326842, 1.000000000000000000, 0.9898214418809326842, 1.000000000000000000, 0.9898214418809326842, 1.000000000000000000, 0.9898214418809326842, 1.000000000000000000, 0.9898214418809326842, 1.000000000000000000, 0.9898214418809326842, 1.000000000000000000, 0.9898214418809326842, 1.000000000000000000, 0.9898214418809326842, 1.000000000000000000, 0.9898214418809326842, 1.000000000000000000, 0.9898214418809326842, 1.000000000000000000, 0.9898214418809326842, 1.000000000000000000, 0.9898214418809326842, 1.000000000000000000, 0.9898214418809326842, 1.000000000000000000, 0.9898214418809326842, 1.000000000000000000, 0.9898214418809326842, 1.000000000000000000, 0.9898214418809326842, 1.000000000000000000, 0.9898214418809326842, 1.000000000000000000, 0.9898214418809326842, 1.000000000000000000, 0.9898214418809326842, 1.000000000000000000, 0.9898214418809326842, 1.000000000000000000, 0.9898214418809326842, 1.000000000000000000, 0.9898214418809326842, 1.000000000000000000, 0.9898214418809326842, 1.000000000000000000, 0.9898214418809326842, 1.000000000000000000, 0.9898214418809326842, 1.000000000000000000, 0.9898214418809326842, 1.000000000000000000, 0.9898214418809326842, 1.000000000000000000, 0.9898214418809326842, 1.000000000000000000, 0.9898214418809326842, 1.000000000000000000, 0.9898214418809326842, 1.000000000000000000, 0.9898214418809326842, 1.000000000000000000, 0.9898214418809326842, 1.000000000000000000, 0.9898214418809326842, 1.000000000000000000, 0.9898214418809326842, 1.000000000000000000, 0.9898214418809326842, 1.000000000000000000, 0.9898214418809326842, 1.000000000000000000, 0.9898214418809326842, 1.000000000000000000, 0.9898214418809326842, 1.000000000000000000, 0.9898214418809326842, 1.000000000000000000, 0.9898214418809326842, 1.000000000000000000, 0.9898214418809326842, 1.000000000000000000, 0.9898214418809326842, 1.000000000000000000, 0.9898214418809326842, 1.000000000000000000, 0.9898214418809326842, 1.000000000000000000, 0.9898214418809326842, 1.000000000000000000, 0.9898214418809326842, 1.000000000000000000, 0.9898214418809326842, 1.000000000000000000, 0.9898214418809326842, 1.000000000000000000, 0.9898214418809326842, 1.000000000000000000, 0.9898214418809326842, 1.000000000000000000, 0.9898214418809326842, 1.000000000000000000, 0.9898214418809326842, 1.000000000000000000, 0.9898214418809326842, 1.000000000000000000, 0.9898214418809326842, 1.000000000000000000, 0.9898214418809326842, 1.000000000000000000, 0.9898214418809326842, 1.000000000000000000, 0.9898214418809326842, 1.000000000000000000, 0.9898214418809326842, 1.000000000000000000, 0.9898214418809326842, 1.000000000000000000, 0.9898214418809326842, 1.000000000000000000, 0.9898214418809326842, 1.000000000000000000, 0.9898214418809326842, 1.000000000000000000, 0.9898214418809326842, 1.000000000000000000, 0.9898214418809326842, 1.000000000000000000, 0.9898214418809326842, 1.000000000000000000, 0.9898214418809326842, 1.000000000000000000, 0.9898214418809326842, 1.000000000000000000, 0.9898214418809326842, 1.000000000000000000, 0.9898214418809326842, 1.000000000000000000, 0.9898214418809326842, 1.000000000000000000, 0.9898214418809326842, 1.000000000000000000, 0.9898214418809326842, 1.000000000000000000, 0.9898214418809326842, 1.000000000000000000, 0.9898214418809326842, 1.000000000000000000, 0.9898214418809326842, 1.000000000000000000, 0.9898214418809326842, 1.000000000000000000, 0.9898214418809326842, 1.000000000000000000, 0.9898214418809326842, 1.000000000000000000, 0.9898214418809326842, 1.000000000000000000, 0.9898214418809326842, 1.000000000000000000, 0.9898214418809326842, 1.000000000000000000, 0.9898214418809326842, 1.000000000000000000, 0.9898214418809326842, 1.000000000000000000, 0.9898214418809326842, 1.000000000000000000, 0.9898214418809326842, 1.000000000000000000, 0.9898214418809326842, 1.000000000000000000, 0.9898214418809326842, 1.000000000000000000, 0.9898214418809326842, 1.000000000000000000, 0.9898214418809326842, 1.000000000000000000, 0.9898214418809326842, 1.000000000000000000, 0.9898214418809326842, 1.000000000000000000, 0.9898214418809326842, 1.000000000000000000, 0.9898214418809326842, 1.000000000000000000, 0.9898214418809326842, 1.000000000000000000, 0.9898214418809326842, 1.000000000000000000, 0.9898214418809326842, 1.000000000000000000, 0.9898214418809326842, 1.000000000000000000, 0.9898214418809326842, 1.000000000000000000, 0.9898214418809326842, 1.000000000000000000, 0.9898214418809326842, 1.000000000000000000, 0.9898214418809326842, 1.000000000000000000, 0.9898214418809326842, 1.000000000000000000, 0.9898214418809326842, 1.000000000000000000, 0.9898214418809326842, 1.000000000000000000, 0.9898214418809326842, 1.000000000000000000, 0.9898214418809326842, 1.000000000000000000, 0.9898214418809326842, 1.000000000000000000, 0.9898214418809326842, 1.000000000000000000, 0.9898214418809326842, 1.000000000000000000, 0.9898214418809326842, 1.000000000000000000, 0.9898214418809326842, 1.000000000000000000, 0.9898214418809326842, 1.000000000000000000, 0.9898214418809326842, 1.000000000000000000, 0.9898214418809326842, 1.000000000000000000, 0.9898214418809326842, 1.000000000000000000, 0.9898214418809326842, 1.000000000000000000, 0.9898214418809326842, 1.000000000000000000, 0.9898214418809326842, 1.000000000000000000, 0.9898214418809326842, 1.000000000000000000, 0.9898214418809326842, 1.000000000000000000, 0.9898214418809326842, 1.000000000000000000, 0.9898214418809326842, 1.000000000000000000, 0.9898214418809326842, 1.000000000000000000, 0.9898214418809326842, 1.000000000000000000, 0.9898214418809326842, 1.000000000000000000, 0.9898214418809326842, 1.000000000000000000, 0.9898214418809326842, 1.000000000000000000, 0.9898214418809326842, 1.000000000000000000, 0.9898214418809326842, 1.000000000000000000, 0.9898214418809326842, 1.000000000000000000, 0.9898214418809326842, 1.000000000000000000, 0.9898214418809326842, 1.000000000000000000, 0.9898214418809326842, 1.000000000000000000, 0.9898214418809326842, 1.000000000000000000, 0.9898214418809326842, 1.000000000000000000, 0.9898214418809326842, 1.000000000000000000, 0.9898214418809326842, 1.000000000000000000, 0.9898214418809326842, 1.000000000000000000, 0.9898214418809326842, 1.000000000000000000, 0.9898214418809326842, 1.000000000000000000, 0.9898214418809326842, 1.000000000000000000, 0.9898214418809326842, 1.000000000000000000, 0.9898214418809326842, 1.000000000000000000, 0.9898214418809326842, 1.000000000000000000, 0.9898214418809326842, 1.000000000000000000, 0.9898214418809326842, 1.000000000000000000, 0.9898214418809326842, 1.000000000000000000, 0.9898214418809326842, 1.000000000000000000, 0.9898214418809326842, 1.000000000000000000, 0.9898214418809326842, 1.000000000000000000, 0.9898214418809326842, 1.000000000000000000, 0.9898214418809326842, 1.000000000000000000, 0.9898214418809326842, 1.000000000000000000, 0.9898214418809326842, 1.000000000000000000, 0.9898214418809326842, 1.000000000000000000, 0.9898214418809326842, 1.000000000000000000, 0.9898214418809326842, 1.000000000000000000, 0.9898214418809326842, 1.000000000000000000, 0.9898214418809326842, 1.000000000000000000, 0.9898214418809326842, 1.000000000000000000, 0.9898214418809326842, 1.000000000000000000, 0.9898214418809326842, 1.000000000000000000, 0.9898214418809326842, 1.000000000000000000, 0.9898214418809326842, 1.000000000000000000, 0.9898214418809326842, 1.000000000000000000, 0.9898214418809326842, 1.000000000000000000, 0.9898214418809326842, 1.000000000000000000, 0.9898214418809326842, 1.000000000000000000, 0.9898214418809326842, 1.000000000000000000, 0.9898214418809326842, 1.000000000000000000, 0.9898214418809326842, 1.000000000000000000, 0.9898214418809326842, 1.000000000000000000, 0.9898214418809326842, 1.000000000000000000, 0.9898214418809326842, 1.000000000000000000, 0.9898214418809326842, 1.000000000000000000, 0.9898214418809326842, 1.000000000000000000, 0.9898214418809326842, 1.000000000000000000, 0.9898214418809326842, 1.000000000000000000, 0.9898214418809326842, 1.000000000000000000, 0.9898214418809326842, 1.000000000000000000, 0.9898214418809326842, 1.000000000000000000, 0.9898214418809326842, 1.000000000000000000, 0.9898214418809326842, 1.000000000000000000, 0.9898214418809326842, 1.000000000000000000, 0.9898214418809326842, 1.000000000000000000, 0.9898214418809326842, 1.000000000000000000, 0.9898214418809326842, 1.000000000000000000, 0.9898214418809326842, 1.000000000000000000, 0.9898214418809326842, 1.000000000000000000, 0.9898214418809326842, 1.000000000000000000, 0.9898214418809326842, 1.000000000000000000, 0.9898214418809326842, 1.000000000000000000, 0.9898214418809326842, 1.000000000000000000, 0.9898214418809326842, 1.000000000000000000, 0.9898214418809326842, 1.000000000000000000, 0.9898214418809326842, 1.000000000000000000, 0.9898214418809326842, 1.000000000000000000, 0.9898214418809326842, 1.000000000000000000, 0.9898214418809326842, 1.000000000000000000, 0.9898214418809326842, 1.000000000000000000, 0.9898214418809326842, 1.000000000000000000, 0.9898214418809326842, 1.000000000000000000, 0.9898214418809326842, 1.000000000000000000, 0.9898214418809326842, 1.000000000000000000, 0.9898214418809326842, 1.000000000000000000, 0.9898214418809326842, 1.000000000000000000, 0.9898214418809326842, 1.000000000000000000, 0.9898214418809326842, 1.000000000000000000, 0.9898214418809326842, 1.000000000000000000, 0.9898214418809326842, 1.000000000000000000, 0.9898214418809326842, 1.000000000000000000, 0.9898214418809326842, 1.000000000000000000, 0.9898214418809326842, 1.000000000000000000, 0.9898214418809326842, 1.000000000000000000, 0.9898214418809326842, 1.000000000000000000, 0.9898214418809326842, 1.000000000000000000, 0.9898214418809326842, 1.000000000000000000, 0.9961809353924466759, 0.9952277490961531914) ) ) 
 REPRESENTATION_ITEM ( '' )  SURFACE ( )  );
#36827 = CARTESIAN_POINT ( 'NONE',  ( 744.7301800767019131, -244.8164208402378961, 337.4774526936615757 ) ) ;
#36828 = CARTESIAN_POINT ( 'NONE',  ( 775.9200461376533440, -167.8055962898689586, 315.3028492785443291 ) ) ;
#36830 = DIRECTION ( 'NONE',  ( 0.000000000000000000, 0.7071067811865578978, 0.7071067811865372477 ) ) ;
#36829 = CARTESIAN_POINT ( 'NONE',  ( 762.3223304703356007, 16.45630643248849267, -322.3223304703362828 ) ) ;
#36831 = VERTEX_POINT ( 'NONE', #25989 ) ;
#36832 = CARTESIAN_POINT ( 'NONE',  ( 802.9823548866075953, -433.0999726633339151, -330.0799878456151077 ) ) ;
#36833 = DIRECTION ( 'NONE',  ( 1.000000000000000000, 0.000000000000000000, 0.000000000000000000 ) ) ;
#36834 = CARTESIAN_POINT ( 'NONE',  ( 805.6418435158337843, -197.4636090269709996, -363.8556311672236916 ) ) ;
#36835 = CARTESIAN_POINT ( 'NONE',  ( 745.7194118038753459, -61.64542720878961291, 348.7631598425976449 ) ) ;
#36837 = CARTESIAN_POINT ( 'NONE',  ( 803.6646147819161570, -185.9073299311472454, -348.8264449731210561 ) ) ;
#36836 = CARTESIAN_POINT ( 'NONE',  ( 180.7583438952258348, 394.6698570112193920, -274.9999999999999432 ) ) ;
#36838 = EDGE_CURVE ( 'NONE', #22371, #6808, #27947, .T. ) ;
#36839 = CARTESIAN_POINT ( 'NONE',  ( 790.8726784830453198, -346.7146871989592682, -362.5472867521010585 ) ) ;
#36840 = CARTESIAN_POINT ( 'NONE',  ( 799.9999999999993179, -462.9681489794448339, -309.9999999999998863 ) ) ;
#36841 = SHAPE_REPRESENTATION ( 'Upper Moving Shear Blade Bar', ( #26858 ), #29006 ) ;
#36842 = CARTESIAN_POINT ( 'NONE',  ( 781.2370466360911223, -212.7363362996982232, -304.9990715423533629 ) ) ;
#36843 = DIRECTION ( 'NONE',  ( 1.000000000000000000, 0.000000000000000000, 0.000000000000000000 ) ) ;
#36844 = DIRECTION ( 'NONE',  ( 0.000000000000000000, -0.7517448203044211352, -0.6594541114781782287 ) ) ;
#36845 = CARTESIAN_POINT ( 'NONE',  ( 783.0745993439762742, -56.19088175424417386, -365.1016975059196739 ) ) ;
#36846 = CARTESIAN_POINT ( 'NONE',  ( 779.4763451958990572, -416.7363362996975980, 365.0264073115438919 ) ) ;
#36847 = EDGE_CURVE ( 'NONE', #9644, #6307, #36784, .T. ) ;
#36848 = CARTESIAN_POINT ( 'NONE',  ( 814.5518280994195948, -231.7255117493288594, -332.4837098697145166 ) ) ;
#36849 = CARTESIAN_POINT ( 'NONE',  ( 779.9999999999997726, 16.45630643248849267, -339.9999999999994884 ) ) ;
#36850 = CARTESIAN_POINT ( 'NONE',  ( 755.5713283507202505, -29.36187538569318178, -334.6858677611754729 ) ) ;
#36851 = VECTOR ( 'NONE', #3561, 1000.000000000000000 ) ;
#36852 = CARTESIAN_POINT ( 'NONE',  ( 815.3608509340175488, -194.7363362996982517, 341.2497674668889545 ) ) ;
#36853 = CARTESIAN_POINT ( 'NONE',  ( 798.0661480581538854, -146.5328690171417350, -309.5768839229118043 ) ) ;
#36854 = CARTESIAN_POINT ( 'NONE',  ( 801.1904061080336987, -140.0891481129654892, 368.3070685750235498 ) ) ;
#36855 = CARTESIAN_POINT ( 'NONE',  ( 745.7998596910086917, -389.3618753856919739, -332.5602148656461168 ) ) ;
#36856 = ADVANCED_FACE ( 'NONE', ( #30533 ), #27307, .F. ) ;
#36857 = CARTESIAN_POINT ( 'NONE',  ( -26.63011601220122060, -513.1383975375929367, -369.9999999999999432 ) ) ;
#36858 = CARTESIAN_POINT ( 'NONE',  ( 764.8639956371174549, -272.0891481129651197, 319.7806653035542013 ) ) ;
#36859 = CARTESIAN_POINT ( 'NONE',  ( 775.8780910478218402, -33.28179084515333130, 364.9511171171680530 ) ) ;
#36860 = CARTESIAN_POINT ( 'NONE',  ( 804.6798772138708955, -375.7255117493283478, -334.6312213355107019 ) ) ;
#36861 = DIRECTION ( 'NONE',  ( 0.000000000000000000, -0.000000000000000000, 1.000000000000000000 ) ) ;
#36862 = CARTESIAN_POINT ( 'NONE',  ( 814.2001403089898304, -449.3618753856918602, -347.4397851343538264 ) ) ;
#36863 = LINE ( 'NONE', #2426, #18110 ) ;
#36864 = CARTESIAN_POINT ( 'NONE',  ( 789.9200121543843807, -97.98741447168734453, 317.0176451133914384 ) ) ;
#36865 = EDGE_LOOP ( 'NONE', ( #4555, #17851 ) ) ;
#36866 = CARTESIAN_POINT ( 'NONE',  ( 754.8072714833581358, -268.8164208402378108, 338.1981804954720587 ) ) ;
#36867 = CARTESIAN_POINT ( 'NONE',  ( 754.9735926884551418, -210.3510508353233490, -340.5236548041000333 ) ) ;
#36868 = CARTESIAN_POINT ( 'NONE',  ( 755.3201227861273992, -51.72551174932946338, 345.3687786644892981 ) ) ;
#36869 = CARTESIAN_POINT ( 'NONE',  ( 801.9858362298568863, -219.0783235625960401, -312.7379699480935642 ) ) ;
#36870 = DIRECTION ( 'NONE',  ( -0.000000000000000000, -1.000000000000000000, -0.000000000000000000 ) ) ;
#36871 = CARTESIAN_POINT ( 'NONE',  ( 773.7943932421234194, -335.8055962898683902, 305.5313806188329409 ) ) ;
#36872 = ORIENTED_EDGE ( 'NONE', *, *, #12533, .T. ) ;
#36873 = CARTESIAN_POINT ( 'NONE',  ( 813.2346286133761168, -437.2601417444135450, 328.9521613784389160 ) ) ;
#36874 = EDGE_CURVE ( 'NONE', #9279, #5066, #19832, .T. ) ;
#36875 = CARTESIAN_POINT ( 'NONE',  ( 774.6858677611749044, -153.7255117493291721, -315.5713283507209894 ) ) ;
#36876 = CARTESIAN_POINT ( 'NONE',  ( 781.7834795799800531, -346.8164208402376971, 315.0636971347436202 ) ) ;
#36877 = CARTESIAN_POINT ( 'NONE',  ( 796.9462024416508257, -84.45278447660206211, -308.9653473494370246 ) ) ;
#36878 = CARTESIAN_POINT ( 'NONE',  ( 794.9819416627830151, -60.99823902205671544, -319.9864689768909898 ) ) ;
#36879 = ORIENTED_EDGE ( 'NONE', *, *, #20712, .F. ) ;
#36880 = CARTESIAN_POINT ( 'NONE',  ( 773.4516893846965786, 4.354572791210176597, -315.8398074228977066 ) ) ;
#36881 = ORIENTED_EDGE ( 'NONE', *, *, #36894, .F. ) ;
#36882 = CARTESIAN_POINT ( 'NONE',  ( 775.8780910478218402, -321.2817908451525000, -364.9511171171680530 ) ) ;
#36884 = CARTESIAN_POINT ( 'NONE',  ( 804.1105419155481968, -363.8272453906068336, 347.6308680596136469 ) ) ;
#36883 = CARTESIAN_POINT ( 'NONE',  ( 762.3223304703356007, -103.5436935675111272, 322.3223304703362828 ) ) ;
#36887 = CARTESIAN_POINT ( 'NONE',  ( 744.9990715423526808, -306.3510508353230648, 341.2370466360926002 ) ) ;
#36886 = DIRECTION ( 'NONE',  ( -0.000000000000000000, 1.000000000000000000, -0.000000000000000000 ) ) ;
#36885 = CARTESIAN_POINT ( 'NONE',  ( 782.5225473063383106, -430.2709662947827383, 375.2698199232970637 ) ) ;
#36888 = CARTESIAN_POINT ( 'NONE',  ( 786.2056067578752163, -107.8055962898691433, 374.4686193811670023 ) ) ;
#36889 = CARTESIAN_POINT ( 'NONE',  ( 766.0291762391763086, -322.9181544815161260, -360.7704444035551319 ) ) ;
#36890 = CARTESIAN_POINT ( 'NONE',  ( 800.2193346964447755, -138.9982390220563957, -355.1360043628815788 ) ) ;
#36891 = CARTESIAN_POINT ( 'NONE',  ( 745.0891759886404770, -436.2709662947827951, 342.4968714119734159 ) ) ;
#36893 = CARTESIAN_POINT ( 'NONE',  ( 772.4999999999993179, -512.9681489794448908, -309.9999999999998863 ) ) ;
#36892 = LINE ( 'NONE', #5462, #12305 ) ;
#36894 = EDGE_CURVE ( 'NONE', #32406, #23058, #22052, .T. ) ;
#36895 = CARTESIAN_POINT ( 'NONE',  ( -78.83651009197140525, 260.0000000000000568, -206.1189999999936049 ) ) ;
#36896 = CARTESIAN_POINT ( 'NONE',  ( 989.9999999999992042, -407.8586036264140375, 201.9999999999998863 ) ) ;
#36897 = CARTESIAN_POINT ( 'NONE',  ( 802.9823548866075953, -313.0999726633342561, 330.0799878456151077 ) ) ;
#36898 = CARTESIAN_POINT ( 'NONE',  ( 803.6646147819161570, -185.9073299311472454, 348.8264449731210561 ) ) ;
#36899 = ORIENTED_EDGE ( 'NONE', *, *, #7510, .F. ) ;
#36900 = CARTESIAN_POINT ( 'NONE',  ( 792.2312462859673587, -131.9073299311473875, -307.2067596250082602 ) ) ;
#36901 = CYLINDRICAL_SURFACE ( 'NONE', #1703, 30.00000000000002842 ) ;
#36902 = CARTESIAN_POINT ( 'NONE',  ( 764.1737431748507561, -58.37269993606236085, 371.6461892240376415 ) ) ;
#36903 = CARTESIAN_POINT ( 'NONE',  ( 754.9967657858570647, -265.5436935675106156, -365.0032342141425374 ) ) ;
#36904 = FACE_BOUND ( 'NONE', #44910, .T. ) ;
#36905 = CARTESIAN_POINT ( 'NONE',  ( 800.2193346964447755, -138.9982390220563957, 355.1360043628815788 ) ) ;
#36906 = CARTESIAN_POINT ( 'NONE',  ( 751.2241431872005251, -352.1692326535046504, -359.9636004259367610 ) ) ;
#36907 = CARTESIAN_POINT ( 'NONE',  ( 772.5602148656447525, -81.72551174932937101, -305.7998596910095443 ) ) ;
#36908 = CARTESIAN_POINT ( 'NONE',  ( 754.7162404726377645, -14.73633629969885384, 339.4709603349214717 ) ) ;
#36909 = CARTESIAN_POINT ( 'NONE',  ( 782.4968714119720516, -346.8164208402376971, -305.0891759886411023 ) ) ;
#36910 = DIRECTION ( 'NONE',  ( -1.000000000000000000, -0.000000000000000000, -0.000000000000000000 ) ) ;
#36911 = CARTESIAN_POINT ( 'NONE',  ( 793.2243759319678702, -410.5328690171408539, 318.4439275373583200 ) ) ;
#36912 = EDGE_LOOP ( 'NONE', ( #5446, #13872, #16940, #13786, #36938, #10235, #35860, #30331, #38080, #26639, #18019, #11769 ) ) ;
#36913 = CARTESIAN_POINT ( 'NONE',  ( 793.2243759319678702, -74.53286901714196233, 318.4439275373583200 ) ) ;
#36914 = CARTESIAN_POINT ( 'NONE',  ( 785.3141322388236176, -213.7255117493289731, -364.4286716492789537 ) ) ;
#36915 = CARTESIAN_POINT ( 'NONE',  ( 810.1134526219336749, -128.5328690171417634, -357.8822607201570349 ) ) ;
#36916 = CARTESIAN_POINT ( 'NONE',  ( 794.9999999999993179, 205.0000000000000568, 255.0000000000000000 ) ) ;
#36917 = CARTESIAN_POINT ( 'NONE',  ( 793.4146539503750546, -241.9874144716869182, 307.6481478633938877 ) ) ;
#36918 = CARTESIAN_POINT ( 'NONE',  ( 788.7366044899766848, -83.90732993114754379, 316.5762568750059813 ) ) ;
#36919 = EDGE_LOOP ( 'NONE', ( #24028, #34496 ) ) ;
#36920 = VERTEX_POINT ( 'NONE', #5836 ) ;
#36921 = CARTESIAN_POINT ( 'NONE',  ( 803.2186876482843445, -223.9874144716869182, -350.0220218866286928 ) ) ;
#36922 = CARTESIAN_POINT ( 'NONE',  ( 785.3141322388236176, -237.7255117493289163, 364.4286716492789537 ) ) ;
#36923 = CARTESIAN_POINT ( 'NONE',  ( 755.2512626584698410, 16.45630643248849267, -315.2512626584710915 ) ) ;
#36924 = CARTESIAN_POINT ( 'NONE',  ( 746.7653713866222915, -65.26014174441471027, -351.0478386215610271 ) ) ;
#36925 = DIRECTION ( 'NONE',  ( 0.000000000000000000, -0.000000000000000000, -1.000000000000000000 ) ) ;
#36926 = ORIENTED_EDGE ( 'NONE', *, *, #14579, .F. ) ;
#36927 = ORIENTED_EDGE ( 'NONE', *, *, #27798, .F. ) ;
#36928 = CARTESIAN_POINT ( 'NONE',  ( 744.6391490659812007, -374.7363362996978253, -338.7502325331110455 ) ) ;
#36929 = CARTESIAN_POINT ( 'NONE',  ( 800.2193346964447755, -234.9982390220561683, -355.1360043628815788 ) ) ;
#36930 = CARTESIAN_POINT ( 'NONE',  ( 745.0891759886404770, -340.2709662947831362, 342.4968714119734159 ) ) ;
#36931 = CARTESIAN_POINT ( 'NONE',  ( 747.3154664389472828, -43.98741447168752217, 326.4474001241230781 ) ) ;
#36932 = CARTESIAN_POINT ( 'NONE',  ( 780.5236548040995785, -236.7363362996981380, -314.9735926884559944 ) ) ;
#36933 = CARTESIAN_POINT ( 'NONE',  ( 791.9812246680005501, -212.6346026584198796, -361.9419747391813189 ) ) ;
#36934 = CARTESIAN_POINT ( 'NONE',  ( 771.2633955100217236, -383.9073299311466485, -363.4237431249939618 ) ) ;
#36935 = EDGE_LOOP ( 'NONE', ( #7516, #35525, #44726, #14149 ) ) ;
#36936 = CARTESIAN_POINT ( 'NONE',  ( 771.1735550268778070, -201.1800572038744690, 316.3353852180827630 ) ) ;
#36937 = CARTESIAN_POINT ( 'NONE',  ( 762.3223304703356007, -103.5436935675111272, -322.3223304703362828 ) ) ;
#36938 = ORIENTED_EDGE ( 'NONE', *, *, #36696, .F. ) ;
#36939 = CARTESIAN_POINT ( 'NONE',  ( 811.0346526505616112, -326.6346026584193396, 323.0537975583477532 ) ) ;
#36940 = CARTESIAN_POINT ( 'NONE',  ( 779.9999999999992042, 126.4563064324884465, 339.9999999999999432 ) ) ;
#36941 = CARTESIAN_POINT ( 'NONE',  ( 759.9999999999992042, 205.0000000000000568, -319.9999999999999432 ) ) ;
#36942 = CARTESIAN_POINT ( 'NONE',  ( 187.1337867209877857, 56.73212367640085318, -362.5753187112032379 ) ) ;
#36943 = CARTESIAN_POINT ( 'NONE',  ( 758.4439275373578084, -180.5545181178801499, 353.2243759319684386 ) ) ;
#36944 = CARTESIAN_POINT ( 'NONE',  ( 755.3201227861273992, -75.72551174932937101, 345.3687786644892981 ) ) ;
#36945 = ORIENTED_EDGE ( 'NONE', *, *, #13086, .F. ) ;
#36946 = CARTESIAN_POINT ( 'NONE',  ( 760.0363995740630116, -442.9181544815157849, -368.7758568127991907 ) ) ;
#36947 = CARTESIAN_POINT ( 'NONE',  ( 813.1304606946831655, -17.90732993114776406, -352.3570229623691716 ) ) ;
#36948 = CARTESIAN_POINT ( 'NONE',  ( 754.8983024940795303, -258.8965053807777963, 336.9254006560228163 ) ) ;
#36949 = CARTESIAN_POINT ( 'NONE',  ( 767.8955696845333705, -384.4527844766011526, -362.1676090361162323 ) ) ;
#36950 = CARTESIAN_POINT ( 'NONE',  ( 803.6646147819162707, -17.90732993114776406, -348.8264449731211130 ) ) ;
#36951 = CARTESIAN_POINT ( 'NONE',  ( 804.7487373415286811, -427.5436935675101040, 364.7487373415288516 ) ) ;
#36952 = FACE_BOUND ( 'NONE', #42278, .T. ) ;
#36953 = CARTESIAN_POINT ( 'NONE',  ( 787.5531968255692163, -285.8272453906071178, -316.1348686366205811 ) ) ;
#36954 = CARTESIAN_POINT ( 'NONE',  ( 754.9967657858570647, -169.5436935675108430, -365.0032342141425374 ) ) ;
#36955 = CARTESIAN_POINT ( 'NONE',  ( 814.9108240113580450, -64.27096629478397460, 337.5031285880265273 ) ) ;
#36956 = CARTESIAN_POINT ( 'NONE',  ( 749.2812353651451076, -126.4527844766019626, 323.2262854647983090 ) ) ;
#36957 = CARTESIAN_POINT ( 'NONE',  ( 788.0874520139973356, 16.45630643248838609, -314.0623709945898554 ) ) ;
#36958 = DIRECTION ( 'NONE',  ( -1.000000000000000000, 0.000000000000000000, -0.000000000000000000 ) ) ;
#36959 = LINE ( 'NONE', #19408, #11745 ) ;
#36960 = CARTESIAN_POINT ( 'NONE',  ( 758.8095938919642549, -368.0891481129647786, 311.6929314249763365 ) ) ;
#36961 = CARTESIAN_POINT ( 'NONE',  ( 800.2193346964447755, -330.9982390220558273, -355.1360043628815788 ) ) ;
#36962 = CARTESIAN_POINT ( 'NONE',  ( 755.8398074228967971, 4.558040073766884248, 333.4516893846970333 ) ) ;
#36963 = CARTESIAN_POINT ( 'NONE',  ( 750.9282345327678740, -88.91815448151682233, -319.8311093483690115 ) ) ;
#36964 = CARTESIAN_POINT ( 'NONE',  ( 766.7756240680305382, -134.5328690171417350, -361.5560724626415663 ) ) ;
#36965 = CARTESIAN_POINT ( 'NONE',  ( 800.1688906516307043, -130.1692326535054463, 369.0717654672308186 ) ) ;
#36966 = PLANE ( 'NONE',  #35787 ) ;
#36967 = CARTESIAN_POINT ( 'NONE',  ( 759.8311093483677041, -166.1692326535053041, 310.9282345327691814 ) ) ;
#36968 = CARTESIAN_POINT ( 'NONE',  ( 794.9819416627830151, -12.99823902205686821, -319.9864689768909898 ) ) ;
#36969 = CARTESIAN_POINT ( 'NONE',  ( 765.8855110935204493, -118.1692326535054463, -319.0159684113471599 ) ) ;
#36970 = CARTESIAN_POINT ( 'NONE',  ( 795.1360043628807261, -116.0891481129656029, -360.2193346964456282 ) ) ;
#36971 = CARTESIAN_POINT ( 'NONE',  ( 785.3141322388236176, -141.7255117493291721, 364.4286716492789537 ) ) ;
#36972 = CARTESIAN_POINT ( 'NONE',  ( 784.0799538623451781, -419.8055962898681059, -364.6971507214555572 ) ) ;
#36974 = CARTESIAN_POINT ( 'NONE',  ( 788.8264449731201466, -261.1800572038742416, 363.6646147819170665 ) ) ;
#36973 = CARTESIAN_POINT ( 'NONE',  ( 792.1044303154645831, -276.4527844766013800, 317.8323909638837677 ) ) ;
#36975 = DIRECTION ( 'NONE',  ( 1.000000000000000000, 0.000000000000000000, -0.000000000000000000 ) ) ;
#36976 = ORIENTED_EDGE ( 'NONE', *, *, #5541, .F. ) ;
#36977 = CARTESIAN_POINT ( 'NONE',  ( 760.5453621957607311, 2.921676437403253779, 323.8424801807151425 ) ) ;
#36978 = CARTESIAN_POINT ( 'NONE',  ( 804.1009440267234822, -263.4636090269708006, -314.0944755984392600 ) ) ;
#36979 = ORIENTED_EDGE ( 'NONE', *, *, #20723, .T. ) ;
#36980 = DIRECTION ( 'NONE',  ( -1.000000000000000000, 0.000000000000000000, 0.000000000000000000 ) ) ;
#36981 = CARTESIAN_POINT ( 'NONE',  ( 745.7998596910086917, -221.3618753856925707, 332.5602148656461168 ) ) ;
#36982 = CARTESIAN_POINT ( 'NONE',  ( 804.8461984189677878, -290.1908817542434349, 336.9566956441385628 ) ) ;
#36983 = CARTESIAN_POINT ( 'NONE',  ( 759.2295555964440155, -400.1692326535045936, 353.9708237608231229 ) ) ;
#36984 = VERTEX_POINT ( 'NONE', #33997 ) ;
#36985 = CARTESIAN_POINT ( 'NONE',  ( 766.9102291470427417, -114.5545181178803631, -318.6633372737382501 ) ) ;
#36986 = CARTESIAN_POINT ( 'NONE',  ( 794.9819416627830151, -276.9982390220559978, -319.9864689768909898 ) ) ;
#36987 = ORIENTED_EDGE ( 'NONE', *, *, #26462, .F. ) ;
#36988 = CARTESIAN_POINT ( 'NONE',  ( 754.8072714833581358, -436.8164208402372992, -338.1981804954720587 ) ) ;
#36989 = CARTESIAN_POINT ( 'NONE',  ( 771.1735550268778070, -81.18005720387481006, -316.3353852180827630 ) ) ;
#36990 = CARTESIAN_POINT ( 'NONE',  ( 783.0433043558608688, -288.8965053807775121, 315.1538015810313027 ) ) ;
#36991 = DIRECTION ( 'NONE',  ( -0.000000000000000000, 1.000000000000000000, -0.000000000000000000 ) ) ;
#36992 = CARTESIAN_POINT ( 'NONE',  ( -773.4999999999993179, -494.6608068873671300, -357.6536686473015720 ) ) ;
#36993 = CARTESIAN_POINT ( 'NONE',  ( 795.1360043628807261, 3.910851887033985896, 360.2193346964456282 ) ) ;
#36994 = ORIENTED_EDGE ( 'NONE', *, *, #20363, .T. ) ;
#36995 = CARTESIAN_POINT ( 'NONE',  ( 810.4231160770870019, -336.5545181178796952, -321.9338519418446936 ) ) ;
#36996 = CARTESIAN_POINT ( 'NONE',  ( 745.1792804349281596, -206.1908817542437191, 343.7566961878542884 ) ) ;
#36998 = CARTESIAN_POINT ( 'NONE',  ( 759.9864689768902508, -290.0891481129650629, -354.9819416627836404 ) ) ;
#36997 = CARTESIAN_POINT ( 'NONE',  ( -879.9999999999992042, 579.9999999999998863, -320.0000000000000000 ) ) ;
#36999 = CARTESIAN_POINT ( 'NONE',  ( -26.63011601220122060, -110.5936016518799221, 750.6326042729449455 ) ) ;
#37000 = CARTESIAN_POINT ( 'NONE',  ( 759.0159684113467620, -160.9181544815165807, -325.8855110935213020 ) ) ;
#37001 = APPLICATION_CONTEXT ( 'automotive_design' ) ;
#37002 = CARTESIAN_POINT ( 'NONE',  ( 792.2312462859673587, -59.90732993114762905, 307.2067596250082602 ) ) ;
#37003 = CARTESIAN_POINT ( 'NONE',  ( 919.9999999999993179, 219.9999999999998863, 359.9749999999999659 ) ) ;
#37004 = CARTESIAN_POINT ( 'NONE',  ( 763.2262854647970016, -368.6346026584193964, -309.2812353651462445 ) ) ;
#37005 = CARTESIAN_POINT ( 'NONE',  ( 755.3201227861273992, -51.72551174932946338, 345.3687786644892981 ) ) ;
#37006 = CARTESIAN_POINT ( 'NONE',  ( 755.8990559732751535, -275.4636090269708575, 365.9055244015606831 ) ) ;
#37007 = CIRCLE ( 'NONE', #28919, 19.99999999999990763 ) ;
#37008 = CARTESIAN_POINT ( 'NONE',  ( 758.8095938919642549, -248.0891481129651481, 311.6929314249763365 ) ) ;
#37009 = CARTESIAN_POINT ( 'NONE',  ( 767.7687537140311633, 0.09267006885218045942, -372.7932403749916830 ) ) ;
#37010 = FACE_BOUND ( 'NONE', #1199, .T. ) ;
#37011 = CARTESIAN_POINT ( 'NONE',  ( 959.5497976682736407, 239.9999999999998863, 350.0000000000000000 ) ) ;
#37012 = EDGE_CURVE ( 'NONE', #29607, #29231, #14686, .T. ) ;
#37013 = CARTESIAN_POINT ( 'NONE',  ( 781.7834795799800531, -370.8164208402375834, 315.0636971347436202 ) ) ;
#37014 = CARTESIAN_POINT ( 'NONE',  ( 800.9840315886518738, -124.9181544815167086, 354.1144889064786412 ) ) ;
#37015 = CARTESIAN_POINT ( 'NONE',  ( 775.9200461376533440, 0.1944037101305369775, -315.3028492785443291 ) ) ;
#37016 = LINE ( 'NONE', #15562, #26205 ) ;
#37017 = CARTESIAN_POINT ( 'NONE',  ( 786.4999999999993179, -512.9681489794448908, -327.9999999999999432 ) ) ;
#37018 = CARTESIAN_POINT ( 'NONE',  ( 795.6651683502461765, -130.7146871989599504, 371.3240766477733814 ) ) ;
#37019 = CARTESIAN_POINT ( 'NONE',  ( 759.9864689768902508, -386.0891481129647786, 354.9819416627836404 ) ) ;
#37020 = ORIENTED_EDGE ( 'NONE', *, *, #10316, .F. ) ;
#37021 = CARTESIAN_POINT ( 'NONE',  ( 795.9930595647434757, -315.0783235625957559, -320.7433823573372820 ) ) ;
#37023 = CARTESIAN_POINT ( 'NONE',  ( 788.7366044899766848, -155.9073299311473306, 316.5762568750059813 ) ) ;
#37022 = CARTESIAN_POINT ( 'NONE',  ( 755.5713283507202505, -149.3618753856928265, 334.6858677611754729 ) ) ;
#37024 = UNCERTAINTY_MEASURE_WITH_UNIT (LENGTH_MEASURE( 1.000000000000000082E-05 ), #32820, 'distance_accuracy_value', 'NONE');
#37025 = CARTESIAN_POINT ( 'NONE',  ( 808.7758568127978833, -340.1692326535047641, -320.0363995740631822 ) ) ;
#37026 = FACE_OUTER_BOUND ( 'NONE', #30221, .T. ) ;
#37027 = ORIENTED_EDGE ( 'NONE', *, *, #40217, .F. ) ;
#37028 = CARTESIAN_POINT ( 'NONE',  ( 800.0135310231082713, -350.0891481129648923, 325.0180583372163028 ) ) ;
#37029 = EDGE_LOOP ( 'NONE', ( #18666, #3768, #11037, #37261 ) ) ;
#37030 = LINE ( 'NONE', #5384, #40146 ) ;
#37031 = ADVANCED_FACE ( 'NONE', ( #22530 ), #23594, .F. ) ;
#37032 = CARTESIAN_POINT ( 'NONE',  ( 796.7737145352015204, -188.6346026584199365, -370.7187646348536987 ) ) ;
#37033 = CARTESIAN_POINT ( 'NONE',  ( 782.5225473063383106, -118.2709662947838041, 375.2698199232970637 ) ) ;
#37034 = ORIENTED_EDGE ( 'NONE', *, *, #11041, .F. ) ;
#37035 = VECTOR ( 'NONE', #15596, 1000.000000000000114 ) ;
#37036 = CARTESIAN_POINT ( 'NONE',  ( 778.1981804954715471, -178.2709662947835909, -314.8072714833591021 ) ) ;
#37037 = ORIENTED_EDGE ( 'NONE', *, *, #4371, .F. ) ;
#37038 = CARTESIAN_POINT ( 'NONE',  ( 804.4286716492782716, 6.638124614306706306, -345.3141322388244703 ) ) ;
#37039 = CARTESIAN_POINT ( 'NONE',  ( 759.0252816721024374, -264.9982390220561115, 368.0189434323527280 ) ) ;
#37040 = CARTESIAN_POINT ( 'NONE',  ( 805.1016975059191054, -174.8965053807779952, 343.0745993439771837 ) ) ;
#37042 = CARTESIAN_POINT ( 'NONE',  ( 799.9999999999993179, 205.0000000000000568, 255.0000000000000000 ) ) ;
#37041 = DIRECTION ( 'NONE',  ( 1.000000000000000000, 0.000000000000000000, -0.000000000000000000 ) ) ;
#37043 = EDGE_CURVE ( 'NONE', #8196, #14052, #2826, .T. ) ;
#37044 = ORIENTED_EDGE ( 'NONE', *, *, #31546, .T. ) ;
#37045 = CARTESIAN_POINT ( 'NONE',  ( 780.5236548040995785, -428.7363362996975980, -314.9735926884559944 ) ) ;
#37046 = CARTESIAN_POINT ( 'NONE',  ( -858.8365100919713768, 230.0000000000001990, -197.2499999999882903 ) ) ;
#37047 = CARTESIAN_POINT ( 'NONE',  ( 783.7953271457878373, -200.1908817542436907, -375.1787889125761239 ) ) ;
#37048 = CARTESIAN_POINT ( 'NONE',  ( 795.8262568251477660, -94.37269993606224716, 308.3538107759623585 ) ) ;
#37050 = CARTESIAN_POINT ( 'NONE',  ( 805.1927285166397041, -184.8164208402380950, -341.8018195045277707 ) ) ;
#37049 = CARTESIAN_POINT ( 'NONE',  ( 799.9999999999993179, 197.3292319334027241, -273.4704985657796783 ) ) ;
#37051 = CARTESIAN_POINT ( 'NONE',  ( 769.1273215169530886, -358.7146871989592114, -317.4527132478988847 ) ) ;
#37052 = CARTESIAN_POINT ( 'NONE',  ( 767.9999999999992042, 205.0000000000000568, -339.9999999999999432 ) ) ;
#37053 = CARTESIAN_POINT ( 'NONE',  ( 771.3260364891663130, -211.6454272087891582, -306.0683387631859773 ) ) ;
#37054 = CARTESIAN_POINT ( 'NONE',  ( 989.9999999999992042, 249.9999999999998863, 209.9999999999999716 ) ) ;
#37055 = CARTESIAN_POINT ( 'NONE',  ( 998.9999999999992042, 249.9999999999998863, 199.9999999999999716 ) ) ;
#37056 = CARTESIAN_POINT ( 'NONE',  ( 755.5913626894240451, -61.64542720878961291, -346.6156483768012890 ) ) ;
#37057 = CARTESIAN_POINT ( 'NONE',  ( 755.3028492785439312, -447.2817908451521021, 335.9200461376539693 ) ) ;
#37058 = VECTOR ( 'NONE', #33216, 1000.000000000000000 ) ;
#37059 = CARTESIAN_POINT ( 'NONE',  ( 812.7932403749906598, -231.1800572038743553, -327.7687537140311633 ) ) ;
#37060 = CARTESIAN_POINT ( 'NONE',  ( 802.5472867521000353, -244.3726999360617924, 350.8726784830461156 ) ) ;
#37061 = DIRECTION ( 'NONE',  ( 1.892425610156518354E-16, 1.000000000000000000, -0.000000000000000000 ) ) ;
#37062 = CARTESIAN_POINT ( 'NONE',  ( -879.9999999999992042, 240.0000000000002274, -244.9999999999999716 ) ) ;
#37063 = CARTESIAN_POINT ( 'NONE',  ( 774.6312213355099630, -47.36187538569312494, -364.6798772138717482 ) ) ;
#37064 = CARTESIAN_POINT ( 'NONE',  ( 786.2694204179717872, -165.2817908451529547, 305.1769319972829067 ) ) ;
#37065 = EDGE_CURVE ( 'NONE', #2171, #36781, #2856, .T. ) ;
#37066 = CARTESIAN_POINT ( 'NONE',  ( 811.6461892240364477, -124.7146871989599930, -324.1737431748509835 ) ) ;
#37067 = CARTESIAN_POINT ( 'NONE',  ( 767.6429770376289525, -153.1800572038746395, 306.8695393053162093 ) ) ;
#37068 = CARTESIAN_POINT ( 'NONE',  ( 755.2512626584698410, -367.5436935675102745, -315.2512626584710915 ) ) ;
#37069 = CARTESIAN_POINT ( 'NONE',  ( -829.9999999999992042, 529.9999999999997726, -360.0000000000000000 ) ) ;
#37070 = CARTESIAN_POINT ( 'NONE',  ( 774.6858677611749044, -249.7255117493288594, 315.5713283507209894 ) ) ;
#37071 = VECTOR ( 'NONE', #42596, 1000.000000000000000 ) ;
#37072 = CARTESIAN_POINT ( 'NONE',  ( 786.5483106153019435, -7.645427208789786100, 364.1601925771022366 ) ) ;
#37073 = CARTESIAN_POINT ( 'NONE',  ( 788.8264449731200330, -405.1800572038737300, -363.6646147819171233 ) ) ;
#37074 = DIRECTION ( 'NONE',  ( -1.000000000000000000, -0.000000000000000000, -0.000000000000000000 ) ) ;
#37075 = CARTESIAN_POINT ( 'NONE',  ( 812.7932403749906598, -447.1800572038736732, -327.7687537140311633 ) ) ;
#37076 = DIRECTION ( 'NONE',  ( -0.000000000000000000, -0.6755902076156505842, -0.7372773368101327440 ) ) ;
#37077 = CARTESIAN_POINT ( 'NONE',  ( 756.7813123517142913, -91.98741447168737295, 329.9779781133712504 ) ) ;
#37078 = VERTEX_POINT ( 'NONE', #15608 ) ;
#37079 = CARTESIAN_POINT ( 'NONE',  ( 798.7617431975189675, -219.6237781080506295, -323.0428371773161871 ) ) ;
#37080 = CARTESIAN_POINT ( 'NONE',  ( 771.1735550268778070, -57.18005720387489532, 316.3353852180827630 ) ) ;
#37081 = CARTESIAN_POINT ( 'NONE',  ( 793.4146539503750546, -217.9874144716870035, -307.6481478633938877 ) ) ;
#37082 = CARTESIAN_POINT ( 'NONE',  ( 808.7758568127978833, -388.1692326535045936, 320.0363995740631822 ) ) ;
#37083 = ORIENTED_EDGE ( 'NONE', *, *, #15333, .F. ) ;
#37084 = EDGE_CURVE ( 'NONE', #27336, #19541, #16691, .T. ) ;
#37085 = CARTESIAN_POINT ( 'NONE',  ( 800.0135310231082713, -182.0891481129654323, -325.0180583372163028 ) ) ;
#37086 = CARTESIAN_POINT ( 'NONE',  ( 804.4286716492782716, -377.3618753856920875, 345.3141322388244703 ) ) ;
#37087 = EDGE_CURVE ( 'NONE', #13538, #5955, #9751, .T. ) ;
#37088 = CARTESIAN_POINT ( 'NONE',  ( 744.7301800767019131, -76.81642084023845030, -337.4774526936615757 ) ) ;
#37089 = AXIS2_PLACEMENT_3D ( 'NONE', #30824, #26658, #26445 ) ;
#37090 = CARTESIAN_POINT ( 'NONE',  ( 805.1927285166399315, -88.81642084023843609, -341.8018195045277707 ) ) ;
#37091 = ORIENTED_EDGE ( 'NONE', *, *, #6607, .T. ) ;
#37092 = CARTESIAN_POINT ( 'NONE',  ( 758.4439275373578084, -12.55451811788067751, -353.2243759319684386 ) ) ;
#37093 = ORIENTED_EDGE ( 'NONE', *, *, #42786, .F. ) ;
#37094 = CARTESIAN_POINT ( 'NONE',  ( 799.2566176426618085, -336.0090635724251911, -324.0069404352559559 ) ) ;
#37096 = CARTESIAN_POINT ( 'NONE',  ( 790.0220218866281812, -415.0999726633340288, 363.2186876482849129 ) ) ;
#37095 = CARTESIAN_POINT ( 'NONE',  ( 800.0135310231082713, -86.08914811296573077, 325.0180583372163028 ) ) ;
#37099 = CARTESIAN_POINT ( 'NONE',  ( 773.7943932421234194, -335.8055962898683902, 305.5313806188329409 ) ) ;
#37098 = DIRECTION ( 'NONE',  ( 1.000000000000000000, 0.000000000000000000, -0.000000000000000000 ) ) ;
#37097 = CARTESIAN_POINT ( 'NONE',  ( 748.9653473494365699, -434.6346026584190554, 356.9462024416520762 ) ) ;
#37100 = ADVANCED_FACE ( 'NONE', ( #12148 ), #505, .T. ) ;
#37101 = CARTESIAN_POINT ( 'NONE',  ( 757.4527132478984868, -328.3726999360615650, -329.1273215169538844 ) ) ;
#37102 = CARTESIAN_POINT ( 'NONE',  ( 771.2633955100217236, -335.9073299311468190, -363.4237431249939618 ) ) ;
#37103 = CARTESIAN_POINT ( 'NONE',  ( 802.1676090361156639, -158.6346026584199933, -327.8955696845344505 ) ) ;
#37104 = CARTESIAN_POINT ( 'NONE',  ( 809.0717654672305343, -4.918154481517067467, 360.1688906516309885 ) ) ;
#37106 = CARTESIAN_POINT ( 'NONE',  ( -28.63011601220122415, -544.8427095258973623, -369.9999999999999432 ) ) ;
#37105 = DIRECTION ( 'NONE',  ( -0.000000000000000000, 1.000000000000000000, -0.000000000000000000 ) ) ;
#37107 = CARTESIAN_POINT ( 'NONE',  ( 783.0433043558608688, -264.8965053807776826, -315.1538015810313027 ) ) ;
#37108 = CARTESIAN_POINT ( 'NONE',  ( 745.1792804349281596, -134.1908817542439181, -343.7566961878542884 ) ) ;
#37109 = CARTESIAN_POINT ( 'NONE',  ( 789.5584187865343893, -452.9681489794450613, 363.1011989789364520 ) ) ;
#37110 = FACE_OUTER_BOUND ( 'NONE', #33237, .T. ) ;
#37111 = CARTESIAN_POINT ( 'NONE',  ( 790.0220218866281812, -295.0999726633343698, 363.2186876482849129 ) ) ;
#37112 = VERTEX_POINT ( 'NONE', #27984 ) ;
#37113 = CARTESIAN_POINT ( 'NONE',  ( 767.6429770376291799, -153.1800572038746111, -306.8695393053162093 ) ) ;
#37114 = EDGE_CURVE ( 'NONE', #23583, #17118, #13911, .T. ) ;
#37115 = PLANE ( 'NONE',  #31228 ) ;
#37116 = CARTESIAN_POINT ( 'NONE',  ( 760.0363995740630116, -58.91815448151690759, 368.7758568127991907 ) ) ;
#37117 = ADVANCED_FACE ( 'NONE', ( #42300 ), #10664, .T. ) ;
#37118 = CARTESIAN_POINT ( 'NONE',  ( 812.7932403749906598, -279.1800572038741848, -327.7687537140311633 ) ) ;
#37119 = PLANE ( 'NONE',  #35774 ) ;
#37120 = CARTESIAN_POINT ( 'NONE',  ( 797.8594530101008786, -133.5436935675110135, 322.1405469898980982 ) ) ;
#37121 = AXIS2_PLACEMENT_3D ( 'NONE', #26502, #2015, #40603 ) ;
#37122 = ORIENTED_EDGE ( 'NONE', *, *, #955, .T. ) ;
#37123 = CARTESIAN_POINT ( 'NONE',  ( 747.3154664389472828, -331.9874144716865203, -326.4474001241230781 ) ) ;
#37124 = AXIS2_PLACEMENT_3D ( 'NONE', #28664, #42966, #14812 ) ;
#37125 = CARTESIAN_POINT ( 'NONE',  ( 808.3070685750230950, -90.99823902205663728, -361.1904061080339261 ) ) ;
#37126 = CARTESIAN_POINT ( 'NONE',  ( 763.0428371773158460, -11.46360902697159290, 358.7617431975195359 ) ) ;
#37127 = CARTESIAN_POINT ( 'NONE',  ( 751.6929314249748586, -366.9982390220556567, -318.8095938919659034 ) ) ;
#37128 = CYLINDRICAL_SURFACE ( 'NONE', #1818, 8.024999999999948841 ) ;
#37129 = CARTESIAN_POINT ( 'NONE',  ( 790.8726784830453198, -418.7146871989590409, 362.5472867521010585 ) ) ;
#37130 = ORIENTED_EDGE ( 'NONE', *, *, #43119, .F. ) ;
#37131 = EDGE_CURVE ( 'NONE', #35125, #34305, #17372, .T. ) ;
#37132 = CARTESIAN_POINT ( 'NONE',  ( 761.9338519418445230, -110.5328690171418629, -370.4231160770881957 ) ) ;
#37133 = DIRECTION ( 'NONE',  ( -1.000000000000000000, -0.000000000000000000, 0.000000000000000000 ) ) ;
#37134 = CARTESIAN_POINT ( 'NONE',  ( 752.4576283171824116, -237.0783235625960117, 317.7880784355627952 ) ) ;
#37135 = CARTESIAN_POINT ( 'NONE',  ( 803.6646147819162707, -89.90732993114752958, 348.8264449731211130 ) ) ;
#37136 = ORIENTED_EDGE ( 'NONE', *, *, #8252, .T. ) ;
#37137 = AXIS2_PLACEMENT_3D ( 'NONE', #4551, #15414, #18202 ) ;
#37138 = EDGE_CURVE ( 'NONE', #38643, #12556, #13941, .T. ) ;
#37139 = CARTESIAN_POINT ( 'NONE',  ( 756.1348686366196716, 6.739858255585061464, -347.5531968255698416 ) ) ;
#37140 = CARTESIAN_POINT ( 'NONE',  ( 803.4237431249931660, -255.1800572038742700, 331.2633955100225194 ) ) ;
#37141 = EDGE_CURVE ( 'NONE', #9315, #17287, #21289, .T. ) ;
#37142 = CARTESIAN_POINT ( 'NONE',  ( 759.8311093483677041, -430.1692326535043094, -310.9282345327691814 ) ) ;
#37143 = LINE ( 'NONE', #37384, #37201 ) ;
#37144 = ORIENTED_EDGE ( 'NONE', *, *, #15665, .F. ) ;
#37145 = ORIENTED_EDGE ( 'NONE', *, *, #42510, .T. ) ;
#37146 = CARTESIAN_POINT ( 'NONE',  ( 764.1737431748507561, -394.3726999360613377, -371.6461892240376415 ) ) ;
#37147 = CARTESIAN_POINT ( 'NONE',  ( 756.5762568750052424, -243.1800572038743269, -348.7366044899774238 ) ) ;
#37148 = CARTESIAN_POINT ( 'NONE',  ( 813.1304606946831655, -329.9073299311467622, 352.3570229623691716 ) ) ;
#37149 = CARTESIAN_POINT ( 'NONE',  ( 768.8385539511368734, -47.26014174441477422, 306.4236121716840557 ) ) ;
#37150 = CARTESIAN_POINT ( 'NONE',  ( 805.2837595273609850, -218.7363362996982232, -340.5290396650784714 ) ) ;
#37151 = CARTESIAN_POINT ( 'NONE',  ( 804.6798772138708955, -207.7255117493289447, -334.6312213355107019 ) ) ;
#37152 = CIRCLE ( 'NONE', #17254, 20.00000000000001776 ) ;
#37153 = CARTESIAN_POINT ( 'NONE',  ( 781.8018195045267476, -406.2709662947828519, -365.1927285166407273 ) ) ;
#37154 = VECTOR ( 'NONE', #17884, 1000.000000000000114 ) ;
#37155 = ORIENTED_EDGE ( 'NONE', *, *, #5195, .F. ) ;
#37156 = CARTESIAN_POINT ( 'NONE',  ( 755.3201227861273992, -195.7255117493289731, 345.3687786644892981 ) ) ;
#37157 = CARTESIAN_POINT ( 'NONE',  ( 778.1981804954714335, -106.2709662947838467, -314.8072714833589885 ) ) ;
#37158 = EDGE_LOOP ( 'NONE', ( #40634, #43085, #36822, #21087, #986, #22154, #28608, #8084 ) ) ;
#37159 = CARTESIAN_POINT ( 'NONE',  ( 812.7932403749906598, -327.1800572038741279, 327.7687537140311633 ) ) ;
#37160 = DIRECTION ( 'NONE',  ( 0.000000000000000000, 0.000000000000000000, -1.000000000000000000 ) ) ;
#37161 = DIRECTION ( 'NONE',  ( -1.000000000000000000, 0.000000000000000000, -0.000000000000000000 ) ) ;
#37162 = CARTESIAN_POINT ( 'NONE',  ( 51.16348990802859475, 260.0000000000000568, -199.9999999999945146 ) ) ;
#37163 = CARTESIAN_POINT ( 'NONE',  ( 757.0176451133909268, -181.0999726633347109, 349.9200121543848354 ) ) ;
#37164 = CARTESIAN_POINT ( 'NONE',  ( 801.9419747391806368, -66.45278447660216159, 351.9812246680014027 ) ) ;
#37165 = VERTEX_POINT ( 'NONE', #14366 ) ;
#37166 = CARTESIAN_POINT ( 'NONE',  ( 764.1737431748507561, -442.3726999360611103, -371.6461892240376415 ) ) ;
#37167 = CARTESIAN_POINT ( 'NONE',  ( 744.7301800767020268, -28.81642084023863504, -337.4774526936615189 ) ) ;
#37168 = CARTESIAN_POINT ( 'NONE',  ( 795.9930595647434757, -243.0783235625959833, 320.7433823573372820 ) ) ;
#37169 = CARTESIAN_POINT ( 'NONE',  ( 792.1044303154645831, -396.4527844766010389, -317.8323909638837677 ) ) ;
#37170 = CARTESIAN_POINT ( 'NONE',  ( 762.1405469898973024, -1.543693567511449594, -357.8594530101016176 ) ) ;
#37171 = AXIS2_PLACEMENT_3D ( 'NONE', #990, #14178, #43263 ) ;
#37172 = CARTESIAN_POINT ( 'NONE',  ( 767.7687537140311633, -431.9073299311464211, 372.7932403749916830 ) ) ;
#37173 = DIRECTION ( 'NONE',  ( 1.000000000000000000, 0.000000000000000000, 0.000000000000000000 ) ) ;
#37174 = CARTESIAN_POINT ( 'NONE',  ( 760.7433823573367135, -300.0090635724252479, -355.9930595647440441 ) ) ;
#37175 = CARTESIAN_POINT ( 'NONE',  ( 749.2812353651451076, -150.4527844766018916, -323.2262854647983090 ) ) ;
#37176 = CARTESIAN_POINT ( 'NONE',  ( 782.4968714119720516, -82.81642084023846451, 305.0891759886411023 ) ) ;
#37177 = CARTESIAN_POINT ( 'NONE',  ( 801.1904061080336987, -140.0891481129654892, 368.3070685750235498 ) ) ;
#37178 = CARTESIAN_POINT ( 'NONE',  ( 795.0120564873543572, 16.45630643248849267, -314.4408280072604498 ) ) ;
#37179 = DIRECTION ( 'NONE',  ( -0.000000000000000000, 1.000000000000000000, -0.000000000000000000 ) ) ;
#37180 = DIRECTION ( 'NONE',  ( -1.880165489482579047E-16, -1.000000000000000000, -0.000000000000000000 ) ) ;
#37181 = CARTESIAN_POINT ( 'NONE',  ( 754.9967657858570647, -361.5436935675103882, 365.0032342141425374 ) ) ;
#37182 = CARTESIAN_POINT ( 'NONE',  ( 755.5713283507202505, -365.3618753856920875, -334.6858677611754729 ) ) ;
#37183 = CIRCLE ( 'NONE', #23156, 8.025000000000003908 ) ;
#37184 = CARTESIAN_POINT ( 'NONE',  ( 789.5670355615794733, -453.0432664090020012, 363.0970091259334822 ) ) ;
#37185 = CIRCLE ( 'NONE', #17285, 9.999999999999982236 ) ;
#37186 = CARTESIAN_POINT ( 'NONE',  ( 768.9521613784389729, -105.8272453906076578, -373.2346286133773106 ) ) ;
#37187 = CARTESIAN_POINT ( 'NONE',  ( 803.2186876482843445, -151.9874144716871740, -350.0220218866286928 ) ) ;
#37188 = CARTESIAN_POINT ( 'NONE',  ( 807.5423716828161105, -129.0783235625963243, 362.2119215644372048 ) ) ;
#37189 = CARTESIAN_POINT ( 'NONE',  ( 799.9999999999993179, 212.6707680665973612, 236.5295014342203785 ) ) ;
#37190 = CARTESIAN_POINT ( 'NONE',  ( 801.9419747391806368, -42.45278447660223264, -351.9812246680014027 ) ) ;
#37191 = CARTESIAN_POINT ( 'NONE',  ( 764.0069404352550464, -183.0783235625961538, -359.2566176426627180 ) ) ;
#37192 = CARTESIAN_POINT ( 'NONE',  ( 795.1360043628807261, -140.0891481129654892, -360.2193346964456282 ) ) ;
#37193 = CARTESIAN_POINT ( 'NONE',  ( 797.6776695296629214, -139.5436935675110135, 357.6776695296636603 ) ) ;
#37194 = CARTESIAN_POINT ( 'NONE',  ( 787.6308680596127942, -419.2601417444136587, -364.1105419155492768 ) ) ;
#37196 = CARTESIAN_POINT ( 'NONE',  ( 803.6646147819162707, -305.9073299311468190, 348.8264449731211130 ) ) ;
#37195 = CARTESIAN_POINT ( 'NONE',  ( 791.9812246680005501, -284.6346026584196807, 361.9419747391813189 ) ) ;
#37197 = CARTESIAN_POINT ( 'NONE',  ( -728.8365100919714905, 256.5000000000001705, -202.7499999999890008 ) ) ;
#37198 = VERTEX_POINT ( 'NONE', #20595 ) ;
#37199 = CARTESIAN_POINT ( 'NONE',  ( 780.5290396650775619, 11.64894916467595642, 365.2837595273619513 ) ) ;
#37200 = CARTESIAN_POINT ( 'NONE',  ( 778.7629533639073998, -272.7363362996981095, -375.0009284576466371 ) ) ;
#37201 = VECTOR ( 'NONE', #1800, 1000.000000000000114 ) ;
#37202 = ORIENTED_EDGE ( 'NONE', *, *, #24100, .F. ) ;
#37203 = PRODUCT_CONTEXT ( 'NONE', #8103, 'mechanical' ) ;
#37204 = CIRCLE ( 'NONE', #43130, 24.99999999999991118 ) ;
#37205 = CARTESIAN_POINT ( 'NONE',  ( 744.7301800767020268, -220.8164208402380098, 337.4774526936615189 ) ) ;
#37206 = CARTESIAN_POINT ( 'NONE',  ( 776.9254006560222479, -284.1908817542434917, 314.8983024940802125 ) ) ;
#37207 = CARTESIAN_POINT ( 'NONE',  ( 779.4709603349208464, -384.3510508353227806, 314.7162404726379918 ) ) ;
#37208 = ORIENTED_EDGE ( 'NONE', *, *, #43865, .T. ) ;
#37209 = CARTESIAN_POINT ( 'NONE',  ( 758.4439275373578084, -108.5545181178803915, -353.2243759319684386 ) ) ;
#37210 = CARTESIAN_POINT ( 'NONE',  ( 755.5713283507202505, -101.3618753856929544, -334.6858677611754729 ) ) ;
#37211 = CARTESIAN_POINT ( 'NONE',  ( 788.7366044899766848, -275.9073299311469896, -316.5762568750059813 ) ) ;
#37212 = ORIENTED_EDGE ( 'NONE', *, *, #43627, .F. ) ;
#37213 = CARTESIAN_POINT ( 'NONE',  ( 771.2633955100217236, -431.9073299311464211, -363.4237431249939618 ) ) ;
#37214 = CARTESIAN_POINT ( 'NONE',  ( 755.5713283507202505, -77.36187538569302546, -334.6858677611754729 ) ) ;
#37215 = CARTESIAN_POINT ( 'NONE',  ( 772.3691319403857278, -287.2601417444140566, 315.8894580844506663 ) ) ;
#37216 = CARTESIAN_POINT ( 'NONE',  ( -338.8365100919713200, 260.0000000000001137, -199.9999999999917861 ) ) ;
#37217 = CARTESIAN_POINT ( 'NONE',  ( 779.9999999999992042, -452.9681489794448339, 339.9999999999999432 ) ) ;
#37218 = CLOSED_SHELL ( 'NONE', ( #36297, #18231, #2134, #9320, #2666, #15122, #30361, #8922, #189, #16424, #37359, #29455, #2898, #1683, #16249, #35439, #25881, #45301, #33114, #14549, #39690, #13990, #26366, #10564, #43923, #42743, #4877, #9473, #32015, #23787, #41864, #1558, #39989, #21946, #2662, #21867, #35479, #34502, #23017, #22066, #35141, #19895, #27548, #6374, #14244, #11532, #11354, #39414, #34581, #32368, #18807, #10276, #9724, #37031, #15944, #27196 ) ) ;
#37219 = CARTESIAN_POINT ( 'NONE',  ( 454.7528517110262101, 199.9999999999999432, -122.7905160835442615 ) ) ;
#37220 = ORIENTED_EDGE ( 'NONE', *, *, #10099, .T. ) ;
#37221 = CARTESIAN_POINT ( 'NONE',  ( 786.2694204179717872, -333.2817908451523863, -305.1769319972829067 ) ) ;
#37222 = CIRCLE ( 'NONE', #4797, 6.119000000000013095 ) ;
#37223 = CARTESIAN_POINT ( 'NONE',  ( 768.9521613784389729, -201.8272453906073451, 373.2346286133773106 ) ) ;
#37225 = CARTESIAN_POINT ( 'NONE',  ( 800.2193346964447755, -282.9982390220558841, -355.1360043628815788 ) ) ;
#37224 = DIRECTION ( 'NONE',  ( 0.000000000000000000, 0.000000000000000000, -1.000000000000000000 ) ) ;
#37226 = DIRECTION ( 'NONE',  ( 0.000000000000000000, -0.000000000000000000, 1.000000000000000000 ) ) ;
#37227 = CARTESIAN_POINT ( 'NONE',  ( 760.7433823573367135, -204.0090635724255606, -355.9930595647440441 ) ) ;
#37228 = CARTESIAN_POINT ( 'NONE',  ( 810.7187646348534145, -42.45278447660223264, 356.7737145352016341 ) ) ;
#37229 = DIRECTION ( 'NONE',  ( -0.000000000000000000, 1.000000000000000000, -1.586032892321652088E-15 ) ) ;
#37230 = CARTESIAN_POINT ( 'NONE',  ( 787.5162901302840055, -395.3618753856919739, -305.4481719005793252 ) ) ;
#37231 =( LENGTH_UNIT ( ) NAMED_UNIT ( * ) SI_UNIT ( .MILLI., .METRE. ) );
#37232 = CARTESIAN_POINT ( 'NONE',  ( 788.7366044899766848, -59.90732993114762905, 316.5762568750059813 ) ) ;
#37233 = CIRCLE ( 'NONE', #44603, 10.00000000000000888 ) ;
#37234 = CARTESIAN_POINT ( 'NONE',  ( 745.1792804349281596, -326.1908817542433781, 343.7566961878542884 ) ) ;
#37235 = CARTESIAN_POINT ( 'NONE',  ( 745.0891759886404770, -244.2709662947834204, 342.4968714119734159 ) ) ;
#37236 = CARTESIAN_POINT ( 'NONE',  ( 796.9462024416508257, -12.45278447660232146, -308.9653473494370246 ) ) ;
#37237 = CARTESIAN_POINT ( 'NONE',  ( 778.1981804954714335, -250.2709662947832783, -314.8072714833589885 ) ) ;
#37238 = VECTOR ( 'NONE', #32893, 1000.000000000000000 ) ;
#37239 = CARTESIAN_POINT ( 'NONE',  ( -78.83651009197140525, 256.5000000000000568, -199.9999999999936051 ) ) ;
#37240 = AXIS2_PLACEMENT_3D ( 'NONE', #21041, #34680, #19741 ) ;
#37241 = CARTESIAN_POINT ( 'NONE',  ( 762.3223304703356007, -343.5436935675103314, 322.3223304703362828 ) ) ;
#37242 = CARTESIAN_POINT ( 'NONE',  ( 757.4527132478984868, -136.3726999360621051, 329.1273215169538844 ) ) ;
#37243 = CARTESIAN_POINT ( 'NONE',  ( 799.4546378042377910, -9.078323562596708030, -356.1575198192848006 ) ) ;
#37244 = CARTESIAN_POINT ( 'NONE',  ( 765.0180583372156207, -384.9982390220556567, 360.0135310231089534 ) ) ;
#37245 = DIRECTION ( 'NONE',  ( -0.000000000000000000, 1.000000000000000000, -0.000000000000000000 ) ) ;
#37246 = CARTESIAN_POINT ( 'NONE',  ( -39.63011601220123481, 26.27639943461401018, 900.0000000000001137 ) ) ;
#37247 = CARTESIAN_POINT ( 'NONE',  ( 754.8072714833581358, -412.8164208402372992, 338.1981804954720587 ) ) ;
#37248 = ORIENTED_EDGE ( 'NONE', *, *, #37727, .F. ) ;
#37249 = CARTESIAN_POINT ( 'NONE',  ( 788.8264449731200330, -45.18005720387493085, -363.6646147819171233 ) ) ;
#37250 = VECTOR ( 'NONE', #26666, 1000.000000000000000 ) ;
#37251 = CARTESIAN_POINT ( 'NONE',  ( 783.0433043558608688, -336.8965053807774552, -315.1538015810313027 ) ) ;
#37253 = CARTESIAN_POINT ( 'NONE',  ( 768.0187753319979720, -152.6346026584200786, 318.0580252608186242 ) ) ;
#37252 = CARTESIAN_POINT ( 'NONE',  ( 797.6776695296629214, -187.5436935675108430, 357.6776695296636603 ) ) ;
#37254 = ADVANCED_FACE ( 'NONE', ( #42079 ), #31673, .F. ) ;
#37255 = CIRCLE ( 'NONE', #1841, 6.118999999999985562 ) ;
#37256 = CARTESIAN_POINT ( 'NONE',  ( 744.9990715423526808, -378.3510508353227806, -341.2370466360926002 ) ) ;
#37257 = DIRECTION ( 'NONE',  ( 0.000000000000000000, 0.000000000000000000, 1.000000000000000000 ) ) ;
#37258 = ORIENTED_EDGE ( 'NONE', *, *, #29199, .F. ) ;
#37259 = CARTESIAN_POINT ( 'NONE',  ( 778.1981804954714335, -370.2709662947831362, 314.8072714833589885 ) ) ;
#37260 = VECTOR ( 'NONE', #5537, 1000.000000000000000 ) ;
#37261 = ORIENTED_EDGE ( 'NONE', *, *, #28090, .T. ) ;
#37262 = DIRECTION ( 'NONE',  ( -0.000000000000000000, 1.000000000000000000, -0.000000000000000000 ) ) ;
#37263 = CARTESIAN_POINT ( 'NONE',  ( 782.4968714119720516, -178.8164208402381519, -305.0891759886411023 ) ) ;
#37264 = CARTESIAN_POINT ( 'NONE',  ( 814.9108240113580450, -112.2709662947838325, 337.5031285880265273 ) ) ;
#37265 = ORIENTED_EDGE ( 'NONE', *, *, #7148, .F. ) ;
#37266 = VECTOR ( 'NONE', #45666, 1000.000000000000000 ) ;
#37267 = CARTESIAN_POINT ( 'NONE',  ( 791.9812246680005501, -164.6346026584200217, -361.9419747391813189 ) ) ;
#37268 = VERTEX_POINT ( 'NONE', #38613 ) ;
#37269 = CARTESIAN_POINT ( 'NONE',  ( 804.6798772138708955, -327.7255117493285184, -334.6312213355107019 ) ) ;
#37270 = CARTESIAN_POINT ( 'NONE',  ( 791.9460785601769430, -462.7578698805381237, -362.0383033825738721 ) ) ;
#37271 = CARTESIAN_POINT ( 'NONE',  ( 748.9653473494363425, -266.6346026584197375, 356.9462024416521331 ) ) ;
#37272 = CARTESIAN_POINT ( 'NONE',  ( 754.8983024940795303, -210.8965053807778816, 336.9254006560228163 ) ) ;
#37274 = CARTESIAN_POINT ( 'NONE',  ( -928.0249999999991815, 154.9999999999998863, 350.0000000000000000 ) ) ;
#37273 = CARTESIAN_POINT ( 'NONE',  ( 998.9999999999992042, 249.9999999999998863, -360.0000000000000000 ) ) ;
#37275 = FACE_OUTER_BOUND ( 'NONE', #33536, .T. ) ;
#37276 = AXIS2_PLACEMENT_3D ( 'NONE', #8406, #33126, #29642 ) ;
#37277 = ORIENTED_EDGE ( 'NONE', *, *, #19836, .F. ) ;
#37278 = EDGE_CURVE ( 'NONE', #16704, #37595, #2125, .T. ) ;
#37279 = CARTESIAN_POINT ( 'NONE',  ( 793.0897708529556667, -438.5545181178793541, -361.3366627262616362 ) ) ;
#37280 = LINE ( 'NONE', #19733, #37372 ) ;
#37281 = VERTEX_POINT ( 'NONE', #3741 ) ;
#37282 = CARTESIAN_POINT ( 'NONE',  ( 814.4686193811664907, -243.2817908451526705, -346.2056067578752732 ) ) ;
#37283 = CARTESIAN_POINT ( 'NONE',  ( 771.3260364891663130, -115.6454272087894424, 306.0683387631859773 ) ) ;
#37285 = CARTESIAN_POINT ( 'NONE',  ( 758.0580252608178853, -174.4527844766018063, -328.0187753319985404 ) ) ;
#37284 = CARTESIAN_POINT ( 'NONE',  ( 794.9999999999993179, -365.3551492539851893, 18.13243251470705886 ) ) ;
#37286 = CARTESIAN_POINT ( 'NONE',  ( 776.9566956441375396, -348.8965053807774552, -364.8461984189686405 ) ) ;
#37287 = FACE_OUTER_BOUND ( 'NONE', #18653, .T. ) ;
#37288 = CARTESIAN_POINT ( 'NONE',  ( 750.9282345327678740, -232.9181544815163249, -319.8311093483690115 ) ) ;
#37289 = CARTESIAN_POINT ( 'NONE',  ( 701.1634899080286232, 256.4999999999999432, -199.9999999999990337 ) ) ;
#37290 = CARTESIAN_POINT ( 'NONE',  ( 701.1634899080286232, 256.4999999999999432, -199.9999999999990337 ) ) ;
#37291 = CARTESIAN_POINT ( 'NONE',  ( 783.0745993439762742, -80.19088175424411702, -365.1016975059196739 ) ) ;
#37292 = CARTESIAN_POINT ( 'NONE',  ( 780.5236548040995785, -452.7363362996975411, 314.9735926884559944 ) ) ;
#37293 = DIRECTION ( 'NONE',  ( -0.000000000000000000, 0.000000000000000000, 1.000000000000000000 ) ) ;
#37294 = VECTOR ( 'NONE', #43259, 1000.000000000000000 ) ;
#37295 = CARTESIAN_POINT ( 'NONE',  ( 792.2312462859673587, -275.9073299311469896, -307.2067596250082602 ) ) ;
#37296 = DIRECTION ( 'NONE',  ( -1.000000000000000000, 0.000000000000000000, 0.000000000000000000 ) ) ;
#37297 = CARTESIAN_POINT ( 'NONE',  ( -265.7583438952258916, -600.0000000000000000, -244.9999999999999716 ) ) ;
#37298 = CARTESIAN_POINT ( 'NONE',  ( 764.8639956371174549, -56.08914811296580893, -319.7806653035542013 ) ) ;
#37299 = AXIS2_PLACEMENT_3D ( 'NONE', #4516, #818, #8210 ) ;
#37300 = CARTESIAN_POINT ( 'NONE',  ( 802.2119215644370342, -222.0090635724254184, 367.5423716828165084 ) ) ;
#37301 = CARTESIAN_POINT ( 'NONE',  ( 788.7631598425961101, -145.4419599262326699, -305.7194118038759143 ) ) ;
#37302 = CARTESIAN_POINT ( 'NONE',  ( 772.4837098697144029, -143.3618753856927697, 374.5518280994205611 ) ) ;
#37303 = CARTESIAN_POINT ( 'NONE',  ( 787.5162901302840055, -395.3618753856918602, -305.4481719005792684 ) ) ;
#37304 = DIRECTION ( 'NONE',  ( 1.000000000000000000, 0.000000000000000000, -0.000000000000000000 ) ) ;
#37305 = CARTESIAN_POINT ( 'NONE',  ( 771.1735550268778070, -249.1800572038742416, 316.3353852180827630 ) ) ;
#37306 = CARTESIAN_POINT ( 'NONE',  ( 804.1105419155481968, -27.82724539060790292, 347.6308680596136469 ) ) ;
#37307 = CARTESIAN_POINT ( 'NONE',  ( 774.6312213355099630, -383.3618753856921444, -364.6798772138717482 ) ) ;
#37308 = DIRECTION ( 'NONE',  ( -0.000000000000000000, -0.000000000000000000, -1.000000000000000000 ) ) ;
#37309 = CARTESIAN_POINT ( 'NONE',  ( 781.2370466360911223, -44.73633629969875614, -304.9990715423533629 ) ) ;
#37310 = DIRECTION ( 'NONE',  ( -1.880165489482579047E-16, -1.000000000000000000, -0.000000000000000000 ) ) ;
#37312 = CARTESIAN_POINT ( 'NONE',  ( 801.9419747391806368, -306.4527844766013800, 351.9812246680014027 ) ) ;
#37311 = CARTESIAN_POINT ( 'NONE',  ( 804.9511171171677688, -77.80559628986920018, 335.8780910478229202 ) ) ;
#37313 = ORIENTED_EDGE ( 'NONE', *, *, #33110, .F. ) ;
#37314 = CARTESIAN_POINT ( 'NONE',  ( 755.5713283507202505, -269.3618753856924286, 334.6858677611754729 ) ) ;
#37315 = EDGE_CURVE ( 'NONE', #14073, #43845, #41286, .T. ) ;
#37316 = VECTOR ( 'NONE', #15374, 1000.000000000000000 ) ;
#37317 = CARTESIAN_POINT ( 'NONE',  ( 776.9566956441375396, -228.8965053807778816, -364.8461984189686405 ) ) ;
#37318 = CARTESIAN_POINT ( 'NONE',  ( 767.8955696845333705, -120.4527844766019484, -362.1676090361162323 ) ) ;
#37319 = CARTESIAN_POINT ( 'NONE',  ( 764.8639956371174549, -56.08914811296580893, 319.7806653035542013 ) ) ;
#37320 = CARTESIAN_POINT ( 'NONE',  ( 756.1443688327750579, -237.6237781080505442, -314.3581564841659315 ) ) ;
#37321 = DIRECTION ( 'NONE',  ( 0.000000000000000000, -1.000000000000000000, 0.000000000000000000 ) ) ;
#37322 = CARTESIAN_POINT ( 'NONE',  ( 800.1688906516307043, -394.1692326535045368, 369.0717654672308186 ) ) ;
#37323 = VERTEX_POINT ( 'NONE', #7436 ) ;
#37324 = CARTESIAN_POINT ( 'NONE',  ( 813.9316612368132837, -439.4419599262316751, 348.6739635108323228 ) ) ;
#37325 = CARTESIAN_POINT ( 'NONE',  ( 795.1360043628807261, -164.0891481129655176, -360.2193346964456282 ) ) ;
#37326 = CARTESIAN_POINT ( 'NONE',  ( 778.2165204200184689, -358.8164208402375834, 364.9363028652563230 ) ) ;
#37327 = CARTESIAN_POINT ( 'NONE',  ( 800.9747183278959710, -60.99823902205671544, -311.9810565676471583 ) ) ;
#37328 = CARTESIAN_POINT ( 'NONE',  ( 785.3687786644885591, -83.36187538569299704, -315.3201227861280813 ) ) ;
#37329 = ORIENTED_EDGE ( 'NONE', *, *, #202, .T. ) ;
#37330 = CARTESIAN_POINT ( 'NONE',  ( 780.5236548040995785, -20.73633629969883430, -314.9735926884559944 ) ) ;
#37331 = CIRCLE ( 'NONE', #13746, 10.00000000000000888 ) ;
#37332 = ORIENTED_EDGE ( 'NONE', *, *, #19126, .F. ) ;
#37333 = CARTESIAN_POINT ( 'NONE',  ( 799.2566176426618085, -360.0090635724250774, -324.0069404352559559 ) ) ;
#37335 = CARTESIAN_POINT ( 'NONE',  ( 779.4763451958990572, -392.7363362996977116, 365.0264073115438919 ) ) ;
#37334 = CARTESIAN_POINT ( 'NONE',  ( 778.2165204200184689, -94.81642084023843609, 364.9363028652563230 ) ) ;
#37336 = CONICAL_SURFACE ( 'NONE', #15207, 8.024999999999948841, 0.7853981633974337351 ) ;
#37339 = CARTESIAN_POINT ( 'NONE',  ( 813.9316612368132837, -319.4419599262320730, 348.6739635108323228 ) ) ;
#37338 = LINE ( 'NONE', #12852, #10735 ) ;
#37337 = CARTESIAN_POINT ( 'NONE',  ( 777.5031285880264704, -430.8164208402374129, 374.9108240113588408 ) ) ;
#37340 = CARTESIAN_POINT ( 'NONE',  ( 744.9990715423526808, -114.3510508353236617, 341.2370466360926002 ) ) ;
#37341 = CARTESIAN_POINT ( 'NONE',  ( 787.5531968255692163, -309.8272453906070041, -316.1348686366205811 ) ) ;
#37342 = CARTESIAN_POINT ( 'NONE',  ( 755.3201227861273992, -315.7255117493286320, -345.3687786644892981 ) ) ;
#37343 = CARTESIAN_POINT ( 'NONE',  ( 814.8207195650702488, -146.1908817542438896, -336.2433038121456548 ) ) ;
#37344 = CARTESIAN_POINT ( 'NONE',  ( 801.1904061080336987, -452.0891481129646650, 368.3070685750235498 ) ) ;
#37345 = VECTOR ( 'NONE', #10676, 1000.000000000000000 ) ;
#37347 = CARTESIAN_POINT ( 'NONE',  ( 759.9999999999992042, -462.9681489794448339, -309.9999999999998863 ) ) ;
#37346 = DIRECTION ( 'NONE',  ( 0.000000000000000000, 0.000000000000000000, 1.000000000000000000 ) ) ;
#37348 = CARTESIAN_POINT ( 'NONE',  ( 786.2694204179717872, -117.2817908451530684, -305.1769319972829067 ) ) ;
#37349 = DIRECTION ( 'NONE',  ( 0.000000000000000000, -1.000000000000000000, 0.000000000000000000 ) ) ;
#37350 = DIRECTION ( 'NONE',  ( 0.000000000000000000, -6.938893903907222461E-16, 1.000000000000000000 ) ) ;
#37351 = CARTESIAN_POINT ( 'NONE',  ( 760.7433823573367135, -324.0090635724251911, 355.9930595647440441 ) ) ;
#37352 = CARTESIAN_POINT ( 'NONE',  ( 797.6776695296629214, -187.5436935675108430, 357.6776695296636603 ) ) ;
#37353 = ORIENTED_EDGE ( 'NONE', *, *, #30641, .F. ) ;
#37354 = CARTESIAN_POINT ( 'NONE',  ( 745.5313806188320314, -303.2817908451525000, 333.7943932421247268 ) ) ;
#37355 = CARTESIAN_POINT ( 'NONE',  ( 754.9967657858570647, -169.5436935675108998, -365.0032342141425943 ) ) ;
#37356 = FACE_OUTER_BOUND ( 'NONE', #28369, .T. ) ;
#37357 = CARTESIAN_POINT ( 'NONE',  ( 809.0717654672305343, -124.9181544815167086, 360.1688906516309885 ) ) ;
#37358 = CARTESIAN_POINT ( 'NONE',  ( 745.7998596910086917, -293.3618753856923718, -332.5602148656461168 ) ) ;
#37359 = ADVANCED_FACE ( 'NONE', ( #32141 ), #21509, .F. ) ;
#37360 = CARTESIAN_POINT ( 'NONE',  ( 772.5602148656447525, -441.7255117493282910, -305.7998596910095443 ) ) ;
#37361 = CARTESIAN_POINT ( 'NONE',  ( 788.8264449731200330, -165.1800572038745258, 363.6646147819171233 ) ) ;
#37362 = ORIENTED_EDGE ( 'NONE', *, *, #28918, .T. ) ;
#37363 = CARTESIAN_POINT ( 'NONE',  ( 766.4474001241216001, -403.0999726633339719, 307.3154664389482491 ) ) ;
#37364 = CARTESIAN_POINT ( 'NONE',  ( 801.9858362298568863, -339.0783235625956422, -312.7379699480935642 ) ) ;
#37365 = CARTESIAN_POINT ( 'NONE',  ( 745.4481719005789273, -99.72551174932928575, -347.5162901302853129 ) ) ;
#37366 = CARTESIAN_POINT ( 'NONE',  ( 755.1538015810308480, -62.19088175424416676, 343.0433043558613804 ) ) ;
#37367 = CARTESIAN_POINT ( 'NONE',  ( 801.1904061080336987, -380.0891481129646650, -368.3070685750235498 ) ) ;
#37368 = DIRECTION ( 'NONE',  ( 1.000000000000000000, 0.000000000000000000, -0.000000000000000000 ) ) ;
#37369 = CARTESIAN_POINT ( 'NONE',  ( 799.4546378042377910, -417.0783235625954148, 356.1575198192848006 ) ) ;
#37370 = EDGE_LOOP ( 'NONE', ( #36476, #38012, #39406, #8552 ) ) ;
#37371 = CARTESIAN_POINT ( 'NONE',  ( 789.9200121543843807, -73.98741447168741558, 317.0176451133914384 ) ) ;
#37372 = VECTOR ( 'NONE', #16266, 1000.000000000000114 ) ;
#37373 = EDGE_CURVE ( 'NONE', #11665, #2904, #24973, .T. ) ;
#37374 = VECTOR ( 'NONE', #28611, 1000.000000000000114 ) ;
#37375 = CARTESIAN_POINT ( 'NONE',  ( 791.1614460488616487, -107.2601417444145824, -373.5763878283158874 ) ) ;
#37376 = FACE_OUTER_BOUND ( 'NONE', #6456, .T. ) ;
#37377 = CARTESIAN_POINT ( 'NONE',  ( 815.0009284576459549, -270.3510508353231216, 338.7629533639073429 ) ) ;
#37378 = CARTESIAN_POINT ( 'NONE',  ( 754.8072714833583632, -76.81642084023847872, 338.1981804954721156 ) ) ;
#37379 = ORIENTED_EDGE ( 'NONE', *, *, #15407, .T. ) ;
#37380 = AXIS2_PLACEMENT_3D ( 'NONE', #26816, #40921, #33308 ) ;
#37381 = CARTESIAN_POINT ( 'NONE',  ( 803.4237431249931660, -279.1800572038741848, 331.2633955100225194 ) ) ;
#37382 = VECTOR ( 'NONE', #14066, 1000.000000000000000 ) ;
#37383 = CARTESIAN_POINT ( 'NONE',  ( 812.6845335610512393, -439.9874144716862929, -353.5525998758768651 ) ) ;
#37384 = CARTESIAN_POINT ( 'NONE',  ( 775.4999999999993179, -501.1515549466498669, -368.0974687824633520 ) ) ;
#37385 = EDGE_CURVE ( 'NONE', #37268, #23506, #35589, .T. ) ;
#37386 = ORIENTED_EDGE ( 'NONE', *, *, #7500, .F. ) ;
#37387 = ORIENTED_EDGE ( 'NONE', *, *, #43236, .T. ) ;
#37388 = CARTESIAN_POINT ( 'NONE',  ( 793.5525998758768083, -367.0999726633342561, -372.6845335610516941 ) ) ;
#37389 = EDGE_CURVE ( 'NONE', #40120, #13363, #35296, .T. ) ;
#37390 = CARTESIAN_POINT ( 'NONE',  ( 781.8018195045266339, -238.2709662947833920, -365.1927285166406705 ) ) ;
#37392 = CARTESIAN_POINT ( 'NONE',  ( 758.0141637701419768, -231.0783235625960401, 367.2620300519063790 ) ) ;
#37391 = CARTESIAN_POINT ( 'NONE',  ( 772.5602148656447525, -321.7255117493286320, 305.7998596910095443 ) ) ;
#37393 = EDGE_CURVE ( 'NONE', #14073, #30422, #39781, .T. ) ;
#37394 = CARTESIAN_POINT ( 'NONE',  ( 802.5472867521000353, -220.3726999360618208, -350.8726784830461156 ) ) ;
#37395 = CARTESIAN_POINT ( 'NONE',  ( 765.0180583372156207, -216.9982390220562252, -360.0135310231089534 ) ) ;
#37396 = CARTESIAN_POINT ( 'NONE',  ( 795.1360043628808398, -404.0891481129646650, -360.2193346964456282 ) ) ;
#37397 = ORIENTED_EDGE ( 'NONE', *, *, #37429, .F. ) ;
#37398 = CARTESIAN_POINT ( 'NONE',  ( 767.8955696845333705, -216.4527844766016926, 362.1676090361162323 ) ) ;
#37399 = CARTESIAN_POINT ( 'NONE',  ( 802.1676090361156639, -110.6346026584201638, -327.8955696845344505 ) ) ;
#37400 = ORIENTED_EDGE ( 'NONE', *, *, #27454, .T. ) ;
#37401 = CARTESIAN_POINT ( 'NONE',  ( 767.6429770376289525, -369.1800572038739574, 306.8695393053162093 ) ) ;
#37402 = CARTESIAN_POINT ( 'NONE',  ( 829.9999999999992042, 579.9999999999998863, -320.0000000000000000 ) ) ;
#37403 = CARTESIAN_POINT ( 'NONE',  ( 795.2260422076361692, 16.45630643248849978, 314.2591110605560516 ) ) ;
#37404 = CARTESIAN_POINT ( 'NONE',  ( 779.9999999999992042, 126.4563064324884465, 339.9999999999999432 ) ) ;
#37405 = CARTESIAN_POINT ( 'NONE',  ( 802.5472867521000353, -220.3726999360618208, 350.8726784830461156 ) ) ;
#37406 = CARTESIAN_POINT ( 'NONE',  ( 804.6798772138708955, -87.72551174932937101, 334.6312213355107019 ) ) ;
#37407 = CARTESIAN_POINT ( 'NONE',  ( 745.5313806188320314, -447.2817908451521021, -333.7943932421247268 ) ) ;
#37408 = CARTESIAN_POINT ( 'NONE',  ( 767.7687537140311633, -47.90732993114767169, -372.7932403749916830 ) ) ;
#37409 = CARTESIAN_POINT ( 'NONE',  ( 805.0264073115434940, -270.3510508353231216, 339.4763451958999099 ) ) ;
#37410 = VECTOR ( 'NONE', #33569, 1000.000000000000000 ) ;
#37411 = CARTESIAN_POINT ( 'NONE',  ( 805.1927285166397041, -424.8164208402372992, -341.8018195045277707 ) ) ;
#37412 = CARTESIAN_POINT ( 'NONE',  ( 768.0187753319979720, -8.634602658420517329, -318.0580252608186242 ) ) ;
#37413 = ADVANCED_FACE ( 'NONE', ( #22194 ), #28685, .F. ) ;
#37414 = CARTESIAN_POINT ( 'NONE',  ( 758.8095938919642549, -440.0891481129644944, 311.6929314249763365 ) ) ;
#37415 = CARTESIAN_POINT ( 'NONE',  ( 441.1634899080286232, 259.9999999999999432, -199.9999999999972431 ) ) ;
#37416 = CARTESIAN_POINT ( 'NONE',  ( 796.9571628226829034, -287.4636090269708575, -321.2382568024804641 ) ) ;
#37417 = CARTESIAN_POINT ( 'NONE',  ( 749.2812353651451076, -174.4527844766018063, -323.2262854647983090 ) ) ;
#37418 = EDGE_CURVE ( 'NONE', #20722, #5854, #15290, .T. ) ;
#37419 = CARTESIAN_POINT ( 'NONE',  ( 792.2312462859673587, -83.90732993114754379, 307.2067596250082602 ) ) ;
#37420 = CARTESIAN_POINT ( 'NONE',  ( 745.0891759886404770, -148.2709662947837330, 342.4968714119734159 ) ) ;
#37421 = CARTESIAN_POINT ( 'NONE',  ( 791.3765159950071393, 16.45630643248849623, -314.4691821868552211 ) ) ;
#37422 = CARTESIAN_POINT ( 'NONE',  ( 779.9999999999992042, 16.45630643248849267, 309.9999999999998863 ) ) ;
#37423 = CARTESIAN_POINT ( 'NONE',  ( 803.8556311672234642, -225.6237781080506011, -365.6418435158340117 ) ) ;
#37424 = CARTESIAN_POINT ( 'NONE',  ( 752.7379699480933368, -420.0090635724249069, 361.9858362298580232 ) ) ;
#37425 = DIRECTION ( 'NONE',  ( -0.000000000000000000, 1.000000000000000000, -0.000000000000000000 ) ) ;
#37426 = CARTESIAN_POINT ( 'NONE',  ( 801.1904061080336987, -404.0891481129646081, 368.3070685750235498 ) ) ;
#37427 = CARTESIAN_POINT ( 'NONE',  ( 812.7932403749906598, -15.18005720387504631, 327.7687537140311633 ) ) ;
#37428 = CARTESIAN_POINT ( 'NONE',  ( 774.6312213355099630, -359.3618753856920875, -364.6798772138717482 ) ) ;
#37429 = EDGE_CURVE ( 'NONE', #8747, #34761, #42763, .T. ) ;
#37430 = CARTESIAN_POINT ( 'NONE',  ( 759.2295555964440155, 7.830767346494148740, 353.9708237608231229 ) ) ;
#37431 = CARTESIAN_POINT ( 'NONE',  ( 749.5768839229115201, -108.5545181178803915, -358.0661480581553064 ) ) ;
#37432 = CARTESIAN_POINT ( 'NONE',  ( 756.1348686366196716, -161.2601417444143976, -347.5531968255698416 ) ) ;
#37433 = CARTESIAN_POINT ( 'NONE',  ( 810.1134526219336749, -176.5328690171416213, 357.8822607201570349 ) ) ;
#37434 = DIRECTION ( 'NONE',  ( 1.892425610156518354E-16, 1.000000000000000000, -0.000000000000000000 ) ) ;
#37435 = CARTESIAN_POINT ( 'NONE',  ( 762.3223304703356007, -79.54369356751119824, -322.3223304703362828 ) ) ;
#37436 = CARTESIAN_POINT ( 'NONE',  ( 803.8651313633788504, -149.2601417444144261, -332.4468031744301015 ) ) ;
#37437 = CARTESIAN_POINT ( 'NONE',  ( 759.7806653035534055, -174.9982390220563673, 324.8639956371180801 ) ) ;
#37438 = CARTESIAN_POINT ( 'NONE',  ( 795.6651683502461765, -10.71468719896033761, -371.3240766477733814 ) ) ;
#37440 = CARTESIAN_POINT ( 'NONE',  ( 803.4237431249931660, -279.1800572038741848, 331.2633955100225194 ) ) ;
#37439 = CARTESIAN_POINT ( 'NONE',  ( 762.1405469898971887, -289.5436935675103882, 357.8594530101015607 ) ) ;
#37441 = CARTESIAN_POINT ( 'NONE',  ( 786.4999999999993179, -434.0043448692482002, 397.6917108626901154 ) ) ;
#37442 = ORIENTED_EDGE ( 'NONE', *, *, #19077, .T. ) ;
#37443 = CARTESIAN_POINT ( 'NONE',  ( 754.9735926884551418, -18.35105083532395298, 340.5236548041000333 ) ) ;
#37444 = CARTESIAN_POINT ( 'NONE',  ( 812.3518521366052028, -265.0999726633344267, -326.5853460496235243 ) ) ;
#37445 = VECTOR ( 'NONE', #35856, 1000.000000000000000 ) ;
#37446 = ORIENTED_EDGE ( 'NONE', *, *, #42732, .F. ) ;
#37447 = DIRECTION ( 'NONE',  ( 0.000000000000000000, 0.000000000000000000, 1.000000000000000000 ) ) ;
#37448 = CARTESIAN_POINT ( 'NONE',  ( 800.9747183278959710, -228.9982390220561683, 311.9810565676471583 ) ) ;
#37449 = CARTESIAN_POINT ( 'NONE',  ( 783.0745993439762742, -296.1908817542434917, 365.1016975059196739 ) ) ;
#37450 = CARTESIAN_POINT ( 'NONE',  ( 803.8651313633788504, -413.2601417444136018, 332.4468031744301015 ) ) ;
#37451 = ORIENTED_EDGE ( 'NONE', *, *, #5821, .F. ) ;
#37452 = CARTESIAN_POINT ( 'NONE',  ( 793.9708237608222134, -118.9181544815167229, -319.2295555964448681 ) ) ;
#37453 = CARTESIAN_POINT ( 'NONE',  ( 795.1360043628807261, -116.0891481129656029, -360.2193346964456282 ) ) ;
#37454 = CARTESIAN_POINT ( 'NONE',  ( 795.1360043628808398, -308.0891481129650629, -360.2193346964456282 ) ) ;
#37455 = VERTEX_POINT ( 'NONE', #11124 ) ;
#37456 = CARTESIAN_POINT ( 'NONE',  ( 755.0636971347428243, -436.2709662947827951, -341.7834795799807353 ) ) ;
#37457 = CARTESIAN_POINT ( 'NONE',  ( 769.1273215169530886, -286.7146871989594388, 317.4527132478988847 ) ) ;
#37458 = CARTESIAN_POINT ( 'NONE',  ( 758.7867965644026071, 16.45630643248849267, 318.7867965644036303 ) ) ;
#37459 = LINE ( 'NONE', #31204, #9362 ) ;
#37460 = DIRECTION ( 'NONE',  ( -1.000000000000000000, -1.644774851296528363E-16, 0.000000000000000000 ) ) ;
#37461 = ORIENTED_EDGE ( 'NONE', *, *, #40197, .T. ) ;
#37462 = CARTESIAN_POINT ( 'NONE',  ( 810.4231160770870019, -360.5545181178796383, -321.9338519418446936 ) ) ;
#37463 = CARTESIAN_POINT ( 'NONE',  ( 783.7953271457878373, -200.1908817542436907, 375.1787889125761239 ) ) ;
#37464 = CARTESIAN_POINT ( 'NONE',  ( 800.2193346964447755, -306.9982390220558273, -355.1360043628815788 ) ) ;
#37465 = ADVANCED_FACE ( 'NONE', ( #8132 ), #30887, .F. ) ;
#37466 = PRESENTATION_STYLE_ASSIGNMENT (( #30522 ) ) ;
#37467 = CARTESIAN_POINT ( 'NONE',  ( 805.2837595273609850, -194.7363362996982517, -340.5290396650784714 ) ) ;
#37468 = CARTESIAN_POINT ( 'NONE',  ( 763.2262854647970016, -56.63460265842036279, 309.2812353651462445 ) ) ;
#37469 = DIRECTION ( 'NONE',  ( 0.000000000000000000, 0.000000000000000000, -1.000000000000000000 ) ) ;
#37470 = CARTESIAN_POINT ( 'NONE',  ( 812.7932403749906598, -399.1800572038738437, -327.7687537140311633 ) ) ;
#37471 = FACE_OUTER_BOUND ( 'NONE', #18770, .T. ) ;
#37472 = CARTESIAN_POINT ( 'NONE',  ( 800.2193346964447755, -66.99823902205672255, 355.1360043628815788 ) ) ;
#37473 = CIRCLE ( 'NONE', #33782, 8.024999999999948841 ) ;
#37474 = CARTESIAN_POINT ( 'NONE',  ( 768.9521613784389729, -321.8272453906070609, 373.2346286133773106 ) ) ;
#37475 = DIRECTION ( 'NONE',  ( -1.880165489482579047E-16, -1.000000000000000000, -0.000000000000000000 ) ) ;
#37476 = CARTESIAN_POINT ( 'NONE',  ( 796.9462024416508257, -300.4527844766012663, 308.9653473494370246 ) ) ;
#37477 = CARTESIAN_POINT ( 'NONE',  ( 782.4968714119720516, -34.81642084023861372, -305.0891759886411023 ) ) ;
#37478 = CARTESIAN_POINT ( 'NONE',  ( 778.2165204200184689, -262.8164208402379245, -364.9363028652563230 ) ) ;
#37479 = FACE_OUTER_BOUND ( 'NONE', #7937, .T. ) ;
#37480 = CARTESIAN_POINT ( 'NONE',  ( 785.3141322388236176, -357.7255117493285184, 364.4286716492789537 ) ) ;
#37481 = CARTESIAN_POINT ( 'NONE',  ( 780.5236548040995785, -116.7363362996985217, 314.9735926884559944 ) ) ;
#37482 = CARTESIAN_POINT ( 'NONE',  ( 796.7845633553578182, -57.62377810805111267, -358.5707757039688204 ) ) ;
#37483 = CARTESIAN_POINT ( 'NONE',  ( 781.2497674668890113, -36.35105083532390324, 375.3608509340180603 ) ) ;
#37484 = CARTESIAN_POINT ( 'NONE',  ( 756.5762568750052424, -363.1800572038739006, 348.7366044899774238 ) ) ;
#37485 = CARTESIAN_POINT ( 'NONE',  ( 831.1634899080286232, 239.9999999999998863, -197.2500000000000853 ) ) ;
#37486 = SURFACE_STYLE_USAGE ( .BOTH. , #2602 ) ;
#37487 = CARTESIAN_POINT ( 'NONE',  ( 755.0636971347428243, -436.2709662947827951, 341.7834795799807353 ) ) ;
#37488 = ORIENTED_EDGE ( 'NONE', *, *, #30882, .F. ) ;
#37489 = CARTESIAN_POINT ( 'NONE',  ( 759.2295555964440155, -376.1692326535046504, -353.9708237608231229 ) ) ;
#37491 = CARTESIAN_POINT ( 'NONE',  ( 797.6776695296629214, -187.5436935675108430, 357.6776695296636603 ) ) ;
#37490 = CARTESIAN_POINT ( 'NONE',  ( 802.1676090361156639, -182.6346026584199649, 327.8955696845344505 ) ) ;
#37492 = CARTESIAN_POINT ( 'NONE',  ( 771.2368401574024119, -373.4419599262319593, -374.2805881961240857 ) ) ;
#37493 = DIRECTION ( 'NONE',  ( -1.000000000000000000, 0.000000000000000000, 0.000000000000000000 ) ) ;
#37494 = ORIENTED_EDGE ( 'NONE', *, *, #32600, .T. ) ;
#37495 = CARTESIAN_POINT ( 'NONE',  ( 764.8639956371174549, -392.0891481129648355, 319.7806653035542013 ) ) ;
#37496 = ORIENTED_EDGE ( 'NONE', *, *, #25320, .F. ) ;
#37497 =( NAMED_UNIT ( * ) PLANE_ANGLE_UNIT ( ) SI_UNIT ( $, .RADIAN. ) );
#37498 = CARTESIAN_POINT ( 'NONE',  ( 763.2262854647970016, -200.6346026584199365, -309.2812353651462445 ) ) ;
#37499 = CARTESIAN_POINT ( 'NONE',  ( 800.9747183278959710, -132.9982390220564810, 311.9810565676471583 ) ) ;
#37500 = ORIENTED_EDGE ( 'NONE', *, *, #15904, .F. ) ;
#37501 = CARTESIAN_POINT ( 'NONE',  ( 757.8323909638828582, -194.6346026584199080, -352.1044303154654358 ) ) ;
#37502 = ORIENTED_EDGE ( 'NONE', *, *, #35704, .F. ) ;
#37503 = AXIS2_PLACEMENT_3D ( 'NONE', #36287, #7661, #22409 ) ;
#37504 = CARTESIAN_POINT ( 'NONE',  ( 800.0135310231082713, -326.0891481129649492, -325.0180583372163028 ) ) ;
#37505 = CARTESIAN_POINT ( 'NONE',  ( 794.9819416627830151, 11.00176097794305541, -319.9864689768909898 ) ) ;
#37506 = CARTESIAN_POINT ( 'NONE',  ( 745.0891759886404770, -244.2709662947834204, 342.4968714119734159 ) ) ;
#37507 = CARTESIAN_POINT ( 'NONE',  ( 766.7756240680305382, -182.5328690171416497, 361.5560724626415663 ) ) ;
#37509 = CARTESIAN_POINT ( 'NONE',  ( 914.9999999999992042, 74.99999999999984368, -360.0000000000000000 ) ) ;
#37508 = FACE_OUTER_BOUND ( 'NONE', #5337, .T. ) ;
#37510 = FACE_OUTER_BOUND ( 'NONE', #34991, .T. ) ;
#37511 = ORIENTED_EDGE ( 'NONE', *, *, #2688, .T. ) ;
#37512 = CARTESIAN_POINT ( 'NONE',  ( 780.5236548040995785, -452.7363362996975411, -314.9735926884559944 ) ) ;
#37513 = CARTESIAN_POINT ( 'NONE',  ( 779.9999999999990905, 18.49609980828599376, -309.9999999999999432 ) ) ;
#37514 = CARTESIAN_POINT ( 'NONE',  ( 767.9999999999992042, 205.0000000000000568, -319.9999999999999432 ) ) ;
#37515 = ORIENTED_EDGE ( 'NONE', *, *, #29530, .T. ) ;
#37516 = CARTESIAN_POINT ( 'NONE',  ( 815.3608509340175488, -242.7363362996980811, -341.2497674668889545 ) ) ;
#37517 = CARTESIAN_POINT ( 'NONE',  ( 757.7880784355613741, -114.0090635724258163, 312.4576283171834916 ) ) ;
#37519 = CARTESIAN_POINT ( 'NONE',  ( 767.8955696845333705, -192.4527844766016926, -362.1676090361162323 ) ) ;
#37518 = CARTESIAN_POINT ( 'NONE',  ( -598.8365100919716042, 240.0000000000001705, -202.7499999999898250 ) ) ;
#37520 = CARTESIAN_POINT ( 'NONE',  ( 761.2382568024794409, -375.6237781080501463, -356.9571628226838129 ) ) ;
#37521 = CARTESIAN_POINT ( 'NONE',  ( 755.8990559732751535, -227.4636090269709143, -365.9055244015606831 ) ) ;
#37522 = LINE ( 'NONE', #5406, #16370 ) ;
#37523 = CARTESIAN_POINT ( 'NONE',  ( 454.7528517110262101, 199.9999999999999432, 339.9999999999999432 ) ) ;
#37524 = CARTESIAN_POINT ( 'NONE',  ( 779.4763451958990572, -80.73633629969864955, -365.0264073115438919 ) ) ;
#37525 = CARTESIAN_POINT ( 'NONE',  ( 769.0155153010367712, -418.3726999360612808, 362.7791456095907279 ) ) ;
#37526 = DIRECTION ( 'NONE',  ( 0.000000000000000000, 0.000000000000000000, 1.000000000000000000 ) ) ;
#37527 = CARTESIAN_POINT ( 'NONE',  ( 790.8726784830453198, -418.7146871989590409, -362.5472867521010585 ) ) ;
#37528 = CARTESIAN_POINT ( 'NONE',  ( 749.2812353651451076, -270.4527844766014937, -323.2262854647983090 ) ) ;
#37529 = DIRECTION ( 'NONE',  ( 1.892425610156518354E-16, 1.000000000000000000, -0.000000000000000000 ) ) ;
#37530 = LINE ( 'NONE', #42134, #25366 ) ;
#37531 = CARTESIAN_POINT ( 'NONE',  ( 765.0180583372156207, -48.99823902205675807, -360.0135310231089534 ) ) ;
#37532 = CARTESIAN_POINT ( 'NONE',  ( 788.6739635108323228, -223.6454272087891013, 373.9316612368139090 ) ) ;
#37533 = CARTESIAN_POINT ( 'NONE',  ( 758.0141637701419768, -159.0783235625962391, -367.2620300519063790 ) ) ;
#37534 = CARTESIAN_POINT ( 'NONE',  ( 754.9967657858570647, -169.5436935675108430, 365.0032342141425374 ) ) ;
#37535 = CARTESIAN_POINT ( 'NONE',  ( 751.9810565676468741, -410.0891481129647218, -360.9747183278973921 ) ) ;
#37536 = CARTESIAN_POINT ( 'NONE',  ( 998.9999999999992042, 479.9999999999999432, 360.0000000000000000 ) ) ;
#37537 = CARTESIAN_POINT ( 'NONE',  ( 757.8323909638827445, -266.6346026584197375, 352.1044303154654358 ) ) ;
#37538 = CARTESIAN_POINT ( 'NONE',  ( 786.5483106153019435, -55.64542720878963422, 364.1601925771022366 ) ) ;
#37539 = CARTESIAN_POINT ( 'NONE',  ( 801.9419747391806368, -426.4527844766010389, -351.9812246680014027 ) ) ;
#37540 = VECTOR ( 'NONE', #44582, 1000.000000000000000 ) ;
#37541 = CARTESIAN_POINT ( 'NONE',  ( -919.9999999999993179, 154.9999999999998863, -360.0000000000000000 ) ) ;
#37542 = LINE ( 'NONE', #1973, #45407 ) ;
#37543 = CARTESIAN_POINT ( 'NONE',  ( 794.1144889064781864, -82.16923265350558836, 360.9840315886528401 ) ) ;
#37544 = EDGE_LOOP ( 'NONE', ( #32415, #32034, #12457, #40682 ) ) ;
#37545 = CARTESIAN_POINT ( 'NONE',  ( 756.1348686366196716, -233.2601417444141987, -347.5531968255698416 ) ) ;
#37546 = CARTESIAN_POINT ( 'NONE',  ( 762.1405469898971887, -73.54369356751118403, 357.8594530101015607 ) ) ;
#37547 = CARTESIAN_POINT ( 'NONE',  ( 746.0683387631852383, -259.4419599262322436, -331.3260364891676204 ) ) ;
#37548 = DIRECTION ( 'NONE',  ( 0.000000000000000000, 1.000000000000000000, -1.110223024625155554E-15 ) ) ;
#37549 = CARTESIAN_POINT ( 'NONE',  ( 752.4576283171824116, -381.0783235625954717, 317.7880784355627952 ) ) ;
#37550 = ORIENTED_EDGE ( 'NONE', *, *, #18226, .F. ) ;
#37551 = CARTESIAN_POINT ( 'NONE',  ( 797.8594530101008786, -181.5436935675108145, -322.1405469898980982 ) ) ;
#37552 = CARTESIAN_POINT ( 'NONE',  ( 755.0636971347428243, -388.2709662947829656, 341.7834795799807353 ) ) ;
#37553 = CARTESIAN_POINT ( 'NONE',  ( 754.9967657858570647, -121.5436935675110419, -365.0032342141425374 ) ) ;
#37554 = CARTESIAN_POINT ( 'NONE',  ( 803.6646147819162707, -65.90732993114760063, -348.8264449731211130 ) ) ;
#37555 = EDGE_LOOP ( 'NONE', ( #35117, #27737, #41506, #9174 ) ) ;
#37556 = CARTESIAN_POINT ( 'NONE',  ( 755.1538015810308480, -62.19088175424416676, -343.0433043558613804 ) ) ;
#37557 = VERTEX_POINT ( 'NONE', #7910 ) ;
#37558 = CARTESIAN_POINT ( 'NONE',  ( 790.9844846989617508, -358.3726999360613945, -317.2208543904092721 ) ) ;
#37560 = CARTESIAN_POINT ( 'NONE',  ( 769.0155153010367712, -394.3726999360613377, 362.7791456095907279 ) ) ;
#37559 = CARTESIAN_POINT ( 'NONE',  ( 758.0580252608178853, -102.4527844766020337, 328.0187753319985404 ) ) ;
#37561 = CARTESIAN_POINT ( 'NONE',  ( 789.9200121543843807, -97.98741447168734453, 317.0176451133914384 ) ) ;
#37564 = CARTESIAN_POINT ( 'NONE',  ( 744.8212110874229666, -354.8965053807774552, 336.2046728542121627 ) ) ;
#37563 = FACE_OUTER_BOUND ( 'NONE', #37897, .T. ) ;
#37562 = CARTESIAN_POINT ( 'NONE',  ( 811.0346526505617248, -446.6346026584191122, 323.0537975583478101 ) ) ;
#37565 = CARTESIAN_POINT ( 'NONE',  ( 804.8461984189677878, -314.1908817542433781, -336.9566956441385628 ) ) ;
#37566 = CARTESIAN_POINT ( 'NONE',  ( 805.1927285166397041, -328.8164208402375834, -341.8018195045277707 ) ) ;
#37567 = CARTESIAN_POINT ( 'NONE',  ( 788.6739635108323228, -127.6454272087894140, -373.9316612368139090 ) ) ;
#37568 = ADVANCED_BREP_SHAPE_REPRESENTATION ( '', ( #1937, #26858 ), #7608 ) ;
#37569 = CARTESIAN_POINT ( 'NONE',  ( 787.5162901302840055, -443.3618753856917465, 305.4481719005792684 ) ) ;
#37571 = DIRECTION ( 'NONE',  ( 0.000000000000000000, 0.000000000000000000, -1.000000000000000000 ) ) ;
#37570 = CARTESIAN_POINT ( 'NONE',  ( 879.9999999999992042, 239.9999999999998863, -244.9999999999999716 ) ) ;
#37572 = CARTESIAN_POINT ( 'NONE',  ( 805.0264073115434940, -270.3510508353231216, -339.4763451958999099 ) ) ;
#37573 = CARTESIAN_POINT ( 'NONE',  ( 797.8822607201568644, -126.5545181178803205, -370.1134526219340160 ) ) ;
#37574 = DIRECTION ( 'NONE',  ( 0.000000000000000000, 0.000000000000000000, 1.000000000000000000 ) ) ;
#37575 = DIRECTION ( 'NONE',  ( -0.000000000000000000, 1.000000000000000000, -0.000000000000000000 ) ) ;
#37576 = CARTESIAN_POINT ( 'NONE',  ( 786.5483106153019435, -319.6454272087888739, 364.1601925771022366 ) ) ;
#37577 = CARTESIAN_POINT ( 'NONE',  ( 781.8018195045266339, -190.2709662947835909, 365.1927285166406705 ) ) ;
#37578 = VERTEX_POINT ( 'NONE', #1180 ) ;
#37579 = CARTESIAN_POINT ( 'NONE',  ( 812.3518521366052028, -289.0999726633343698, 326.5853460496235243 ) ) ;
#37580 = EDGE_CURVE ( 'NONE', #7814, #24322, #39014, .T. ) ;
#37581 = CARTESIAN_POINT ( 'NONE',  ( 805.0032342141413437, -157.5436935675109282, -314.9967657858572352 ) ) ;
#37582 = CARTESIAN_POINT ( 'NONE',  ( 181.1634899080285948, 260.0000000000000000, -199.9999999999953957 ) ) ;
#37583 = CARTESIAN_POINT ( 'NONE',  ( 811.3240766477731540, -100.3726999360622187, 355.6651683502462902 ) ) ;
#37584 = CARTESIAN_POINT ( 'NONE',  ( 745.4481719005789273, -315.7255117493286320, -347.5162901302853129 ) ) ;
#37585 = FACE_OUTER_BOUND ( 'NONE', #22591, .T. ) ;
#37586 = CARTESIAN_POINT ( 'NONE',  ( 785.3141322388236176, -165.7255117493291152, 364.4286716492789537 ) ) ;
#37587 = ORIENTED_EDGE ( 'NONE', *, *, #20468, .F. ) ;
#37588 = CARTESIAN_POINT ( 'NONE',  ( 750.9282345327678740, -424.9181544815158986, 319.8311093483690115 ) ) ;
#37589 = CARTESIAN_POINT ( 'NONE',  ( 746.7653713866222915, -353.2601417444137724, -351.0478386215610271 ) ) ;
#37590 = CARTESIAN_POINT ( 'NONE',  ( 755.2512626584698410, -127.5436935675110561, -315.2512626584710915 ) ) ;
#37591 = CARTESIAN_POINT ( 'NONE',  ( 772.4468031744293057, -33.82724539060788516, 363.8651313633793620 ) ) ;
#37592 = CARTESIAN_POINT ( 'NONE',  ( 796.9462024416508257, -372.4527844766010958, -308.9653473494370246 ) ) ;
#37593 = FACE_OUTER_BOUND ( 'NONE', #18724, .T. ) ;
#37594 = CARTESIAN_POINT ( 'NONE',  ( 764.3348316497523456, 25.28531280103955226, 308.6759233522265617 ) ) ;
#37595 = VERTEX_POINT ( 'NONE', #25193 ) ;
#37596 = CARTESIAN_POINT ( 'NONE',  ( 794.1144889064781864, -82.16923265350558836, 360.9840315886528401 ) ) ;
#37597 = EDGE_CURVE ( 'NONE', #41202, #32812, #39306, .T. ) ;
#37598 = CARTESIAN_POINT ( 'NONE',  ( 801.9858362298568863, -171.0783235625962106, -312.7379699480935642 ) ) ;
#37599 = DIRECTION ( 'NONE',  ( -0.000000000000000000, -0.3826834323650838976, -0.9238795325112892920 ) ) ;
#37600 = CARTESIAN_POINT ( 'NONE',  ( 749.8865473780648472, -284.5328690171412518, 322.1177392798429082 ) ) ;
#37601 = CARTESIAN_POINT ( 'NONE',  ( 792.1044303154646968, -84.45278447660207632, 317.8323909638837677 ) ) ;
#37602 = VERTEX_POINT ( 'NONE', #18305 ) ;
#37603 = CARTESIAN_POINT ( 'NONE',  ( 756.7813123517142913, 4.012585528312341054, -329.9779781133712504 ) ) ;
#37604 = CARTESIAN_POINT ( 'NONE',  ( 785.3141322388236176, -261.7255117493288026, 364.4286716492789537 ) ) ;
#37605 = CARTESIAN_POINT ( 'NONE',  ( 807.5423716828161105, -441.0783235625953580, -362.2119215644372048 ) ) ;
#37606 = FACE_BOUND ( 'NONE', #37970, .T. ) ;
#37607 = ORIENTED_EDGE ( 'NONE', *, *, #11433, .T. ) ;
#37608 = ORIENTED_EDGE ( 'NONE', *, *, #20712, .T. ) ;
#37609 = CARTESIAN_POINT ( 'NONE',  ( 813.5763878283155464, -387.8272453906067767, -351.1614460488615350 ) ) ;
#37611 = CARTESIAN_POINT ( 'NONE',  ( 798.0661480581538854, -266.5328690171413655, 309.5768839229118043 ) ) ;
#37610 = CARTESIAN_POINT ( 'NONE',  ( 814.2001403089898304, -329.3618753856922581, 347.4397851343538264 ) ) ;
#37612 = EDGE_CURVE ( 'NONE', #44144, #16382, #735, .T. ) ;
#37613 = CARTESIAN_POINT ( 'NONE',  ( 790.0220218866281812, -223.0999726633346256, -363.2186876482849129 ) ) ;
#37614 = CARTESIAN_POINT ( 'NONE',  ( 804.4286716492782716, -209.3618753856926276, -345.3141322388244703 ) ) ;
#37615 = CARTESIAN_POINT ( 'NONE',  ( 778.2165204200184689, -430.8164208402374129, -364.9363028652563230 ) ) ;
#37616 = CARTESIAN_POINT ( 'NONE',  ( 804.9363028652555840, -208.2709662947835341, 338.2165204200192079 ) ) ;
#37617 = CARTESIAN_POINT ( 'NONE',  ( 762.1405469898971887, -97.54369356751112718, -357.8594530101015607 ) ) ;
#37618 = VERTEX_POINT ( 'NONE', #32383 ) ;
#37619 = CARTESIAN_POINT ( 'NONE',  ( 754.9967657858570647, -361.5436935675103882, 365.0032342141425374 ) ) ;
#37620 = CARTESIAN_POINT ( 'NONE',  ( 180.7583438952258916, 294.6698570112193920, -274.9999999999999432 ) ) ;
#37621 = CARTESIAN_POINT ( 'NONE',  ( 776.2046728542105711, -20.19088175424429110, -304.8212110874238761 ) ) ;
#37622 = CARTESIAN_POINT ( 'NONE',  ( 772.8365271371600329, 16.45630643248849267, 315.6518837687410723 ) ) ;
#37623 = CARTESIAN_POINT ( 'NONE',  ( -78.83651009197140525, 230.0000000000000568, -202.7499999999934346 ) ) ;
#37624 = EDGE_CURVE ( 'NONE', #20178, #18957, #25670, .T. ) ;
#37625 = CARTESIAN_POINT ( 'NONE',  ( 766.9102291470427417, -234.5545181178799794, 318.6633372737382501 ) ) ;
#37626 = CARTESIAN_POINT ( 'NONE',  ( 791.9812246680005501, -92.63460265842026331, 361.9419747391813189 ) ) ;
#37627 = EDGE_LOOP ( 'NONE', ( #8759, #20355 ) ) ;
#37628 = CARTESIAN_POINT ( 'NONE',  ( 807.2620300519052989, -432.0090635724247932, -318.0141637701419768 ) ) ;
#37629 = CARTESIAN_POINT ( 'NONE',  ( 744.7301800767020268, -76.81642084023847872, -337.4774526936615189 ) ) ;
#37630 = CARTESIAN_POINT ( 'NONE',  ( 804.9511171171677688, -245.8055962898686460, 335.8780910478229202 ) ) ;
#37631 = CARTESIAN_POINT ( 'NONE',  ( 774.6312213355099630, -431.3618753856918033, -364.6798772138717482 ) ) ;
#37632 = CARTESIAN_POINT ( 'NONE',  ( 768.0187753319979720, -32.63460265842044095, -318.0580252608186242 ) ) ;
#37633 = CARTESIAN_POINT ( 'NONE',  ( 804.1009440267234822, 0.5363909730283709099, 314.0944755984392600 ) ) ;
#37634 = CARTESIAN_POINT ( 'NONE',  ( -858.8365100919713768, 260.0000000000002274, -199.9999999999881481 ) ) ;
#37635 = CARTESIAN_POINT ( 'NONE',  ( 804.1105419155481968, -291.8272453906071746, -347.6308680596136469 ) ) ;
#37636 = CARTESIAN_POINT ( 'NONE',  ( 782.4968714119720516, -202.8164208402380950, -305.0891759886411023 ) ) ;
#37637 = CARTESIAN_POINT ( 'NONE',  ( 792.3570229623688874, -69.18005720387488111, 373.1304606946836202 ) ) ;
#37638 = CARTESIAN_POINT ( 'NONE',  ( 749.2812353651451076, -150.4527844766018916, 323.2262854647983090 ) ) ;
#37639 = CARTESIAN_POINT ( 'NONE',  ( 914.9999999999992042, 99.99999999999984368, 350.0000000000000000 ) ) ;
#37640 = FACE_BOUND ( 'NONE', #1804, .T. ) ;
#37641 = EDGE_CURVE ( 'NONE', #38354, #15902, #28907, .T. ) ;
#37642 = CARTESIAN_POINT ( 'NONE',  ( 801.9858362298568863, -243.0783235625959833, -312.7379699480935642 ) ) ;
#37643 = CARTESIAN_POINT ( 'NONE',  ( 791.0478386215596629, -405.8272453906067199, 306.7653713866226326 ) ) ;
#37644 = EDGE_CURVE ( 'NONE', #23168, #13136, #25774, .T. ) ;
#37645 = CARTESIAN_POINT ( 'NONE',  ( 782.4968714119720516, -298.8164208402377540, -305.0891759886411023 ) ) ;
#37646 = DIRECTION ( 'NONE',  ( -0.000000000000000000, 1.000000000000000000, -0.000000000000000000 ) ) ;
#37647 = CARTESIAN_POINT ( 'NONE',  ( 759.0252816721024374, -384.9982390220556567, 368.0189434323527280 ) ) ;
#37648 = CARTESIAN_POINT ( 'NONE',  ( 777.5031285880264704, 1.183579159761269040, 374.9108240113588408 ) ) ;
#37649 = CARTESIAN_POINT ( 'NONE',  ( 778.1981804954714335, -346.2709662947830793, -314.8072714833589885 ) ) ;
#37650 = CARTESIAN_POINT ( 'NONE',  ( 786.6156483768007774, -1.441959926233096656, 315.5913626894246136 ) ) ;
#37651 = EDGE_CURVE ( 'NONE', #8247, #18328, #14834, .T. ) ;
#37652 = CARTESIAN_POINT ( 'NONE',  ( 758.0141637701419768, -39.07832356259662276, -367.2620300519063790 ) ) ;
#37653 = CARTESIAN_POINT ( 'NONE',  ( 798.7617431975189675, -171.6237781080507432, -323.0428371773161871 ) ) ;
#37654 = CARTESIAN_POINT ( 'NONE',  ( 771.2368401574024119, -157.4419599262326130, 374.2805881961240857 ) ) ;
#37655 = FACE_BOUND ( 'NONE', #11650, .T. ) ;
#37656 = ORIENTED_EDGE ( 'NONE', *, *, #352, .F. ) ;
#37657 = CARTESIAN_POINT ( 'NONE',  ( 802.1676090361156639, -62.63460265842031305, -327.8955696845344505 ) ) ;
#37658 = CARTESIAN_POINT ( 'NONE',  ( 754.8983024940795303, -162.8965053807780521, -336.9254006560228163 ) ) ;
#37659 = CARTESIAN_POINT ( 'NONE',  ( 797.8594530101008786, -157.5436935675108998, 322.1405469898980982 ) ) ;
#37660 = PRODUCT_DEFINITION_SHAPE ( 'NONE', 'NONE',  #45728 ) ;
#37661 = CARTESIAN_POINT ( 'NONE',  ( 810.1134526219336749, -8.532869017142163059, -357.8822607201570349 ) ) ;
#37663 = CARTESIAN_POINT ( 'NONE',  ( 802.1676090361155502, -278.6346026584196807, 327.8955696845344505 ) ) ;
#37662 = CARTESIAN_POINT ( 'NONE',  ( 754.8072714833581358, -292.8164208402376971, 338.1981804954720587 ) ) ;
#37664 = FACE_OUTER_BOUND ( 'NONE', #35868, .T. ) ;
#37665 = ORIENTED_EDGE ( 'NONE', *, *, #19631, .F. ) ;
#37666 = CARTESIAN_POINT ( 'NONE',  ( 790.8726784830453198, -10.71468719896033761, 362.5472867521010585 ) ) ;
#37667 = CARTESIAN_POINT ( 'NONE',  ( 771.3260364891663130, -283.6454272087889308, -306.0683387631859773 ) ) ;
#37668 = EDGE_CURVE ( 'NONE', #26480, #8204, #15439, .T. ) ;
#37669 = EDGE_LOOP ( 'NONE', ( #18830, #12172, #11287, #41381 ) ) ;
#37670 = DIRECTION ( 'NONE',  ( 1.000000000000000000, 0.000000000000000000, 0.000000000000000000 ) ) ;
#37671 = CARTESIAN_POINT ( 'NONE',  ( 815.2698199232962679, -232.8164208402379529, 342.5225473063383674 ) ) ;
#37672 = EDGE_CURVE ( 'NONE', #10339, #29708, #27973, .T. ) ;
#37673 = CARTESIAN_POINT ( 'NONE',  ( 800.9840315886518738, -340.9181544815160123, 354.1144889064786412 ) ) ;
#37674 = CARTESIAN_POINT ( 'NONE',  ( 803.2186876482843445, -439.9874144716862929, 350.0220218866286928 ) ) ;
#37675 = ORIENTED_EDGE ( 'NONE', *, *, #39050, .F. ) ;
#37676 = CARTESIAN_POINT ( 'NONE',  ( 755.1538015810308480, -110.1908817542440033, -343.0433043558613804 ) ) ;
#37677 = CARTESIAN_POINT ( 'NONE',  ( 755.0636971347428243, -124.2709662947837899, -341.7834795799807353 ) ) ;
#37678 = CARTESIAN_POINT ( 'NONE',  ( 771.2633955100217236, -311.9073299311468759, -363.4237431249939618 ) ) ;
#37679 = ORIENTED_EDGE ( 'NONE', *, *, #32011, .T. ) ;
#37680 = CARTESIAN_POINT ( 'NONE',  ( 768.0187753319979720, -416.6346026584192259, -318.0580252608186242 ) ) ;
#37681 = CARTESIAN_POINT ( 'NONE',  ( 783.0433043558608688, -312.8965053807775689, 315.1538015810313027 ) ) ;
#37682 = EDGE_CURVE ( 'NONE', #35164, #7841, #30917, .T. ) ;
#37683 = DIRECTION ( 'NONE',  ( 0.000000000000000000, -0.000000000000000000, -1.000000000000000000 ) ) ;
#37684 = DIRECTION ( 'NONE',  ( 0.000000000000000000, 0.000000000000000000, -1.000000000000000000 ) ) ;
#37685 = ADVANCED_FACE ( 'NONE', ( #22644 ), #29589, .F. ) ;
#37686 = CARTESIAN_POINT ( 'NONE',  ( 760.7433823573367135, -108.0090635724258448, 355.9930595647440441 ) ) ;
#37687 = CARTESIAN_POINT ( 'NONE',  ( 803.4237431249931660, 8.819942796124882634, 331.2633955100225194 ) ) ;
#37688 = ORIENTED_EDGE ( 'NONE', *, *, #16791, .F. ) ;
#37689 = CARTESIAN_POINT ( 'NONE',  ( 814.8207195650702488, -338.1908817542433212, -336.2433038121456548 ) ) ;
#37690 = CARTESIAN_POINT ( 'NONE',  ( 781.2370466360911223, -212.7363362996982232, 304.9990715423533629 ) ) ;
#37691 = CARTESIAN_POINT ( 'NONE',  ( 755.0636971347428243, -340.2709662947831362, -341.7834795799807353 ) ) ;
#37692 =( LENGTH_UNIT ( ) NAMED_UNIT ( * ) SI_UNIT ( .MILLI., .METRE. ) );
#37693 = CARTESIAN_POINT ( 'NONE',  ( 804.6971507214547046, -171.2817908451529263, -344.0799538623459739 ) ) ;
#37694 = CARTESIAN_POINT ( 'NONE',  ( 801.1904061080336987, -44.08914811296584446, 368.3070685750235498 ) ) ;
#37695 = CARTESIAN_POINT ( 'NONE',  ( 829.9999999999992042, 430.0000000000002842, -244.9999999999999716 ) ) ;
#37696 = CARTESIAN_POINT ( 'NONE',  ( 755.2512626584698410, -391.5436935675101608, -315.2512626584710915 ) ) ;
#37697 = FILL_AREA_STYLE_COLOUR ( '', #4009 ) ;
#37698 = CARTESIAN_POINT ( 'NONE',  ( 750.9282345327678740, -304.9181544815161828, 319.8311093483690115 ) ) ;
#37699 = EDGE_CURVE ( 'NONE', #20516, #43844, #19189, .T. ) ;
#37700 = DIRECTION ( 'NONE',  ( 0.000000000000000000, 0.000000000000000000, -1.000000000000000000 ) ) ;
#37701 = CARTESIAN_POINT ( 'NONE',  ( 759.0252816721024374, -288.9982390220559978, 368.0189434323527280 ) ) ;
#37702 = CARTESIAN_POINT ( 'NONE',  ( 815.2698199232961542, -16.81642084023866701, -342.5225473063383106 ) ) ;
#37703 = CARTESIAN_POINT ( 'NONE',  ( 771.2633955100217236, -263.9073299311469327, -363.4237431249939618 ) ) ;
#37704 = LINE ( 'NONE', #1903, #2538 ) ;
#37705 = CARTESIAN_POINT ( 'NONE',  ( 781.7834795799800531, -394.8164208402374697, 315.0636971347436202 ) ) ;
#37706 = CARTESIAN_POINT ( 'NONE',  ( 804.6971507214547046, -123.2817908451530542, 344.0799538623459739 ) ) ;
#37707 = CARTESIAN_POINT ( 'NONE',  ( 757.2208543904082489, -64.71468719896019195, -350.9844846989624330 ) ) ;
#37708 = CARTESIAN_POINT ( 'NONE',  ( 756.1443688327750579, -69.62377810805107003, 314.3581564841659315 ) ) ;
#37709 = CARTESIAN_POINT ( 'NONE',  ( 792.1044303154646968, -372.4527844766012095, 317.8323909638837677 ) ) ;
#37710 = DIRECTION ( 'NONE',  ( -1.000000000000000000, 0.000000000000000000, 0.000000000000000000 ) ) ;
#37711 = FILL_AREA_STYLE ('',( #13241 ) ) ;
#37712 = CARTESIAN_POINT ( 'NONE',  ( 756.1443688327750579, -141.6237781080508569, 314.3581564841659315 ) ) ;
#37713 = CARTESIAN_POINT ( 'NONE',  ( 755.5713283507202505, -413.3618753856920307, 334.6858677611754729 ) ) ;
#37714 = ORIENTED_EDGE ( 'NONE', *, *, #27824, .T. ) ;
#37715 = CARTESIAN_POINT ( 'NONE',  ( 756.5762568750052424, -75.18005720387485269, -348.7366044899774238 ) ) ;
#37716 = CARTESIAN_POINT ( 'NONE',  ( 805.0264073115434940, -366.3510508353228374, -339.4763451958999099 ) ) ;
#37718 = CARTESIAN_POINT ( 'NONE',  ( 755.5713283507202505, -197.3618753856926560, 334.6858677611754729 ) ) ;
#37717 = CARTESIAN_POINT ( 'NONE',  ( 755.5713283507202505, -197.3618753856926560, 334.6858677611754729 ) ) ;
#37719 = CARTESIAN_POINT ( 'NONE',  ( 793.4146539503750546, -361.9874144716864635, -307.6481478633938877 ) ) ;
#37720 = CARTESIAN_POINT ( 'NONE',  ( 51.16348990802859475, 258.0940000000000509, -206.1189999999945144 ) ) ;
#37721 = ORIENTED_EDGE ( 'NONE', *, *, #16294, .T. ) ;
#37722 = CARTESIAN_POINT ( 'NONE',  ( 805.1927285166397041, -400.8164208402373561, 341.8018195045277707 ) ) ;
#37723 = EDGE_CURVE ( 'NONE', #3030, #9195, #43219, .T. ) ;
#37724 = ORIENTED_EDGE ( 'NONE', *, *, #2411, .F. ) ;
#37725 = CARTESIAN_POINT ( 'NONE',  ( 782.4968714119720516, -202.8164208402380950, -305.0891759886411023 ) ) ;
#37726 = CARTESIAN_POINT ( 'NONE',  ( 813.1304606946831655, -113.9073299311474585, 352.3570229623691716 ) ) ;
#37727 = EDGE_CURVE ( 'NONE', #38644, #35738, #23543, .T. ) ;
#37728 = VERTEX_POINT ( 'NONE', #8799 ) ;
#37729 = CARTESIAN_POINT ( 'NONE',  ( 768.0187753319979720, -224.6346026584198228, -318.0580252608186242 ) ) ;
#37730 = ORIENTED_EDGE ( 'NONE', *, *, #10884, .T. ) ;
#37731 = CARTESIAN_POINT ( 'NONE',  ( 756.5762568750052424, -315.1800572038740711, -348.7366044899774238 ) ) ;
#37732 = CARTESIAN_POINT ( 'NONE',  ( 778.1981804954714335, 13.72903370521577138, -314.8072714833589885 ) ) ;
#37733 = CARTESIAN_POINT ( 'NONE',  ( 787.4397851343537695, -237.7255117493289163, 374.2001403089903988 ) ) ;
#37734 = CARTESIAN_POINT ( 'NONE',  ( 779.4709603349208464, -192.3510508353233774, 314.7162404726379918 ) ) ;
#37736 = CYLINDRICAL_SURFACE ( 'NONE', #29243, 7.999999999999896083 ) ;
#37735 = CARTESIAN_POINT ( 'NONE',  ( 784.4999999999993179, -355.4967352946684969, -16.45562775363623587 ) ) ;
#37737 = FACE_OUTER_BOUND ( 'NONE', #15025, .T. ) ;
#37738 = ORIENTED_EDGE ( 'NONE', *, *, #29360, .T. ) ;
#37739 = CARTESIAN_POINT ( 'NONE',  ( 791.9460785601769430, -462.7578698805381237, -362.0383033825738721 ) ) ;
#37740 = CARTESIAN_POINT ( 'NONE',  ( 265.7583438952258916, 290.0000000000001137, -244.9999999999999716 ) ) ;
#37741 = LINE ( 'NONE', #6092, #35895 ) ;
#37742 = ORIENTED_EDGE ( 'NONE', *, *, #28090, .F. ) ;
#37743 = CARTESIAN_POINT ( 'NONE',  ( 797.8822607201568644, -246.5545181178799510, -370.1134526219340160 ) ) ;
#37744 = VECTOR ( 'NONE', #14603, 1000.000000000000227 ) ;
#37745 = CARTESIAN_POINT ( 'NONE',  ( 747.6481478633932056, -109.0999726633349241, 353.4146539503763620 ) ) ;
#37747 = CARTESIAN_POINT ( 'NONE',  ( 758.0580252608178853, -222.4527844766016642, -328.0187753319985404 ) ) ;
#37746 = CARTESIAN_POINT ( 'NONE',  ( 928.0249999999991815, 154.9999999999998863, 350.0000000000000000 ) ) ;
#37748 = CARTESIAN_POINT ( 'NONE',  ( 784.0799538623451781, -371.8055962898682765, -364.6971507214555572 ) ) ;
#37749 = CIRCLE ( 'NONE', #34808, 9.999999999999982236 ) ;
#37750 = CARTESIAN_POINT ( 'NONE',  ( 760.0363995740630116, -250.9181544815163534, -368.7758568127991907 ) ) ;
#37751 = CARTESIAN_POINT ( 'NONE',  ( -28.63011601220122415, -513.1383975375929367, -367.9999999999999432 ) ) ;
#37752 = LINE ( 'NONE', #12581, #6105 ) ;
#37753 = CARTESIAN_POINT ( 'NONE',  ( 790.0220218866281812, -79.09997266333503774, -363.2186876482849129 ) ) ;
#37754 = CARTESIAN_POINT ( 'NONE',  ( 755.1538015810308480, -446.1908817542429802, 343.0433043558613804 ) ) ;
#37755 = CARTESIAN_POINT ( 'NONE',  ( 814.4686193811664907, -363.2817908451523294, 346.2056067578752732 ) ) ;
#37756 = DIRECTION ( 'NONE',  ( -1.000000000000000000, 0.000000000000000000, 0.000000000000000000 ) ) ;
#37757 = CARTESIAN_POINT ( 'NONE',  ( 801.3366627262608972, -440.5328690171407970, -353.0897708529566899 ) ) ;
#37758 = CARTESIAN_POINT ( 'NONE',  ( 810.7187646348534145, -282.4527844766014937, -356.7737145352016341 ) ) ;
#37759 = CARTESIAN_POINT ( 'NONE',  ( -879.9999999999992042, 260.0000000000002274, -219.9999999999999716 ) ) ;
#37760 = CARTESIAN_POINT ( 'NONE',  ( -181.9156952255813735, 290.0000000000001137, -244.9999999999999716 ) ) ;
#37761 = CARTESIAN_POINT ( 'NONE',  ( 768.0187753319979720, -56.63460265842036279, -318.0580252608186242 ) ) ;
#37762 = CARTESIAN_POINT ( 'NONE',  ( 778.7629533639073998, -200.7363362996982801, 375.0009284576466371 ) ) ;
#37763 = CARTESIAN_POINT ( 'NONE',  ( 776.2433038121456548, -156.8965053807780805, -374.8207195650711014 ) ) ;
#37764 = CARTESIAN_POINT ( 'NONE',  ( 745.4481719005789273, -171.7255117493291152, 347.5162901302853129 ) ) ;
#37765 = CARTESIAN_POINT ( 'NONE',  ( 792.2312462859673587, -395.9073299311465348, -307.2067596250082602 ) ) ;
#37766 = DIRECTION ( 'NONE',  ( 1.000000000000000000, 0.000000000000000000, -0.000000000000000000 ) ) ;
#37767 = CARTESIAN_POINT ( 'NONE',  ( 756.3353852180819104, -269.9073299311468190, 331.1735550268788302 ) ) ;
#37768 = CARTESIAN_POINT ( 'NONE',  ( 784.1219089521767955, -69.28179084515321051, 315.0488828828318333 ) ) ;
#37769 = CARTESIAN_POINT ( 'NONE',  ( 778.2165204200184689, -430.8164208402374129, -364.9363028652563230 ) ) ;
#37770 =( BOUNDED_CURVE ( )  B_SPLINE_CURVE ( 3, ( #45458, #41526, #24409, #9878 ),
 .UNSPECIFIED., .F., .T. ) 
 B_SPLINE_CURVE_WITH_KNOTS ( ( 4, 4 ),
 ( 0.000000000000000000, 1.570796326794896558 ),
 .UNSPECIFIED. ) 
 CURVE ( )  GEOMETRIC_REPRESENTATION_ITEM ( )  RATIONAL_B_SPLINE_CURVE ( ( 1.000000000000000000, 0.8047378541243649375, 0.8047378541243649375, 1.000000000000000000 ) ) 
 REPRESENTATION_ITEM ( '' )  );
#37771 = LINE ( 'NONE', #35215, #29186 ) ;
#37772 = DIRECTION ( 'NONE',  ( 0.000000000000000000, -0.6438296778008192334, 0.7651688349527138167 ) ) ;
#37774 = CARTESIAN_POINT ( 'NONE',  ( 794.9819416627830151, -324.9982390220559409, 319.9864689768909898 ) ) ;
#37773 = CARTESIAN_POINT ( 'NONE',  ( 805.0264073115434940, -78.35105083532376113, 339.4763451958999099 ) ) ;
#37775 = ORIENTED_EDGE ( 'NONE', *, *, #13697, .T. ) ;
#37776 = CARTESIAN_POINT ( 'NONE',  ( 793.2243759319678702, -266.5328690171413655, -318.4439275373583200 ) ) ;
#37777 = CARTESIAN_POINT ( 'NONE',  ( 754.8072714833581358, -76.81642084023845030, 338.1981804954720587 ) ) ;
#37778 = VECTOR ( 'NONE', #34270, 1000.000000000000000 ) ;
#37779 = CARTESIAN_POINT ( 'NONE',  ( 803.8556311672234642, -249.6237781080505158, -365.6418435158340117 ) ) ;
#37780 = CARTESIAN_POINT ( 'NONE',  ( 51.16348990802859475, 258.0940000000000509, -199.9999999999945146 ) ) ;
#37781 = CARTESIAN_POINT ( 'NONE',  ( 801.9858362298568863, -387.0783235625955285, 312.7379699480935642 ) ) ;
#37782 = ORIENTED_EDGE ( 'NONE', *, *, #21258, .F. ) ;
#37783 = CARTESIAN_POINT ( 'NONE',  ( 794.9819416627830151, -300.9982390220559409, 319.9864689768909898 ) ) ;
#37784 = CARTESIAN_POINT ( 'NONE',  ( 796.7737145352015204, 3.365397341579444479, 370.7187646348536987 ) ) ;
#37785 = CARTESIAN_POINT ( 'NONE',  ( 804.4286716492782716, -161.3618753856927697, -345.3141322388244703 ) ) ;
#37786 = CARTESIAN_POINT ( 'NONE',  ( 759.7806653035534055, -390.9982390220557136, 324.8639956371180801 ) ) ;
#37787 = CARTESIAN_POINT ( 'NONE',  ( 745.7998596910086917, -125.3618753856928834, -332.5602148656461168 ) ) ;
#37788 = CARTESIAN_POINT ( 'NONE',  ( 800.2193346964446619, -90.99823902205662307, -355.1360043628816925 ) ) ;
#37789 = ORIENTED_EDGE ( 'NONE', *, *, #17924, .T. ) ;
#37790 = CARTESIAN_POINT ( 'NONE',  ( 773.4516893846965786, -43.64542720878966975, -315.8398074228977066 ) ) ;
#37791 = CARTESIAN_POINT ( 'NONE',  ( 763.0428371773158460, -347.4636090269705733, -358.7617431975195359 ) ) ;
#37793 = CARTESIAN_POINT ( 'NONE',  ( 804.6971507214547046, -411.2817908451521589, 344.0799538623459739 ) ) ;
#37792 = CARTESIAN_POINT ( 'NONE',  ( 771.1735550268778070, -105.1800572038747248, 316.3353852180827630 ) ) ;
#37794 = CARTESIAN_POINT ( 'NONE',  ( 801.3366627262608972, -104.5328690171418913, 353.0897708529566899 ) ) ;
#37797 = CARTESIAN_POINT ( 'NONE',  ( 778.7502325331095108, -360.3510508353228374, 304.6391490659818828 ) ) ;
#37796 = DIRECTION ( 'NONE',  ( 0.000000000000000000, 0.000000000000000000, 1.000000000000000000 ) ) ;
#37795 = CARTESIAN_POINT ( 'NONE',  ( 814.2001403089898304, -449.3618753856918602, 347.4397851343538264 ) ) ;
#37798 = CARTESIAN_POINT ( 'NONE',  ( 746.0683387631852383, -115.4419599262327409, 331.3260364891676204 ) ) ;
#37799 = CARTESIAN_POINT ( 'NONE',  ( 802.5472867521000353, -364.3726999360614514, -350.8726784830461156 ) ) ;
#37800 = CARTESIAN_POINT ( 'NONE',  ( 788.7366044899766848, -323.9073299311468190, -316.5762568750059813 ) ) ;
#37801 = AXIS2_PLACEMENT_3D ( 'NONE', #26030, #1341, #8506 ) ;
#37802 = CARTESIAN_POINT ( 'NONE',  ( 749.5768839229115201, -132.5545181178802920, -358.0661480581553064 ) ) ;
#37803 = CARTESIAN_POINT ( 'NONE',  ( 778.7629533639073998, -8.736336299698871599, 375.0009284576466371 ) ) ;
#37805 = LINE ( 'NONE', #6154, #9356 ) ;
#37804 = DIRECTION ( 'NONE',  ( -1.000000000000000000, 0.000000000000000000, 0.000000000000000000 ) ) ;
#37806 = CARTESIAN_POINT ( 'NONE',  ( 796.7845633553578182, -273.6237781080504305, -358.5707757039688204 ) ) ;
#37807 = CARTESIAN_POINT ( 'NONE',  ( 797.8822607201568644, -150.5545181178802352, -370.1134526219340160 ) ) ;
#37808 = CARTESIAN_POINT ( 'NONE',  ( -786.4999999999993179, 26.27639943461401018, 900.0000000000001137 ) ) ;
#37809 = CARTESIAN_POINT ( 'NONE',  ( -115.7583438952258774, -600.0000000000000000, -320.0000000000000568 ) ) ;
#37810 = CARTESIAN_POINT ( 'NONE',  ( 790.0220218866281812, -319.0999726633342561, 363.2186876482849129 ) ) ;
#37811 = VERTEX_POINT ( 'NONE', #15720 ) ;
#37812 = CARTESIAN_POINT ( 'NONE',  ( 791.0478386215596629, -309.8272453906070041, 306.7653713866226326 ) ) ;
#37813 = CARTESIAN_POINT ( 'NONE',  ( 808.0189434323515343, -182.0891481129654323, -319.0252816721025511 ) ) ;
#37814 = DIRECTION ( 'NONE',  ( -0.000000000000000000, -0.000000000000000000, 1.000000000000000000 ) ) ;
#37815 = CARTESIAN_POINT ( 'NONE',  ( 757.7880784355613741, -114.0090635724258163, 312.4576283171834916 ) ) ;
#37816 = CARTESIAN_POINT ( 'NONE',  ( 748.9653473494363425, -290.6346026584195101, -356.9462024416521331 ) ) ;
#37817 = CARTESIAN_POINT ( 'NONE',  ( 999.9999999999992042, -599.0000000000001137, -359.0000000000000000 ) ) ;
#37818 = CARTESIAN_POINT ( 'NONE',  ( 571.1634899080285095, 256.4999999999999432, -193.8809999999981528 ) ) ;
#37819 = CARTESIAN_POINT ( 'NONE',  ( 802.1676090361156639, -134.6346026584201070, 327.8955696845344505 ) ) ;
#37820 = ORIENTED_EDGE ( 'NONE', *, *, #2582, .T. ) ;
#37821 = CARTESIAN_POINT ( 'NONE',  ( 805.6418435158337843, -437.4636090269703459, 363.8556311672236916 ) ) ;
#37822 = CARTESIAN_POINT ( 'NONE',  ( 788.7631598425961101, -361.4419599262319593, -305.7194118038759143 ) ) ;
#37823 = CARTESIAN_POINT ( 'NONE',  ( 787.5162901302840055, -131.3618753856928834, -305.4481719005792684 ) ) ;
#37824 = CARTESIAN_POINT ( 'NONE',  ( 755.8894580844503253, -39.82724539060786384, 332.3691319403863531 ) ) ;
#37825 = CARTESIAN_POINT ( 'NONE',  ( 748.9653473494363425, -386.6346026584191691, -356.9462024416521331 ) ) ;
#37826 = DIRECTION ( 'NONE',  ( 1.000000000000000000, 0.000000000000000000, 0.000000000000000000 ) ) ;
#37827 = CARTESIAN_POINT ( 'NONE',  ( 793.4146539503750546, 22.01258552831228599, 307.6481478633938877 ) ) ;
#37828 = EDGE_LOOP ( 'NONE', ( #22771, #26415, #14119, #33573 ) ) ;
#37829 = AXIS2_PLACEMENT_3D ( 'NONE', #32708, #29014, #36844 ) ;
#37830 = CARTESIAN_POINT ( 'NONE',  ( 773.7943932421234194, -143.8055962898690154, -305.5313806188329409 ) ) ;
#37831 = LINE ( 'NONE', #34362, #42497 ) ;
#37832 = CARTESIAN_POINT ( 'NONE',  ( 746.0683387631852383, -283.4419599262321867, 331.3260364891676204 ) ) ;
#37833 = CARTESIAN_POINT ( 'NONE',  ( 755.5713283507202505, -101.3618753856929544, 334.6858677611754729 ) ) ;
#37834 = AXIS2_PLACEMENT_3D ( 'NONE', #9032, #30502, #36980 ) ;
#37835 = ORIENTED_EDGE ( 'NONE', *, *, #4424, .T. ) ;
#37836 = CARTESIAN_POINT ( 'NONE',  ( 795.9930595647434757, -3.078323562596726681, -320.7433823573372820 ) ) ;
#37837 = CARTESIAN_POINT ( 'NONE',  ( 805.1927285166397041, -280.8164208402378677, 341.8018195045277707 ) ) ;
#37838 = CARTESIAN_POINT ( 'NONE',  ( 747.2067596250078623, -3.180057203875080063, -352.2312462859687230 ) ) ;
#37839 = CARTESIAN_POINT ( 'NONE',  ( 799.9999999999993179, 212.6707680665973612, -236.5295014342203785 ) ) ;
#37840 = ORIENTED_EDGE ( 'NONE', *, *, #26922, .T. ) ;
#37841 = ORIENTED_EDGE ( 'NONE', *, *, #18488, .F. ) ;
#37842 = CARTESIAN_POINT ( 'NONE',  ( 803.6646147819161570, -185.9073299311472454, -348.8264449731210561 ) ) ;
#37843 = CARTESIAN_POINT ( 'NONE',  ( 746.4236121716829757, -399.8272453906067767, -328.8385539511384650 ) ) ;
#37845 = CARTESIAN_POINT ( 'NONE',  ( 752.4576283171824116, -237.0783235625960117, 317.7880784355627952 ) ) ;
#37844 = CARTESIAN_POINT ( 'NONE',  ( 792.3570229623691148, -357.1800572038739574, 373.1304606946836770 ) ) ;
#37846 = CARTESIAN_POINT ( 'NONE',  ( 763.8424801807145741, -258.0090635724253616, -320.5453621957614700 ) ) ;
#37847 = CARTESIAN_POINT ( 'NONE',  ( 762.1405469898971887, -217.5436935675107293, -357.8594530101015607 ) ) ;
#37848 = CARTESIAN_POINT ( 'NONE',  ( 771.2633955100217236, -407.9073299311465348, -363.4237431249939618 ) ) ;
#37849 = CARTESIAN_POINT ( 'NONE',  ( 794.9819416627830151, -228.9982390220561683, 319.9864689768909898 ) ) ;
#37850 = EDGE_LOOP ( 'NONE', ( #15000, #18543 ) ) ;
#37851 = CARTESIAN_POINT ( 'NONE',  ( 782.5225473063381969, -358.2709662947829088, 375.2698199232970637 ) ) ;
#37852 = CARTESIAN_POINT ( 'NONE',  ( -208.8365100919714052, 260.0000000000001137, -202.7499999999925251 ) ) ;
#37853 = CARTESIAN_POINT ( 'NONE',  ( 797.8822607201568644, -6.554518117880697048, -370.1134526219340160 ) ) ;
#37854 = PLANE ( 'NONE',  #25578 ) ;
#37855 = LINE ( 'NONE', #26761, #39363 ) ;
#37856 = CARTESIAN_POINT ( 'NONE',  ( 804.8461984189677878, -242.1908817542435770, 336.9566956441385628 ) ) ;
#37857 = CARTESIAN_POINT ( 'NONE',  ( 771.1735550268778070, -81.18005720387481006, 316.3353852180827630 ) ) ;
#37858 = EDGE_CURVE ( 'NONE', #36186, #6776, #23508, .T. ) ;
#37859 = ORIENTED_EDGE ( 'NONE', *, *, #11150, .T. ) ;
#37860 = CARTESIAN_POINT ( 'NONE',  ( 745.1792804349281596, -446.1908817542429802, -343.7566961878542884 ) ) ;
#37861 = CIRCLE ( 'NONE', #23821, 7.999999999999896083 ) ;
#37862 = CARTESIAN_POINT ( 'NONE',  ( 763.2262854647970016, -80.63460265842029173, -309.2812353651462445 ) ) ;
#37863 = PRODUCT_DEFINITION_FORMATION_WITH_SPECIFIED_SOURCE ( 'ANY', '', #38425, .NOT_KNOWN. ) ;
#37864 = CARTESIAN_POINT ( 'NONE',  ( 783.0433043558608688, -240.8965053807777963, 315.1538015810313027 ) ) ;
#37865 = CARTESIAN_POINT ( 'NONE',  ( 759.9864689768902508, -434.0891481129646081, -354.9819416627836404 ) ) ;
#37866 = CARTESIAN_POINT ( 'NONE',  ( 755.5713283507202505, -29.36187538569318178, -334.6858677611754729 ) ) ;
#37867 = CARTESIAN_POINT ( 'NONE',  ( 760.0363995740630116, -10.91815448151704793, 368.7758568127991907 ) ) ;
#37868 = CARTESIAN_POINT ( 'NONE',  ( 805.1927285166397041, 7.183579159761247723, -341.8018195045277707 ) ) ;
#37869 = CARTESIAN_POINT ( 'NONE',  ( 814.2001403089898304, -185.3618753856926844, -347.4397851343538264 ) ) ;
#37870 = CARTESIAN_POINT ( 'NONE',  ( 755.2512626584698410, -79.54369356751119824, 315.2512626584710915 ) ) ;
#37871 = CARTESIAN_POINT ( 'NONE',  ( 751.6929314249748586, -126.9982390220565094, 318.8095938919659034 ) ) ;
#37872 = CARTESIAN_POINT ( 'NONE',  ( 939.9999999999993179, -418.3138125091625170, -201.9999999999998863 ) ) ;
#37873 = LINE ( 'NONE', #27704, #39468 ) ;
#37874 = CARTESIAN_POINT ( 'NONE',  ( 783.7566961878529810, -288.8965053807775121, -305.1792804349288417 ) ) ;
#37875 = CARTESIAN_POINT ( 'NONE',  ( 783.7953271457878373, -416.1908817542430938, 375.1787889125761239 ) ) ;
#37876 = CARTESIAN_POINT ( 'NONE',  ( 763.0537975583475827, -288.4527844766014937, -371.0346526505627480 ) ) ;
#37877 = CARTESIAN_POINT ( 'NONE',  ( 181.1634899080285948, 260.0000000000000000, -199.9999999999953957 ) ) ;
#37878 = CARTESIAN_POINT ( 'NONE',  ( 796.7737145352015204, -404.6346026584193396, 370.7187646348536987 ) ) ;
#37879 = CARTESIAN_POINT ( 'NONE',  ( 792.3570229623691148, -21.18005720387502322, 373.1304606946836770 ) ) ;
#37880 = CARTESIAN_POINT ( 'NONE',  ( 757.8323909638827445, -338.6346026584195101, -352.1044303154654358 ) ) ;
#37881 = CARTESIAN_POINT ( 'NONE',  ( 793.2243759319678702, -26.53286901714210799, 318.4439275373583200 ) ) ;
#37882 = CARTESIAN_POINT ( 'NONE',  ( 771.2368401574024119, -37.44195992623299674, -374.2805881961240857 ) ) ;
#37883 = CARTESIAN_POINT ( 'NONE',  ( 766.7756240680305382, -158.5328690171417065, -361.5560724626415663 ) ) ;
#37884 = CARTESIAN_POINT ( 'NONE',  ( 766.5853460496234675, -181.9874144716870887, 372.3518521366060554 ) ) ;
#37885 = DIRECTION ( 'NONE',  ( 0.000000000000000000, 0.000000000000000000, 1.000000000000000000 ) ) ;
#37886 = CARTESIAN_POINT ( 'NONE',  ( 776.2433038121456548, -180.8965053807779952, 374.8207195650711014 ) ) ;
#37887 = ORIENTED_EDGE ( 'NONE', *, *, #32039, .T. ) ;
#37888 = CARTESIAN_POINT ( 'NONE',  ( 757.8323909638827445, -74.63460265842032015, -352.1044303154654358 ) ) ;
#37889 = CARTESIAN_POINT ( 'NONE',  ( 759.2295555964440155, -160.1692326535053326, -353.9708237608231229 ) ) ;
#37890 = CARTESIAN_POINT ( 'NONE',  ( 788.8264449731200330, -165.1800572038745258, 363.6646147819171233 ) ) ;
#37891 = EDGE_CURVE ( 'NONE', #10815, #25509, #41128, .T. ) ;
#37892 = CARTESIAN_POINT ( 'NONE',  ( 813.2346286133761168, 18.73985825558501972, -328.9521613784389160 ) ) ;
#37894 = CARTESIAN_POINT ( 'NONE',  ( 778.2165204200184689, -310.8164208402377540, 364.9363028652563230 ) ) ;
#37893 = CARTESIAN_POINT ( 'NONE',  ( 755.3201227861273992, -291.7255117493285752, 345.3687786644892981 ) ) ;
#37895 = VECTOR ( 'NONE', #8690, 1000.000000000000114 ) ;
#37896 = DIRECTION ( 'NONE',  ( -0.000000000000000000, 0.000000000000000000, 1.000000000000000000 ) ) ;
#37897 = EDGE_LOOP ( 'NONE', ( #1779, #27802, #33335, #35979, #26423, #41601, #19902, #37511 ) ) ;
#37898 = CARTESIAN_POINT ( 'NONE',  ( 804.9511171171677688, -5.805596289869448867, 335.8780910478229202 ) ) ;
#37899 = CARTESIAN_POINT ( 'NONE',  ( 760.0363995740630116, -322.9181544815161260, -368.7758568127991907 ) ) ;
#37900 = CARTESIAN_POINT ( 'NONE',  ( 755.2512626584698410, -223.5436935675107577, 315.2512626584710915 ) ) ;
#37901 = CARTESIAN_POINT ( 'NONE',  ( 804.8461984189677878, -338.1908817542433212, 336.9566956441385628 ) ) ;
#37902 = CARTESIAN_POINT ( 'NONE',  ( 796.7845633553578182, -417.6237781080499190, 358.5707757039688204 ) ) ;
#37903 = CARTESIAN_POINT ( 'NONE',  ( 798.5707757039680246, -125.4636090269712412, -356.7845633553585003 ) ) ;
#37904 = CARTESIAN_POINT ( 'NONE',  ( 792.1044303154645831, -108.4527844766019911, -317.8323909638837677 ) ) ;
#37905 = CARTESIAN_POINT ( 'NONE',  ( 774.6312213355098493, -311.3618753856923149, -364.6798772138717482 ) ) ;
#37906 = ORIENTED_EDGE ( 'NONE', *, *, #43568, .F. ) ;
#37907 = CARTESIAN_POINT ( 'NONE',  ( 768.0187753319979720, -440.6346026584191122, -318.0580252608186242 ) ) ;
#37908 = VECTOR ( 'NONE', #20186, 1000.000000000000114 ) ;
#37909 = CARTESIAN_POINT ( 'NONE',  ( 779.4709603349208464, -312.3510508353230080, 314.7162404726379918 ) ) ;
#37910 = DIRECTION ( 'NONE',  ( -1.000000000000000000, -4.625929269271485914E-16, -0.000000000000000000 ) ) ;
#37911 = CARTESIAN_POINT ( 'NONE',  ( 799.9999999999993179, -462.9681489794448339, 370.0000000000000568 ) ) ;
#37912 = CARTESIAN_POINT ( 'NONE',  ( 796.1575198192839480, -126.0090635724257737, 359.4546378042384163 ) ) ;
#37913 = CARTESIAN_POINT ( 'NONE',  ( 879.9999999999992042, 430.0000000000002842, -320.0000000000000568 ) ) ;
#37914 = ORIENTED_EDGE ( 'NONE', *, *, #28125, .F. ) ;
#37915 = CARTESIAN_POINT ( 'NONE',  ( 812.3518521366052028, -337.0999726633342561, -326.5853460496235243 ) ) ;
#37916 = CARTESIAN_POINT ( 'NONE',  ( 762.1177392798416577, -234.5545181178799794, 309.8865473780659272 ) ) ;
#37917 = CARTESIAN_POINT ( 'NONE',  ( 801.9419747391806368, -330.4527844766013231, -351.9812246680014027 ) ) ;
#37918 = DIRECTION ( 'NONE',  ( -1.000000000000000000, -0.000000000000000000, -0.000000000000000000 ) ) ;
#37919 = CARTESIAN_POINT ( 'NONE',  ( 800.9840315886518738, -196.9181544815164386, -354.1144889064786412 ) ) ;
#37920 = CARTESIAN_POINT ( 'NONE',  ( 815.2698199232961542, -40.81642084023859951, 342.5225473063383106 ) ) ;
#37921 = CARTESIAN_POINT ( 'NONE',  ( 805.7454966640377734, -452.9681489794450044, 346.1170114844039745 ) ) ;
#37922 = CARTESIAN_POINT ( 'NONE',  ( 763.0537975583476964, -384.4527844766011526, -371.0346526505628617 ) ) ;
#37923 = VECTOR ( 'NONE', #25032, 1000.000000000000000 ) ;
#37924 = CARTESIAN_POINT ( 'NONE',  ( 879.9999999999992042, 240.0000000000000853, -360.0000000000000000 ) ) ;
#37925 = CARTESIAN_POINT ( 'NONE',  ( 776.2046728542105711, -332.1908817542433781, 304.8212110874238761 ) ) ;
#37926 = LINE ( 'NONE', #11918, #41205 ) ;
#37927 = CARTESIAN_POINT ( 'NONE',  ( 801.1904061080336987, -308.0891481129650629, 368.3070685750235498 ) ) ;
#37928 = CARTESIAN_POINT ( 'NONE',  ( 767.6429770376289525, -9.180057203875058747, -306.8695393053162093 ) ) ;
#37929 = CARTESIAN_POINT ( 'NONE',  ( 792.1044303154645831, -252.4527844766015789, -317.8323909638837677 ) ) ;
#37930 = EDGE_CURVE ( 'NONE', #27336, #26364, #22867, .T. ) ;
#37931 = FACE_OUTER_BOUND ( 'NONE', #33088, .T. ) ;
#37932 = CARTESIAN_POINT ( 'NONE',  ( 774.6312213355099630, -407.3618753856920307, 364.6798772138717482 ) ) ;
#37933 = CARTESIAN_POINT ( 'NONE',  ( 760.7433823573367135, -156.0090635724256742, 355.9930595647440441 ) ) ;
#37934 = CARTESIAN_POINT ( 'NONE',  ( 761.2382568024794409, -39.62377810805116951, -356.9571628226838129 ) ) ;
#37935 = CARTESIAN_POINT ( 'NONE',  ( 805.9055244015594326, -51.62377810805111267, 315.8990559732753240 ) ) ;
#37936 = CARTESIAN_POINT ( 'NONE',  ( 765.0180583372156207, -360.9982390220557704, 360.0135310231089534 ) ) ;
#37937 = CARTESIAN_POINT ( 'NONE',  ( -37.63011601220122770, -513.1383975375929367, -350.0000000000000000 ) ) ;
#37938 = VECTOR ( 'NONE', #25835, 1000.000000000000000 ) ;
#37939 =( LENGTH_UNIT ( ) NAMED_UNIT ( * ) SI_UNIT ( .MILLI., .METRE. ) );
#37940 = CARTESIAN_POINT ( 'NONE',  ( 744.9990715423526808, -138.3510508353236048, 341.2370466360926002 ) ) ;
#37941 = CARTESIAN_POINT ( 'NONE',  ( 768.0187753319979720, -440.6346026584191122, 318.0580252608186242 ) ) ;
#37942 = ORIENTED_EDGE ( 'NONE', *, *, #31178, .T. ) ;
#37943 = CARTESIAN_POINT ( 'NONE',  ( 804.4286716492782716, -65.36187538569306810, -345.3141322388244703 ) ) ;
#37944 = EDGE_CURVE ( 'NONE', #10891, #45297, #1404, .T. ) ;
#37945 = EDGE_CURVE ( 'NONE', #19734, #43685, #30727, .T. ) ;
#37946 = AXIS2_PLACEMENT_3D ( 'NONE', #36857, #40096, #44238 ) ;
#37947 = CARTESIAN_POINT ( 'NONE',  ( 761.2382568024794409, -351.6237781080502032, -356.9571628226838129 ) ) ;
#37949 = CARTESIAN_POINT ( 'NONE',  ( 762.3223304703356007, -199.5436935675108430, 322.3223304703362828 ) ) ;
#37948 = CARTESIAN_POINT ( 'NONE',  ( 802.1676090361156639, -206.6346026584198512, 327.8955696845344505 ) ) ;
#37950 = CARTESIAN_POINT ( 'NONE',  ( 815.0009284576459549, -366.3510508353228374, -338.7629533639073429 ) ) ;
#37951 = CARTESIAN_POINT ( 'NONE',  ( 879.9999999999990905, 479.9999999999998863, 210.0000000000000000 ) ) ;
#37952 = VERTEX_POINT ( 'NONE', #40658 ) ;
#37953 = CARTESIAN_POINT ( 'NONE',  ( 774.6312213355099630, -383.3618753856921444, 364.6798772138717482 ) ) ;
#37954 = ORIENTED_EDGE ( 'NONE', *, *, #42697, .F. ) ;
#37955 = CARTESIAN_POINT ( 'NONE',  ( 800.9747183278959710, -228.9982390220561683, -311.9810565676471583 ) ) ;
#37956 = CARTESIAN_POINT ( 'NONE',  ( 755.2512626584698410, -127.5436935675110561, 315.2512626584710915 ) ) ;
#37957 = VERTEX_POINT ( 'NONE', #30035 ) ;
#37958 = CARTESIAN_POINT ( 'NONE',  ( 781.7834795799800531, -226.8164208402380098, -315.0636971347436202 ) ) ;
#37959 = VECTOR ( 'NONE', #4210, 1000.000000000000000 ) ;
#37960 = ORIENTED_EDGE ( 'NONE', *, *, #9748, .F. ) ;
#37961 = EDGE_CURVE ( 'NONE', #34249, #10339, #5782, .T. ) ;
#37962 = CARTESIAN_POINT ( 'NONE',  ( 757.8323909638827445, -338.6346026584195101, -352.1044303154654358 ) ) ;
#37963 = CARTESIAN_POINT ( 'NONE',  ( 805.1927285166397041, 7.183579159761247723, -341.8018195045277707 ) ) ;
#37964 = VECTOR ( 'NONE', #10960, 1000.000000000000000 ) ;
#37965 = EDGE_CURVE ( 'NONE', #40984, #23028, #39812, .T. ) ;
#37966 = CARTESIAN_POINT ( 'NONE',  ( 794.1144889064781864, -202.1692326535051905, 360.9840315886528401 ) ) ;
#37968 = CARTESIAN_POINT ( 'NONE',  ( 772.4999999999993179, -462.9681489794448339, -369.0473750965555837 ) ) ;
#37967 = CARTESIAN_POINT ( 'NONE',  ( 794.9285562942586694, -457.5945560043289788, 366.0218793896430043 ) ) ;
#37969 = CARTESIAN_POINT ( 'NONE',  ( -28.63011601220122415, -544.8427095258973623, -369.9999999999999432 ) ) ;
#37970 = EDGE_LOOP ( 'NONE', ( #26818, #23143 ) ) ;
#37971 = CARTESIAN_POINT ( 'NONE',  ( 764.8639956371174549, 15.91085188703394238, -319.7806653035542013 ) ) ;
#37972 = CARTESIAN_POINT ( 'NONE',  ( 786.4999999999993179, -110.5936016518798652, 750.6326042729449455 ) ) ;
#37973 = PLANE ( 'NONE',  #26292 ) ;
#37974 = EDGE_CURVE ( 'NONE', #39962, #9635, #25743, .T. ) ;
#37975 = VERTEX_POINT ( 'NONE', #40445 ) ;
#37976 = CARTESIAN_POINT ( 'NONE',  ( 768.9521613784389729, -225.8272453906072599, -373.2346286133773106 ) ) ;
#37977 = CARTESIAN_POINT ( 'NONE',  ( 793.5525998758768083, -103.0999726633349525, 372.6845335610516941 ) ) ;
#37978 = VECTOR ( 'NONE', #43117, 1000.000000000000000 ) ;
#37980 = CARTESIAN_POINT ( 'NONE',  ( 804.9363028652555840, -232.2709662947834488, -338.2165204200192079 ) ) ;
#37979 = CARTESIAN_POINT ( 'NONE',  ( 787.4999999999992042, -512.9681489794448908, 350.0000000000000000 ) ) ;
#37981 = CARTESIAN_POINT ( 'NONE',  ( 803.2186876482843445, -391.9874144716864066, -350.0220218866286928 ) ) ;
#37982 = CARTESIAN_POINT ( 'NONE',  ( 744.6391490659812007, -254.7363362996981095, -338.7502325331110455 ) ) ;
#37983 = PLANE ( 'NONE',  #26744 ) ;
#37984 = DIRECTION ( 'NONE',  ( -1.337618101958019798E-16, 1.000000000000000000, 1.672022627447524747E-16 ) ) ;
#37985 = CARTESIAN_POINT ( 'NONE',  ( 755.8894580844503253, -87.82724539060770041, -332.3691319403863531 ) ) ;
#37986 = CARTESIAN_POINT ( 'NONE',  ( 793.0897708529556667, -438.5545181178793541, 361.3366627262616362 ) ) ;
#37987 = CIRCLE ( 'NONE', #7027, 10.00000000000000888 ) ;
#37988 = AXIS2_PLACEMENT_3D ( 'NONE', #15594, #12132, #43537 ) ;
#37989 = CARTESIAN_POINT ( 'NONE',  ( 797.8822607201568644, -366.5545181178795815, 370.1134526219340160 ) ) ;
#37990 = CARTESIAN_POINT ( 'NONE',  ( 799.9999999999993179, -512.9681489794448908, 339.9999999999999432 ) ) ;
#37991 = CARTESIAN_POINT ( 'NONE',  ( 759.2295555964440155, -424.1692326535044799, -353.9708237608231229 ) ) ;
#37992 = CARTESIAN_POINT ( 'NONE',  ( 759.0252816721024374, -288.9982390220559978, -368.0189434323527280 ) ) ;
#37993 = DIRECTION ( 'NONE',  ( 0.000000000000000000, 0.000000000000000000, 1.000000000000000000 ) ) ;
#37994 = CARTESIAN_POINT ( 'NONE',  ( 785.3687786644884454, 12.63812461430668321, 315.3201227861279676 ) ) ;
#37995 = CARTESIAN_POINT ( 'NONE',  ( 754.8072714833581358, -76.81642084023845030, -338.1981804954720587 ) ) ;
#37996 = ADVANCED_FACE ( 'NONE', ( #9480 ), #34410, .T. ) ;
#37997 = CARTESIAN_POINT ( 'NONE',  ( 747.6481478633932056, -205.0999726633346256, 353.4146539503763620 ) ) ;
#37998 = CARTESIAN_POINT ( 'NONE',  ( 811.6461892240364477, -172.7146871989598083, -324.1737431748509835 ) ) ;
#37999 = CARTESIAN_POINT ( 'NONE',  ( 772.5602148656447525, -201.7255117493290015, 305.7998596910095443 ) ) ;
#38000 = CARTESIAN_POINT ( 'NONE',  ( 805.0032342141412300, -421.5436935675101040, -314.9967657858571783 ) ) ;
#38001 = FACE_BOUND ( 'NONE', #34724, .T. ) ;
#38002 = EDGE_CURVE ( 'NONE', #1656, #27157, #5312, .T. ) ;
#38003 = VECTOR ( 'NONE', #6521, 1000.000000000000000 ) ;
#38004 = CARTESIAN_POINT ( 'NONE',  ( 788.7366044899766848, -299.9073299311468759, 316.5762568750059813 ) ) ;
#38005 = CARTESIAN_POINT ( 'NONE',  ( 802.5472867521000353, -52.37269993606237506, 350.8726784830461156 ) ) ;
#38006 = CARTESIAN_POINT ( 'NONE',  ( 755.3201227861273992, -411.7255117493282910, -345.3687786644892981 ) ) ;
#38007 = CIRCLE ( 'NONE', #18098, 2.749999999999808153 ) ;
#38008 = DIRECTION ( 'NONE',  ( -1.000000000000000000, -0.000000000000000000, 0.000000000000000000 ) ) ;
#38009 = CARTESIAN_POINT ( 'NONE',  ( 759.9999999999992042, -512.9681489794448908, 339.9999999999999432 ) ) ;
#38011 = CARTESIAN_POINT ( 'NONE',  ( 792.1044303154645831, -324.4527844766013231, 317.8323909638837677 ) ) ;
#38010 = CARTESIAN_POINT ( 'NONE',  ( 769.1273215169530886, -118.7146871989600072, 317.4527132478988847 ) ) ;
#38012 = ORIENTED_EDGE ( 'NONE', *, *, #28976, .T. ) ;
#38013 = EDGE_CURVE ( 'NONE', #3415, #6890, #36959, .T. ) ;
#38014 = CARTESIAN_POINT ( 'NONE',  ( 754.8983024940795303, -258.8965053807777963, -336.9254006560228163 ) ) ;
#38015 = CARTESIAN_POINT ( 'NONE',  ( 778.1981804954714335, -106.2709662947838467, 314.8072714833589885 ) ) ;
#38016 = CARTESIAN_POINT ( 'NONE',  ( 751.2241431872005251, -256.1692326535049915, -359.9636004259367610 ) ) ;
#38017 = DIRECTION ( 'NONE',  ( 1.000000000000000000, 0.000000000000000000, 0.000000000000000000 ) ) ;
#38018 = CARTESIAN_POINT ( 'NONE',  ( 771.2368401574024119, -373.4419599262319593, 374.2805881961240857 ) ) ;
#38019 = ORIENTED_EDGE ( 'NONE', *, *, #16727, .T. ) ;
#38020 = CARTESIAN_POINT ( 'NONE',  ( 785.3687786644884454, -299.3618753856922581, 315.3201227861279676 ) ) ;
#38021 = CIRCLE ( 'NONE', #43896, 8.024999999999948841 ) ;
#38022 = CARTESIAN_POINT ( 'NONE',  ( 770.0799878456142551, -61.98741447168745822, -362.9823548866085616 ) ) ;
#38023 = CARTESIAN_POINT ( 'NONE',  ( 801.9419747391806368, -162.4527844766018632, -351.9812246680014027 ) ) ;
#38024 = CARTESIAN_POINT ( 'NONE',  ( 759.7806653035534055, -366.9982390220556567, 324.8639956371180801 ) ) ;
#38025 = VECTOR ( 'NONE', #12761, 1000.000000000000000 ) ;
#38026 = CARTESIAN_POINT ( 'NONE',  ( 787.5162901302840055, -107.3618753856928976, -305.4481719005792684 ) ) ;
#38027 = CARTESIAN_POINT ( 'NONE',  ( 804.6798772138710092, -111.7255117493292857, -334.6312213355106451 ) ) ;
#38028 = EDGE_LOOP ( 'NONE', ( #20400, #24639, #8315, #5764 ) ) ;
#38029 = CARTESIAN_POINT ( 'NONE',  ( 796.1575198192839480, -54.00906357242601530, -359.4546378042384163 ) ) ;
#38030 = CARTESIAN_POINT ( 'NONE',  ( 804.1105419155481968, -339.8272453906069472, -347.6308680596136469 ) ) ;
#38032 = CARTESIAN_POINT ( 'NONE',  ( 804.1105419155481968, -411.8272453906067199, 347.6308680596136469 ) ) ;
#38031 = CARTESIAN_POINT ( 'NONE',  ( 804.4286716492782716, -113.3618753856929260, 345.3141322388244703 ) ) ;
#38035 = CARTESIAN_POINT ( 'NONE',  ( 744.9990715423526808, -354.3510508353228943, 341.2370466360926002 ) ) ;
#38034 = CARTESIAN_POINT ( 'NONE',  ( -789.9999999999992042, 205.0000000000000568, -329.9999999999999432 ) ) ;
#38033 = LINE ( 'NONE', #27178, #18151 ) ;
#38036 = CARTESIAN_POINT ( 'NONE',  ( 745.1769319972822814, -113.8055962898691149, 346.2694204179732083 ) ) ;
#38037 = CARTESIAN_POINT ( 'NONE',  ( 755.3028492785439312, -375.2817908451523294, -335.9200461376539693 ) ) ;
#38038 = CARTESIAN_POINT ( 'NONE',  ( 755.3201227861273992, -363.7255117493284047, -345.3687786644892981 ) ) ;
#38039 = CARTESIAN_POINT ( 'NONE',  ( 802.2119215644370342, -126.0090635724257737, -367.5423716828165084 ) ) ;
#38040 = AXIS2_PLACEMENT_3D ( 'NONE', #41215, #34036, #30574 ) ;
#38041 = CARTESIAN_POINT ( 'NONE',  ( 747.6481478633932056, -13.09997266333522248, 353.4146539503763620 ) ) ;
#38043 = FACE_OUTER_BOUND ( 'NONE', #22784, .T. ) ;
#38042 = DIRECTION ( 'NONE',  ( 0.000000000000000000, 0.000000000000000000, 1.000000000000000000 ) ) ;
#38044 = CARTESIAN_POINT ( 'NONE',  ( 754.3581564841646241, -161.4636090269711133, -316.1443688327762516 ) ) ;
#38045 = FACE_OUTER_BOUND ( 'NONE', #31129, .T. ) ;
#38046 = LINE ( 'NONE', #44976, #39291 ) ;
#38047 = CARTESIAN_POINT ( 'NONE',  ( 775.8780910478218402, -345.2817908451523863, 364.9511171171680530 ) ) ;
#38048 = VERTEX_POINT ( 'NONE', #33731 ) ;
#38049 = CARTESIAN_POINT ( 'NONE',  ( 811.3240766477731540, -292.3726999360616219, 355.6651683502462902 ) ) ;
#38050 = CARTESIAN_POINT ( 'NONE',  ( 772.5602148656447525, -177.7255117493290868, -305.7998596910095443 ) ) ;
#38051 = DIRECTION ( 'NONE',  ( -1.000000000000000000, 1.892425610156518354E-16, 0.000000000000000000 ) ) ;
#38052 = CARTESIAN_POINT ( 'NONE',  ( 810.4231160770870019, -120.5545181178803205, 321.9338519418446936 ) ) ;
#38053 = CARTESIAN_POINT ( 'NONE',  ( 777.5031285880264704, -310.8164208402377540, -374.9108240113588408 ) ) ;
#38054 = AXIS2_PLACEMENT_3D ( 'NONE', #12568, #25965, #1935 ) ;
#38055 = CARTESIAN_POINT ( 'NONE',  ( 786.4999999999993179, -110.5936016518799221, 750.6326042729449455 ) ) ;
#38056 = PRODUCT_DEFINITION_SHAPE ( 'NONE', 'NONE',  #45737 ) ;
#38057 = DIRECTION ( 'NONE',  ( 0.000000000000000000, 0.000000000000000000, -1.000000000000000000 ) ) ;
#38058 = CARTESIAN_POINT ( 'NONE',  ( 759.9864689768902508, -194.0891481129654039, 354.9819416627836404 ) ) ;
#38059 = VERTEX_POINT ( 'NONE', #12943 ) ;
#38060 = CARTESIAN_POINT ( 'NONE',  ( 757.7880784355613741, -426.0090635724247932, 312.4576283171834916 ) ) ;
#38061 = CARTESIAN_POINT ( 'NONE',  ( 811.6461892240364477, -388.7146871989592114, -324.1737431748509835 ) ) ;
#38062 = CARTESIAN_POINT ( 'NONE',  ( 804.7487373415286811, -115.5436935675110988, -364.7487373415288516 ) ) ;
#38063 = CARTESIAN_POINT ( 'NONE',  ( 776.9254006560222479, -44.19088175424421649, 314.8983024940802125 ) ) ;
#38064 = CARTESIAN_POINT ( 'NONE',  ( 772.4837098697144029, -383.3618753856921444, -374.5518280994205611 ) ) ;
#38065 = PLANE ( 'NONE',  #25444 ) ;
#38066 = CARTESIAN_POINT ( 'NONE',  ( 805.0264073115434940, -438.3510508353226669, 339.4763451958999099 ) ) ;
#38067 = ORIENTED_EDGE ( 'NONE', *, *, #40134, .T. ) ;
#38068 = EDGE_CURVE ( 'NONE', #24322, #42149, #12482, .T. ) ;
#38069 = CARTESIAN_POINT ( 'NONE',  ( 814.8230680027162407, -149.8055962898689870, -333.7305795820267917 ) ) ;
#38070 = CARTESIAN_POINT ( 'NONE',  ( 768.8385539511368734, -263.2601417444141134, 306.4236121716840557 ) ) ;
#38071 = CARTESIAN_POINT ( 'NONE',  ( 791.9812246680005501, -116.6346026584201780, 361.9419747391813189 ) ) ;
#38072 = EDGE_LOOP ( 'NONE', ( #15685, #26802, #1488, #31208 ) ) ;
#38073 = AXIS2_PLACEMENT_3D ( 'NONE', #6088, #34948, #41434 ) ;
#38074 = CARTESIAN_POINT ( 'NONE',  ( 803.2186876482843445, -7.987414471687621642, -350.0220218866286928 ) ) ;
#38075 = CARTESIAN_POINT ( 'NONE',  ( 800.2193346964447755, -282.9982390220558841, 355.1360043628815788 ) ) ;
#38076 = CARTESIAN_POINT ( 'NONE',  ( 796.7737145352015204, 3.365397341579444479, -370.7187646348536987 ) ) ;
#38077 = CARTESIAN_POINT ( 'NONE',  ( 441.1634899080286232, 258.0939999999999372, -206.1189999999972144 ) ) ;
#38078 = EDGE_LOOP ( 'NONE', ( #29443, #45057, #33389, #36148 ) ) ;
#38080 = ORIENTED_EDGE ( 'NONE', *, *, #16833, .F. ) ;
#38079 = CARTESIAN_POINT ( 'NONE',  ( 775.9200461376533440, -95.80559628986917176, -315.3028492785443291 ) ) ;
#38081 = CARTESIAN_POINT ( 'NONE',  ( 781.7834795799800531, -178.8164208402381519, -315.0636971347436202 ) ) ;
#38082 = CARTESIAN_POINT ( 'NONE',  ( 757.7880784355613741, -402.0090635724250205, -312.4576283171834916 ) ) ;
#38083 = VECTOR ( 'NONE', #26518, 1000.000000000000000 ) ;
#38084 = CARTESIAN_POINT ( 'NONE',  ( 778.1981804954714335, -250.2709662947832783, -314.8072714833589885 ) ) ;
#38085 = AXIS2_PLACEMENT_3D ( 'NONE', #2388, #9336, #24952 ) ;
#38087 = CARTESIAN_POINT ( 'NONE',  ( 761.9338519418445230, -254.5328690171413655, 370.4231160770881957 ) ) ;
#38086 = CARTESIAN_POINT ( 'NONE',  ( 815.2698199232962679, -352.8164208402375266, 342.5225473063383674 ) ) ;
#38088 = CARTESIAN_POINT ( 'NONE',  ( 758.4439275373578084, -252.5545181178799226, -353.2243759319684386 ) ) ;
#38089 = CARTESIAN_POINT ( 'NONE',  ( 800.2193346964447755, -258.9982390220561115, -355.1360043628815788 ) ) ;
#38090 = CARTESIAN_POINT ( 'NONE',  ( 804.9363028652555840, -424.2709662947829088, -338.2165204200192079 ) ) ;
#38091 = CARTESIAN_POINT ( 'NONE',  ( 785.3141322388236176, -69.72551174932942786, -364.4286716492789537 ) ) ;
#38092 = CARTESIAN_POINT ( 'NONE',  ( 797.6776695296629214, -235.5436935675107293, 357.6776695296636603 ) ) ;
#38093 = ORIENTED_EDGE ( 'NONE', *, *, #5775, .F. ) ;
#38094 = CARTESIAN_POINT ( 'NONE',  ( 746.8695393053150156, -341.9073299311465917, 327.6429770376306010 ) ) ;
#38095 = CARTESIAN_POINT ( 'NONE',  ( -879.9999999999992042, 260.0000000000002274, -219.9999999999999716 ) ) ;
#38096 = CARTESIAN_POINT ( 'NONE',  ( 814.8207195650702488, -50.19088175424420939, -336.2433038121456548 ) ) ;
#38097 = CARTESIAN_POINT ( 'NONE',  ( 770.7832876896738981, 16.45630643248850333, 316.4833103687052471 ) ) ;
#38098 = CARTESIAN_POINT ( 'NONE',  ( 799.9999999999993179, -512.9681489794448908, 309.9999999999998863 ) ) ;
#38099 = CARTESIAN_POINT ( 'NONE',  ( 802.5472867521000353, -244.3726999360617924, 350.8726784830461156 ) ) ;
#38100 = CARTESIAN_POINT ( 'NONE',  ( 781.7834795799800531, -130.8164208402383224, 315.0636971347436202 ) ) ;
#38101 = CARTESIAN_POINT ( 'NONE',  ( 769.9779781133707957, -19.09997266333520116, -316.7813123517150871 ) ) ;
#38102 = CARTESIAN_POINT ( 'NONE',  ( 814.5518280994195948, -63.72551174932941365, -332.4837098697145166 ) ) ;
#38103 = CARTESIAN_POINT ( 'NONE',  ( 754.9735926884551418, -282.3510508353230080, 340.5236548041000333 ) ) ;
#38104 = AXIS2_PLACEMENT_3D ( 'NONE', #28239, #7945, #7255 ) ;
#38105 = CARTESIAN_POINT ( 'NONE',  ( 788.7366044899766848, -443.9073299311464780, -316.5762568750059813 ) ) ;
#38106 = CARTESIAN_POINT ( 'NONE',  ( 762.1405469898973024, -49.54369356751129772, -357.8594530101016176 ) ) ;
#38107 = CARTESIAN_POINT ( 'NONE',  ( 799.9636004259356241, 1.081845518482914104, 311.2241431872006956 ) ) ;
#38109 = CIRCLE ( 'NONE', #18207, 6.118999999999985562 ) ;
#38108 = CARTESIAN_POINT ( 'NONE',  ( 814.5518280994195948, -183.7255117493290015, -332.4837098697145734 ) ) ;
#38110 = CARTESIAN_POINT ( 'NONE',  ( 801.1904061080336987, -68.08914811296575920, 368.3070685750235498 ) ) ;
#38111 = CARTESIAN_POINT ( 'NONE',  ( 759.0252816721024374, -168.9982390220563673, 368.0189434323527280 ) ) ;
#38112 = VECTOR ( 'NONE', #40811, 1000.000000000000000 ) ;
#38113 = CARTESIAN_POINT ( 'NONE',  ( 180.7583438952258348, 394.6698570112193920, -274.9999999999999432 ) ) ;
#38114 = EDGE_CURVE ( 'NONE', #26522, #45491, #30183, .T. ) ;
#38115 = PLANE ( 'NONE',  #32088 ) ;
#38116 = CARTESIAN_POINT ( 'NONE',  ( 810.1134526219336749, -272.5328690171413086, -357.8822607201570349 ) ) ;
#38117 = CARTESIAN_POINT ( 'NONE',  ( 746.4236121716829757, -399.8272453906067767, 328.8385539511384650 ) ) ;
#38118 = CARTESIAN_POINT ( 'NONE',  ( 748.9653473494363425, -290.6346026584195101, -356.9462024416521331 ) ) ;
#38119 = DIRECTION ( 'NONE',  ( 5.551115123125783688E-16, 1.000000000000000000, 0.000000000000000000 ) ) ;
#38120 = CARTESIAN_POINT ( 'NONE',  ( 792.2312462859673587, -395.9073299311465348, 307.2067596250082602 ) ) ;
#38121 = CARTESIAN_POINT ( 'NONE',  ( 772.4837098697145166, -23.36187538569319244, 374.5518280994205611 ) ) ;
#38122 = CARTESIAN_POINT ( 'NONE',  ( 795.1360043628807261, -356.0891481129647218, -360.2193346964456282 ) ) ;
#38123 = CONICAL_SURFACE ( 'NONE', #21898, 8.024999999999948841, 0.7853981633963380560 ) ;
#38124 = CARTESIAN_POINT ( 'NONE',  ( 763.2154366446407039, -21.62377810805121570, 321.4292242960311228 ) ) ;
#38125 = CARTESIAN_POINT ( 'NONE',  ( 778.2165204200184689, -190.8164208402381234, -364.9363028652563230 ) ) ;
#38126 = CARTESIAN_POINT ( 'NONE',  ( 776.2433038121456548, -36.89650538077844288, -374.8207195650711014 ) ) ;
#38127 = CARTESIAN_POINT ( 'NONE',  ( 789.9200121543843807, -145.9874144716871740, -317.0176451133914384 ) ) ;
#38128 = CARTESIAN_POINT ( 'NONE',  ( 800.1688906516307043, -178.1692326535052473, 369.0717654672308186 ) ) ;
#38129 = DIRECTION ( 'NONE',  ( 1.000000000000000000, 4.625929269271485914E-16, 0.000000000000000000 ) ) ;
#38130 = ORIENTED_EDGE ( 'NONE', *, *, #7470, .T. ) ;
#38131 = CARTESIAN_POINT ( 'NONE',  ( 762.1405469898971887, -49.54369356751129061, -357.8594530101015607 ) ) ;
#38132 = CARTESIAN_POINT ( 'NONE',  ( 789.9200121543843807, -169.9874144716871172, -317.0176451133914384 ) ) ;
#38133 = CARTESIAN_POINT ( 'NONE',  ( 768.0187753319979720, -176.6346026584199933, 318.0580252608186242 ) ) ;
#38134 = CARTESIAN_POINT ( 'NONE',  ( 815.1787889125755555, -6.896505380778533478, -343.7953271457877804 ) ) ;
#38135 = CARTESIAN_POINT ( 'NONE',  ( 774.6858677611749044, -297.7255117493286889, 315.5713283507209894 ) ) ;
#38136 = LINE ( 'NONE', #23782, #30855 ) ;
#38137 = ORIENTED_EDGE ( 'NONE', *, *, #2079, .F. ) ;
#38138 = CARTESIAN_POINT ( 'NONE',  ( 787.6308680596127942, -11.26014174441488258, 364.1105419155492768 ) ) ;
#38139 = CARTESIAN_POINT ( 'NONE',  ( 752.7379699480933368, -324.0090635724251911, -361.9858362298580232 ) ) ;
#38140 = VECTOR ( 'NONE', #36215, 1000.000000000000000 ) ;
#38141 = CARTESIAN_POINT ( 'NONE',  ( 751.9810565676468741, -266.0891481129651197, 360.9747183278973921 ) ) ;
#38142 = CARTESIAN_POINT ( 'NONE',  ( 754.7162404726377645, -326.7363362996979390, 339.4709603349214717 ) ) ;
#38143 = CARTESIAN_POINT ( 'NONE',  ( 787.6308680596127942, -419.2601417444136587, 364.1105419155492768 ) ) ;
#38144 = CARTESIAN_POINT ( 'NONE',  ( 763.8424801807145741, -138.0090635724257311, -320.5453621957614700 ) ) ;
#38145 = CARTESIAN_POINT ( 'NONE',  ( 757.8323909638827445, -122.6346026584201354, -352.1044303154654358 ) ) ;
#38146 = CARTESIAN_POINT ( 'NONE',  ( 794.9819416627830151, -300.9982390220559409, -319.9864689768909898 ) ) ;
#38147 = VERTEX_POINT ( 'NONE', #23764 ) ;
#38148 = VECTOR ( 'NONE', #36553, 1000.000000000000000 ) ;
#38149 = CARTESIAN_POINT ( 'NONE',  ( 763.2154366446407039, -333.6237781080502600, 321.4292242960311228 ) ) ;
#38150 = CARTESIAN_POINT ( 'NONE',  ( -265.7583438952258916, 290.0000000000001137, -244.9999999999999716 ) ) ;
#38151 = AXIS2_PLACEMENT_3D ( 'NONE', #12797, #29673, #40748 ) ;
#38152 = CARTESIAN_POINT ( 'NONE',  ( 757.0176451133909268, -109.0999726633349241, 349.9200121543848354 ) ) ;
#38153 = CARTESIAN_POINT ( 'NONE',  ( 771.2633955100217236, -23.90732993114773919, 363.4237431249939618 ) ) ;
#38154 = ORIENTED_EDGE ( 'NONE', *, *, #24465, .T. ) ;
#38155 = CARTESIAN_POINT ( 'NONE',  ( 814.8207195650702488, -386.1908817542432075, -336.2433038121456548 ) ) ;
#38156 = ADVANCED_FACE ( 'NONE', ( #29806 ), #22797, .F. ) ;
#38157 = FACE_OUTER_BOUND ( 'NONE', #27122, .T. ) ;
#38158 = CARTESIAN_POINT ( 'NONE',  ( 768.9521613784389729, -225.8272453906072599, 373.2346286133773106 ) ) ;
#38159 = CARTESIAN_POINT ( 'NONE',  ( 802.7791456095903868, -196.7146871989598083, 329.0155153010375102 ) ) ;
#38160 = CARTESIAN_POINT ( 'NONE',  ( 755.3201227861273992, -339.7255117493285184, -345.3687786644892981 ) ) ;
#38161 = PRESENTATION_STYLE_ASSIGNMENT (( #24041 ) ) ;
#38162 = CARTESIAN_POINT ( 'NONE',  ( 786.5483106153019435, -175.6454272087892718, -364.1601925771022366 ) ) ;
#38163 = EDGE_CURVE ( 'NONE', #19824, #1441, #30479, .T. ) ;
#38164 = CARTESIAN_POINT ( 'NONE',  ( -919.9999999999993179, 219.9999999999998863, 339.9999999999999432 ) ) ;
#38165 = CARTESIAN_POINT ( 'NONE',  ( 751.9810565676468741, -434.0891481129646081, -360.9747183278973921 ) ) ;
#38166 = CARTESIAN_POINT ( 'NONE',  ( 775.4999999999993179, -365.3551492539851893, -18.13243251470705886 ) ) ;
#38167 = CARTESIAN_POINT ( 'NONE',  ( 746.4236121716829757, -351.8272453906068336, 328.8385539511384650 ) ) ;
#38168 = CARTESIAN_POINT ( 'NONE',  ( -959.5497976682736407, 240.0000000000002274, -2132.806278688367456 ) ) ;
#38169 = CARTESIAN_POINT ( 'NONE',  ( 763.0537975583475827, -288.4527844766014937, 371.0346526505627480 ) ) ;
#38170 = CARTESIAN_POINT ( 'NONE',  ( 772.4837098697144029, -47.36187538569312494, -374.5518280994205611 ) ) ;
#38171 = CARTESIAN_POINT ( 'NONE',  ( 805.1927285166397041, -232.8164208402379245, -341.8018195045277707 ) ) ;
#38172 = CARTESIAN_POINT ( 'NONE',  ( -775.4999999999993179, -359.5698779088871788, -26.28906389436296109 ) ) ;
#38173 = CARTESIAN_POINT ( 'NONE',  ( 788.7366044899766848, -395.9073299311465348, 316.5762568750059813 ) ) ;
#38174 = CARTESIAN_POINT ( 'NONE',  ( 805.2837595273609850, -146.7363362996984506, 340.5290396650784714 ) ) ;
#38175 = CARTESIAN_POINT ( 'NONE',  ( 786.2694204179717872, -21.28179084515337749, -305.1769319972829067 ) ) ;
#38176 = CARTESIAN_POINT ( 'NONE',  ( 794.1144889064781864, -58.16923265350564520, -360.9840315886528401 ) ) ;
#38177 = CARTESIAN_POINT ( 'NONE',  ( 744.8212110874229666, -66.89650538077835051, 336.2046728542121627 ) ) ;
#38178 = CARTESIAN_POINT ( 'NONE',  ( 791.9812246680005501, -380.6346026584192828, 361.9419747391813189 ) ) ;
#38179 = VECTOR ( 'NONE', #9322, 1000.000000000000000 ) ;
#38180 = DIRECTION ( 'NONE',  ( -1.000000000000000000, -0.000000000000000000, 0.000000000000000000 ) ) ;
#38181 = DIRECTION ( 'NONE',  ( 0.000000000000000000, -1.000000000000000000, 1.672022627447524993E-16 ) ) ;
#38182 = CARTESIAN_POINT ( 'NONE',  ( 767.8955696845333705, -432.4527844766008684, 362.1676090361162323 ) ) ;
#38183 = EDGE_LOOP ( 'NONE', ( #26719, #5572 ) ) ;
#38184 = CARTESIAN_POINT ( 'NONE',  ( 771.2633955100217236, -47.90732993114767169, -363.4237431249939618 ) ) ;
#38185 = CARTESIAN_POINT ( 'NONE',  ( 787.6308680596127942, -347.2601417444138860, -364.1105419155492768 ) ) ;
#38186 = EDGE_CURVE ( 'NONE', #5395, #18090, #9253, .T. ) ;
#38188 = CARTESIAN_POINT ( 'NONE',  ( 771.2633955100217236, -191.9073299311471885, 363.4237431249939618 ) ) ;
#38187 = CARTESIAN_POINT ( 'NONE',  ( 804.4286716492782716, -185.3618753856926844, 345.3141322388244703 ) ) ;
#38189 = CARTESIAN_POINT ( 'NONE',  ( 747.3154664389472828, -355.9874144716865203, -326.4474001241230781 ) ) ;
#38190 = CYLINDRICAL_SURFACE ( 'NONE', #41904, 2.749999999999863665 ) ;
#38191 = VERTEX_POINT ( 'NONE', #27029 ) ;
#38192 = CARTESIAN_POINT ( 'NONE',  ( 795.1360043628807261, -404.0891481129646081, 360.2193346964456282 ) ) ;
#38193 = VERTEX_POINT ( 'NONE', #26342 ) ;
#38194 = CARTESIAN_POINT ( 'NONE',  ( 763.0537975583475827, -216.4527844766016926, -371.0346526505627480 ) ) ;
#38195 = CARTESIAN_POINT ( 'NONE',  ( 813.1304606946831655, -137.9073299311473875, 352.3570229623691716 ) ) ;
#38196 = VERTEX_POINT ( 'NONE', #10562 ) ;
#38197 = CARTESIAN_POINT ( 'NONE',  ( 797.6776695296629214, -211.5436935675107861, -357.6776695296636603 ) ) ;
#38198 = VERTEX_POINT ( 'NONE', #6472 ) ;
#38199 = CARTESIAN_POINT ( 'NONE',  ( 757.8323909638827445, -362.6346026584194533, -352.1044303154654358 ) ) ;
#38200 = CARTESIAN_POINT ( 'NONE',  ( 755.3201227861273992, -27.72551174932954510, -345.3687786644892981 ) ) ;
#38201 = CARTESIAN_POINT ( 'NONE',  ( 755.0488828828309806, -209.8055962898687881, 344.1219089521771934 ) ) ;
#38202 = CARTESIAN_POINT ( 'NONE',  ( -454.7528517110260964, 240.0000000000001421, 350.0000000000000000 ) ) ;
#38203 = DIRECTION ( 'NONE',  ( -1.000000000000000000, 0.000000000000000000, 0.000000000000000000 ) ) ;
#38204 = ADVANCED_FACE ( 'NONE', ( #45266 ), #2779, .T. ) ;
#38205 = VERTEX_POINT ( 'NONE', #39037 ) ;
#38206 = CARTESIAN_POINT ( 'NONE',  ( 800.2193346964447755, 5.001760977943074948, -355.1360043628815788 ) ) ;
#38207 = LINE ( 'NONE', #6330, #15268 ) ;
#38208 = EDGE_LOOP ( 'NONE', ( #38655, #45589, #39840, #18888 ) ) ;
#38209 = CARTESIAN_POINT ( 'NONE',  ( 757.7880784355613741, -234.0090635724255037, -312.4576283171834916 ) ) ;
#38210 = CARTESIAN_POINT ( 'NONE',  ( 747.6481478633932056, -133.0999726633348246, 353.4146539503763620 ) ) ;
#38211 = VECTOR ( 'NONE', #27783, 1000.000000000000000 ) ;
#38213 = CARTESIAN_POINT ( 'NONE',  ( 804.6798772138708955, -231.7255117493288310, -334.6312213355107019 ) ) ;
#38212 = CARTESIAN_POINT ( 'NONE',  ( -338.8365100919713200, 240.0000000000001137, -199.9999999999917861 ) ) ;
#38214 = CARTESIAN_POINT ( 'NONE',  ( 759.2295555964440155, -400.1692326535045936, -353.9708237608231229 ) ) ;
#38215 = DIRECTION ( 'NONE',  ( 0.000000000000000000, 0.000000000000000000, 1.000000000000000000 ) ) ;
#38216 = FACE_OUTER_BOUND ( 'NONE', #12284, .T. ) ;
#38217 = CARTESIAN_POINT ( 'NONE',  ( 802.9823548866075953, -73.09997266333502353, -330.0799878456151077 ) ) ;
#38218 = ADVANCED_FACE ( 'NONE', ( #20996 ), #13402, .T. ) ;
#38219 = CARTESIAN_POINT ( 'NONE',  ( 814.2805881961230625, -385.6454272087888171, 331.2368401574024119 ) ) ;
#38220 = DIRECTION ( 'NONE',  ( -1.000000000000000000, 0.000000000000000000, -0.000000000000000000 ) ) ;
#38221 = CARTESIAN_POINT ( 'NONE',  ( 752.4576283171824116, 2.921676437403253779, -317.7880784355627952 ) ) ;
#38222 = CARTESIAN_POINT ( 'NONE',  ( 792.3570229623691148, -285.1800572038741279, -373.1304606946836770 ) ) ;
#38223 = FACE_BOUND ( 'NONE', #35906, .T. ) ;
#38224 = CYLINDRICAL_SURFACE ( 'NONE', #9894, 2.749999999999835687 ) ;
#38225 = CARTESIAN_POINT ( 'NONE',  ( 797.8594530101008786, -85.54369356751118403, -322.1405469898980982 ) ) ;
#38226 = CARTESIAN_POINT ( 'NONE',  ( 786.2694204179717872, -213.2817908451527842, 305.1769319972829067 ) ) ;
#38227 = CARTESIAN_POINT ( 'NONE',  ( 786.2056067578752163, -179.8055962898688733, -374.4686193811670023 ) ) ;
#38228 = CARTESIAN_POINT ( 'NONE',  ( 800.9747183278959710, -180.9982390220563389, 311.9810565676471583 ) ) ;
#38229 = CARTESIAN_POINT ( 'NONE',  ( 804.7487373415286811, -403.5436935675101608, -364.7487373415288516 ) ) ;
#38230 = PLANE ( 'NONE',  #329 ) ;
#38231 = CARTESIAN_POINT ( 'NONE',  ( 803.6646147819161570, -281.9073299311468759, 348.8264449731210561 ) ) ;
#38232 = CARTESIAN_POINT ( 'NONE',  ( 754.7162404726377645, -62.73633629969871350, 339.4709603349214717 ) ) ;
#38233 = ADVANCED_FACE ( 'NONE', ( #3464 ), #16871, .F. ) ;
#38234 = CARTESIAN_POINT ( 'NONE',  ( 764.8639956371174549, -416.0891481129645513, -319.7806653035542013 ) ) ;
#38235 = DIRECTION ( 'NONE',  ( 1.892425610156518601E-16, 1.000000000000000000, 0.000000000000000000 ) ) ;
#38237 = EDGE_CURVE ( 'NONE', #17262, #10523, #19868, .T. ) ;
#38236 = DIRECTION ( 'NONE',  ( 0.000000000000000000, 0.000000000000000000, -1.000000000000000000 ) ) ;
#38239 = CARTESIAN_POINT ( 'NONE',  ( 804.4286716492782716, -329.3618753856922581, 345.3141322388244703 ) ) ;
#38238 = CARTESIAN_POINT ( 'NONE',  ( 795.9930595647434757, -123.0783235625963385, 320.7433823573372820 ) ) ;
#38240 = ORIENTED_EDGE ( 'NONE', *, *, #23484, .T. ) ;
#38241 = CARTESIAN_POINT ( 'NONE',  ( 795.9930595647434757, -243.0783235625959833, -320.7433823573372820 ) ) ;
#38242 = EDGE_CURVE ( 'NONE', #26190, #15909, #219, .T. ) ;
#38243 = CARTESIAN_POINT ( 'NONE',  ( 803.6646147819161570, -89.90732993114750116, 348.8264449731210561 ) ) ;
#38244 = CARTESIAN_POINT ( 'NONE',  ( 814.8230680027162407, -269.8055962898686175, -333.7305795820267917 ) ) ;
#38245 = FACE_OUTER_BOUND ( 'NONE', #7992, .T. ) ;
#38246 = CARTESIAN_POINT ( 'NONE',  ( 754.0944755984390895, -423.6237781080499190, 364.1009440267246760 ) ) ;
#38247 = VERTEX_POINT ( 'NONE', #41813 ) ;
#38248 = CARTESIAN_POINT ( 'NONE',  ( 762.1405469898971887, -289.5436935675103882, 357.8594530101015607 ) ) ;
#38249 = CIRCLE ( 'NONE', #8024, 8.025000000000003908 ) ;
#38250 = CARTESIAN_POINT ( 'NONE',  ( 805.1016975059191054, -30.89650538077846065, -343.0745993439771837 ) ) ;
#38251 = CARTESIAN_POINT ( 'NONE',  ( 778.2165204200184689, -190.8164208402381234, -364.9363028652563230 ) ) ;
#38252 = CARTESIAN_POINT ( 'NONE',  ( 788.7366044899766848, -419.9073299311465348, 316.5762568750059813 ) ) ;
#38253 = CARTESIAN_POINT ( 'NONE',  ( 745.4481719005789273, -123.7255117493292147, -347.5162901302853129 ) ) ;
#38254 = CARTESIAN_POINT ( 'NONE',  ( 792.1044303154646968, -108.4527844766020053, -317.8323909638837677 ) ) ;
#38255 = ORIENTED_EDGE ( 'NONE', *, *, #39421, .T. ) ;
#38256 = CARTESIAN_POINT ( 'NONE',  ( 804.8461984189677878, -50.19088175424420939, -336.9566956441385628 ) ) ;
#38257 = CARTESIAN_POINT ( 'NONE',  ( 779.4763451958990572, -392.7363362996977116, -365.0264073115438919 ) ) ;
#38258 = EDGE_CURVE ( 'NONE', #16020, #15909, #3222, .T. ) ;
#38260 = CARTESIAN_POINT ( 'NONE',  ( 790.9844846989617508, -454.3726999360611103, 317.2208543904092721 ) ) ;
#38259 = CARTESIAN_POINT ( 'NONE',  ( 800.0135310231082713, -134.0891481129655745, 325.0180583372163028 ) ) ;
#38261 = CARTESIAN_POINT ( 'NONE',  ( 799.4546378042377910, -105.0783235625964096, 356.1575198192848006 ) ) ;
#38264 = CARTESIAN_POINT ( 'NONE',  ( 771.2368401574024119, -373.4419599262319593, 374.2805881961240857 ) ) ;
#38263 = LINE ( 'NONE', #13096, #2614 ) ;
#38262 = DIRECTION ( 'NONE',  ( 0.000000000000000000, 0.3835384033298669948, -0.9235249282889858025 ) ) ;
#38265 = EDGE_CURVE ( 'NONE', #40312, #18427, #42720, .T. ) ;
#38266 = ORIENTED_EDGE ( 'NONE', *, *, #8889, .T. ) ;
#38267 = CARTESIAN_POINT ( 'NONE',  ( 775.8780910478218402, -345.2817908451523863, -364.9511171171680530 ) ) ;
#38268 = CARTESIAN_POINT ( 'NONE',  ( 754.8072714833581358, -364.8164208402374697, -338.1981804954720587 ) ) ;
#38269 = CARTESIAN_POINT ( 'NONE',  ( 755.8990559732751535, -131.4636090269711985, -365.9055244015606831 ) ) ;
#38270 = CARTESIAN_POINT ( 'NONE',  ( 754.3581564841646241, -41.46360902697149697, 316.1443688327762516 ) ) ;
#38272 = DIRECTION ( 'NONE',  ( -1.000000000000000000, -4.625929269271485914E-16, -0.000000000000000000 ) ) ;
#38271 = CYLINDRICAL_SURFACE ( 'NONE', #41817, 10.00000000000006395 ) ;
#38273 = CARTESIAN_POINT ( 'NONE',  ( 760.5453621957607311, -309.0783235625957559, -323.8424801807151425 ) ) ;
#38274 = CARTESIAN_POINT ( 'NONE',  ( 814.8207195650702488, -146.1908817542438896, -336.2433038121456548 ) ) ;
#38275 = LINE ( 'NONE', #40085, #38533 ) ;
#38277 = EDGE_CURVE ( 'NONE', #4067, #36764, #23997, .T. ) ;
#38276 = DIRECTION ( 'NONE',  ( -1.000000000000000000, -0.000000000000000000, 0.000000000000000000 ) ) ;
#38278 = EDGE_CURVE ( 'NONE', #17174, #8754, #27474, .T. ) ;
#38279 = CARTESIAN_POINT ( 'NONE',  ( 773.4516893846965786, -331.6454272087888171, 315.8398074228977066 ) ) ;
#38280 = CARTESIAN_POINT ( 'NONE',  ( 797.8822607201568644, -318.5545181178796952, 370.1134526219340160 ) ) ;
#38281 = CARTESIAN_POINT ( 'NONE',  ( 777.5031285880264704, -166.8164208402382087, -374.9108240113588408 ) ) ;
#38282 = CARTESIAN_POINT ( 'NONE',  ( 794.9999999999993179, -365.3551492539851893, -18.13243251470705886 ) ) ;
#38283 = CARTESIAN_POINT ( 'NONE',  ( 786.2694204179717872, -117.2817908451530684, 305.1769319972829067 ) ) ;
#38284 = CARTESIAN_POINT ( 'NONE',  ( 772.5602148656447525, -321.7255117493286320, -305.7998596910095443 ) ) ;
#38285 = CARTESIAN_POINT ( 'NONE',  ( 799.9999999999993179, 205.0000000000000568, 319.9999999999999432 ) ) ;
#38286 = DIRECTION ( 'NONE',  ( 0.000000000000000000, 0.000000000000000000, -1.000000000000000000 ) ) ;
#38287 = CARTESIAN_POINT ( 'NONE',  ( 804.4286716492782716, -185.3618753856926844, 345.3141322388244703 ) ) ;
#38288 = ORIENTED_EDGE ( 'NONE', *, *, #33206, .T. ) ;
#38289 = CARTESIAN_POINT ( 'NONE',  ( 811.3240766477731540, -436.3726999360612240, 355.6651683502462902 ) ) ;
#38290 = CARTESIAN_POINT ( 'NONE',  ( 764.3348316497523456, -382.7146871989591546, -308.6759233522265617 ) ) ;
#38291 = CARTESIAN_POINT ( 'NONE',  ( 758.8095938919642549, -128.0891481129655176, -311.6929314249763365 ) ) ;
#38292 = CARTESIAN_POINT ( 'NONE',  ( 759.0159684113467620, -64.91815448151686496, 325.8855110935213020 ) ) ;
#38293 = CARTESIAN_POINT ( 'NONE',  ( 801.1904061080336987, -404.0891481129646081, -368.3070685750235498 ) ) ;
#38295 = EDGE_CURVE ( 'NONE', #12731, #40960, #2892, .T. ) ;
#38294 = DIRECTION ( 'NONE',  ( 0.000000000000000000, -0.000000000000000000, 1.000000000000000000 ) ) ;
#38296 = CARTESIAN_POINT ( 'NONE',  ( 759.8311093483677041, 1.830767346494167391, 310.9282345327691814 ) ) ;
#38297 = ORIENTED_EDGE ( 'NONE', *, *, #37393, .F. ) ;
#38298 = CARTESIAN_POINT ( 'NONE',  ( 745.1769319972822814, -161.8055962898689870, -346.2694204179732083 ) ) ;
#38299 = CARTESIAN_POINT ( 'NONE',  ( 784.9999999999992042, 239.9999999999999432, -244.9999999999999716 ) ) ;
#38300 = CARTESIAN_POINT ( 'NONE',  ( 814.8230680027162407, -269.8055962898686175, 333.7305795820267917 ) ) ;
#38301 = CARTESIAN_POINT ( 'NONE',  ( 795.1360043628808398, -116.0891481129656313, 360.2193346964456282 ) ) ;
#38302 = ORIENTED_EDGE ( 'NONE', *, *, #1788, .F. ) ;
#38303 = CARTESIAN_POINT ( 'NONE',  ( 762.3223304703356007, -295.5436935675105588, 322.3223304703362828 ) ) ;
#38304 = CARTESIAN_POINT ( 'NONE',  ( 815.2698199232961542, -16.81642084023866701, -342.5225473063383106 ) ) ;
#38305 = CARTESIAN_POINT ( 'NONE',  ( 791.4252870525732533, -448.2207382684695176, 369.1877814561917717 ) ) ;
#38306 = ORIENTED_EDGE ( 'NONE', *, *, #30524, .T. ) ;
#38307 = CARTESIAN_POINT ( 'NONE',  ( 745.7194118038753459, -421.6454272087885329, -348.7631598425976449 ) ) ;
#38308 = VECTOR ( 'NONE', #17782, 1000.000000000000000 ) ;
#38309 = EDGE_CURVE ( 'NONE', #22342, #39117, #41572, .T. ) ;
#38310 = CARTESIAN_POINT ( 'NONE',  ( 802.1676090361156639, -14.63460265842049424, 327.8955696845344505 ) ) ;
#38311 = CARTESIAN_POINT ( 'NONE',  ( 756.3353852180819104, -269.9073299311468190, -331.1735550268788302 ) ) ;
#38313 = CARTESIAN_POINT ( 'NONE',  ( 752.4576283171824116, -261.0783235625959264, 317.7880784355627952 ) ) ;
#38312 = CARTESIAN_POINT ( 'NONE',  ( 754.9967657858570647, -361.5436935675103882, 365.0032342141425943 ) ) ;
#38314 = EDGE_CURVE ( 'NONE', #43845, #43683, #692, .T. ) ;
#38315 = CARTESIAN_POINT ( 'NONE',  ( 804.4086373105744769, -265.6454272087889876, -333.3843516231986541 ) ) ;
#38316 = CARTESIAN_POINT ( 'NONE',  ( 785.3141322388236176, -237.7255117493289163, -364.4286716492789537 ) ) ;
#38317 = CARTESIAN_POINT ( 'NONE',  ( 768.0187753319979720, -440.6346026584191122, -318.0580252608186242 ) ) ;
#38318 = CARTESIAN_POINT ( 'NONE',  ( 795.1360043628807261, -92.08914811296568814, -360.2193346964456282 ) ) ;
#38319 = CARTESIAN_POINT ( 'NONE',  ( 755.5713283507202505, -245.3618753856925139, 334.6858677611754729 ) ) ;
#38320 = VERTEX_POINT ( 'NONE', #6689 ) ;
#38321 = CARTESIAN_POINT ( 'NONE',  ( 777.4774526936600978, -370.2709662947831362, 304.7301800767027657 ) ) ;
#38322 = LINE ( 'NONE', #31827, #32988 ) ;
#38323 = CARTESIAN_POINT ( 'NONE',  ( 776.2046728542105711, -44.19088175424421649, -304.8212110874238761 ) ) ;
#38324 = CARTESIAN_POINT ( 'NONE',  ( 914.9999999999992042, 74.99999999999984368, 360.0000000000000000 ) ) ;
#38325 = FACE_OUTER_BOUND ( 'NONE', #22895, .T. ) ;
#38326 = CARTESIAN_POINT ( 'NONE',  ( 805.2837595273609850, -218.7363362996982232, 340.5290396650784714 ) ) ;
#38327 = CARTESIAN_POINT ( 'NONE',  ( 771.1735550268778070, -129.1800572038746111, 316.3353852180827630 ) ) ;
#38328 = ORIENTED_EDGE ( 'NONE', *, *, #6873, .T. ) ;
#38329 = CARTESIAN_POINT ( 'NONE',  ( 776.9254006560222479, -20.19088175424429110, -314.8983024940802125 ) ) ;
#38330 = CARTESIAN_POINT ( 'NONE',  ( 767.6429770376291799, -57.18005720387490243, -306.8695393053162093 ) ) ;
#38331 = CARTESIAN_POINT ( 'NONE',  ( 798.7617431975189675, -291.6237781080503169, 323.0428371773161871 ) ) ;
#38332 = CARTESIAN_POINT ( 'NONE',  ( 756.3353852180819104, -437.9073299311463074, -331.1735550268788302 ) ) ;
#38333 = CARTESIAN_POINT ( 'NONE',  ( 755.0636971347428243, -52.27096629478401724, -341.7834795799807353 ) ) ;
#38334 = CARTESIAN_POINT ( 'NONE',  ( 771.3260364891663130, 4.354572791210176597, 306.0683387631859773 ) ) ;
#38335 = CARTESIAN_POINT ( 'NONE',  ( 805.0032342141412300, -205.5436935675108430, -314.9967657858571783 ) ) ;
#38336 = CARTESIAN_POINT ( 'NONE',  ( 801.1904061080336987, -164.0891481129655176, 368.3070685750235498 ) ) ;
#38337 = CARTESIAN_POINT ( 'NONE',  ( 800.2193346964447755, -90.99823902205663728, 355.1360043628815788 ) ) ;
#38338 = CARTESIAN_POINT ( 'NONE',  ( -208.8365100919714052, 260.0000000000001137, -202.7499999999925251 ) ) ;
#38339 = LINE ( 'NONE', #16635, #6270 ) ;
#38340 = CARTESIAN_POINT ( 'NONE',  ( 744.8212110874229666, -282.8965053807776258, -336.2046728542121627 ) ) ;
#38341 = AXIS2_PLACEMENT_3D ( 'NONE', #770, #4250, #15087 ) ;
#38342 = CARTESIAN_POINT ( 'NONE',  ( 814.2805881961230625, -433.6454272087884760, 331.2368401574024119 ) ) ;
#38343 = CARTESIAN_POINT ( 'NONE',  ( 744.7301800767019131, -268.8164208402378108, -337.4774526936615757 ) ) ;
#38344 = DIRECTION ( 'NONE',  ( -1.000000000000000000, -0.000000000000000000, -0.000000000000000000 ) ) ;
#38345 = CARTESIAN_POINT ( 'NONE',  ( 746.8695393053150156, -389.9073299311465348, 327.6429770376306010 ) ) ;
#38346 = CARTESIAN_POINT ( 'NONE',  ( 767.7687537140311633, -47.90732993114767169, 372.7932403749916830 ) ) ;
#38347 = CARTESIAN_POINT ( 'NONE',  ( 804.9363028652555840, -400.2709662947828519, -338.2165204200192079 ) ) ;
#38348 = CARTESIAN_POINT ( 'NONE',  ( 755.8398074228967971, -19.44195992623303937, 333.4516893846970333 ) ) ;
#38349 = CARTESIAN_POINT ( 'NONE',  ( 758.0141637701419768, -63.07832356259653750, -367.2620300519063790 ) ) ;
#38350 = CARTESIAN_POINT ( 'NONE',  ( 780.5290396650775619, -180.3510508353234343, -365.2837595273619513 ) ) ;
#38351 = CARTESIAN_POINT ( 'NONE',  ( 748.3538107759620743, -184.7146871989598083, 355.8262568251490165 ) ) ;
#38352 = CARTESIAN_POINT ( 'NONE',  ( 755.3201227861273992, -27.72551174932954510, 345.3687786644892981 ) ) ;
#38353 = CARTESIAN_POINT ( 'NONE',  ( 761.9338519418445230, -182.5328690171416497, 370.4231160770881957 ) ) ;
#38354 = VERTEX_POINT ( 'NONE', #27709 ) ;
#38355 = CARTESIAN_POINT ( 'NONE',  ( 804.6798772138708955, -63.72551174932939233, -334.6312213355107019 ) ) ;
#38356 = CARTESIAN_POINT ( 'NONE',  ( 761.2382568024794409, -207.6237781080506295, -356.9571628226838129 ) ) ;
#38357 = CARTESIAN_POINT ( 'NONE',  ( 762.1405469898971887, -169.5436935675108430, 357.8594530101015607 ) ) ;
#38358 = CARTESIAN_POINT ( 'NONE',  ( 793.4146539503750546, -1.987414471687640294, -307.6481478633938877 ) ) ;
#38359 = CARTESIAN_POINT ( 'NONE',  ( 756.5762568750052424, -315.1800572038740711, 348.7366044899774238 ) ) ;
#38360 = FACE_OUTER_BOUND ( 'NONE', #31299, .T. ) ;
#38361 = ORIENTED_EDGE ( 'NONE', *, *, #4352, .T. ) ;
#38362 = CARTESIAN_POINT ( 'NONE',  ( 769.1273215169530886, -22.71468719896029853, 317.4527132478988847 ) ) ;
#38363 = CARTESIAN_POINT ( 'NONE',  ( 762.1177392798416577, -306.5545181178797520, -309.8865473780659272 ) ) ;
#38364 = CARTESIAN_POINT ( 'NONE',  ( 746.8695393053151292, -269.9073299311469327, 327.6429770376306578 ) ) ;
#38365 = CARTESIAN_POINT ( 'NONE',  ( 775.8780910478218402, -345.2817908451523863, 364.9511171171680530 ) ) ;
#38366 = CARTESIAN_POINT ( 'NONE',  ( 800.7704444035546203, -436.1692326535044231, 326.0291762391768771 ) ) ;
#38367 = CARTESIAN_POINT ( 'NONE',  ( 802.5472867521000353, -148.3726999360620198, -350.8726784830461156 ) ) ;
#38368 = CARTESIAN_POINT ( 'NONE',  ( 788.7366044899766848, -131.9073299311473875, -316.5762568750059813 ) ) ;
#38369 = CARTESIAN_POINT ( 'NONE',  ( 797.6776695296629214, -307.5436935675104451, -357.6776695296636603 ) ) ;
#38370 = ORIENTED_EDGE ( 'NONE', *, *, #44398, .T. ) ;
#38371 = CARTESIAN_POINT ( 'NONE',  ( 799.4546378042377910, -321.0783235625956991, 356.1575198192848006 ) ) ;
#38372 = DIRECTION ( 'NONE',  ( -0.000000000000000000, -0.000000000000000000, 1.000000000000000000 ) ) ;
#38373 = CARTESIAN_POINT ( 'NONE',  ( 772.4468031744293057, -105.8272453906076578, 363.8651313633793620 ) ) ;
#38374 = CARTESIAN_POINT ( 'NONE',  ( 802.1676090361156639, -14.63460265842049424, 327.8955696845344505 ) ) ;
#38375 = VERTEX_POINT ( 'NONE', #31847 ) ;
#38376 = CARTESIAN_POINT ( 'NONE',  ( 783.7953271457878373, -392.1908817542432075, -375.1787889125761239 ) ) ;
#38377 = DIRECTION ( 'NONE',  ( 0.000000000000000000, 0.9238795325112891810, -0.3826834323650838421 ) ) ;
#38378 = CARTESIAN_POINT ( 'NONE',  ( 775.8780910478218402, -225.2817908451527273, 364.9511171171680530 ) ) ;
#38379 = CARTESIAN_POINT ( 'NONE',  ( 754.3581564841646241, -233.4636090269708575, 316.1443688327762516 ) ) ;
#38380 = CARTESIAN_POINT ( 'NONE',  ( 805.1016975059191054, -174.8965053807779952, 343.0745993439771837 ) ) ;
#38381 = CARTESIAN_POINT ( 'NONE',  ( 785.3687786644884454, -323.3618753856923149, -315.3201227861279676 ) ) ;
#38382 = LINE ( 'NONE', #34903, #21516 ) ;
#38383 = CARTESIAN_POINT ( 'NONE',  ( 757.0176451133909268, -205.0999726633346256, -349.9200121543848354 ) ) ;
#38384 = CARTESIAN_POINT ( 'NONE',  ( 754.9967657858570647, -1.543693567511449150, 365.0032342141425374 ) ) ;
#38385 = CARTESIAN_POINT ( 'NONE',  ( 808.0106897970731552, -452.9681489794447771, 338.3625385368115985 ) ) ;
#38386 = CARTESIAN_POINT ( 'NONE',  ( 815.2698199232962679, -424.8164208402373561, -342.5225473063383674 ) ) ;
#38387 = DIRECTION ( 'NONE',  ( 1.000000000000000000, 0.000000000000000000, 0.000000000000000000 ) ) ;
#38388 = CARTESIAN_POINT ( 'NONE',  ( 797.8822607201568644, -366.5545181178795815, 370.1134526219340160 ) ) ;
#38389 = CARTESIAN_POINT ( 'NONE',  ( 808.6142084849417415, -454.8672832770561740, -349.9915990122670451 ) ) ;
#38390 = CARTESIAN_POINT ( 'NONE',  ( 782.4968714119720516, -298.8164208402377540, 305.0891759886411023 ) ) ;
#38391 = CARTESIAN_POINT ( 'NONE',  ( 813.1304606946830518, -65.90732993114758642, -352.3570229623690580 ) ) ;
#38392 = CARTESIAN_POINT ( 'NONE',  ( 800.0135310231082713, -278.0891481129651197, -325.0180583372163028 ) ) ;
#38393 = DIRECTION ( 'NONE',  ( 0.000000000000000000, 0.000000000000000000, 1.000000000000000000 ) ) ;
#38394 = CARTESIAN_POINT ( 'NONE',  ( 781.8018195045266339, -406.2709662947829088, 365.1927285166406705 ) ) ;
#38395 = CARTESIAN_POINT ( 'NONE',  ( 784.1219089521767955, -165.2817908451529547, 315.0488828828318333 ) ) ;
#38396 = CARTESIAN_POINT ( 'NONE',  ( 804.1009440267234822, -23.46360902697155026, -314.0944755984392600 ) ) ;
#38397 = CARTESIAN_POINT ( 'NONE',  ( 794.1144889064781864, -34.16923265350572336, -360.9840315886528401 ) ) ;
#38398 = CARTESIAN_POINT ( 'NONE',  ( 747.3154664389472828, -67.98741447168742980, 326.4474001241230781 ) ) ;
#38399 = CARTESIAN_POINT ( 'NONE',  ( 755.5713283507202505, -389.3618753856919739, 334.6858677611754729 ) ) ;
#38400 = CARTESIAN_POINT ( 'NONE',  ( 792.2312462859673587, 12.09267006885214180, 307.2067596250082602 ) ) ;
#38401 = DIRECTION ( 'NONE',  ( 1.000000000000000000, 0.000000000000000000, -0.000000000000000000 ) ) ;
#38402 = CARTESIAN_POINT ( 'NONE',  ( 748.3538107759620743, -136.7146871989600072, 355.8262568251490165 ) ) ;
#38403 = CARTESIAN_POINT ( 'NONE',  ( 788.7366044899766848, -419.9073299311465348, 316.5762568750059813 ) ) ;
#38404 = ORIENTED_EDGE ( 'NONE', *, *, #6658, .T. ) ;
#38405 = CARTESIAN_POINT ( 'NONE',  ( 755.5713283507202505, -53.36187538569310362, -334.6858677611754729 ) ) ;
#38406 = CARTESIAN_POINT ( 'NONE',  ( 769.1273215169530886, -358.7146871989592114, -317.4527132478988847 ) ) ;
#38408 = CARTESIAN_POINT ( 'NONE',  ( 803.6646147819162707, -185.9073299311472169, 348.8264449731211130 ) ) ;
#38407 = CARTESIAN_POINT ( 'NONE',  ( 778.2165204200184689, -238.8164208402379813, 364.9363028652563230 ) ) ;
#38409 = VERTEX_POINT ( 'NONE', #42487 ) ;
#38410 = CARTESIAN_POINT ( 'NONE',  ( 808.7758568127978833, -412.1692326535045936, -320.0363995740631822 ) ) ;
#38411 = CARTESIAN_POINT ( 'NONE',  ( 187.1337867209877857, 50.81038600091411439, 193.6948738798775764 ) ) ;
#38412 = ORIENTED_EDGE ( 'NONE', *, *, #27831, .F. ) ;
#38413 = CARTESIAN_POINT ( 'NONE',  ( 758.0580252608178853, -390.4527844766011526, 328.0187753319985404 ) ) ;
#38414 = ORIENTED_EDGE ( 'NONE', *, *, #3233, .T. ) ;
#38415 = CARTESIAN_POINT ( 'NONE',  ( 758.8095938919642549, -224.0891481129653187, -311.6929314249763365 ) ) ;
#38416 = CARTESIAN_POINT ( 'NONE',  ( 800.9747183278959710, -156.9982390220564241, 311.9810565676471583 ) ) ;
#38417 = VERTEX_POINT ( 'NONE', #17557 ) ;
#38418 = CARTESIAN_POINT ( 'NONE',  ( 771.1735550268780344, -225.1800572038743553, -316.3353852180828198 ) ) ;
#38419 = VERTEX_POINT ( 'NONE', #13861 ) ;
#38420 = CARTESIAN_POINT ( 'NONE',  ( 781.8018195045266339, -358.2709662947829088, -365.1927285166406705 ) ) ;
#38421 = CARTESIAN_POINT ( 'NONE',  ( 762.1405469898971887, -1.543693567511449150, -357.8594530101015607 ) ) ;
#38422 = CARTESIAN_POINT ( 'NONE',  ( 799.4546378042377910, -225.0783235625959833, 356.1575198192848006 ) ) ;
#38423 = DIRECTION ( 'NONE',  ( 0.000000000000000000, 0.000000000000000000, 1.000000000000000000 ) ) ;
#38424 = DIRECTION ( 'NONE',  ( -1.880165489482579047E-16, -1.000000000000000000, 0.000000000000000000 ) ) ;
#38425 = PRODUCT ( 'Foot Treadle Lever Assembly', 'Foot Treadle Lever Assembly', '', ( #24650 ) ) ;
#38426 = VERTEX_POINT ( 'NONE', #20767 ) ;
#38427 = CARTESIAN_POINT ( 'NONE',  ( 784.1219089521767955, -453.2817908451519315, -315.0488828828318333 ) ) ;
#38428 = DIRECTION ( 'NONE',  ( 0.000000000000000000, 0.000000000000000000, -1.000000000000000000 ) ) ;
#38429 = ORIENTED_EDGE ( 'NONE', *, *, #26611, .T. ) ;
#38430 = CARTESIAN_POINT ( 'NONE',  ( 805.6418435158337843, -269.4636090269708006, -363.8556311672236916 ) ) ;
#38431 = CARTESIAN_POINT ( 'NONE',  ( 764.1737431748507561, -130.3726999360621619, 371.6461892240376415 ) ) ;
#38433 = CARTESIAN_POINT ( 'NONE',  ( 759.9864689768902508, -218.0891481129653187, -354.9819416627836404 ) ) ;
#38432 = CARTESIAN_POINT ( 'NONE',  ( 571.1634899080285095, 256.4999999999999432, -197.2499999999982379 ) ) ;
#38434 = CARTESIAN_POINT ( 'NONE',  ( 761.2382568024794409, -399.6237781080500326, -356.9571628226838129 ) ) ;
#38435 = CARTESIAN_POINT ( 'NONE',  ( -208.8365100919714052, 260.0000000000001137, -206.1189999999926954 ) ) ;
#38436 = FACE_BOUND ( 'NONE', #2175, .T. ) ;
#38437 = CARTESIAN_POINT ( 'NONE',  ( 758.4439275373578084, -108.5545181178803915, -353.2243759319684386 ) ) ;
#38438 = CARTESIAN_POINT ( 'NONE',  ( 778.7629533639073998, -392.7363362996977116, 375.0009284576466371 ) ) ;
#38439 = CARTESIAN_POINT ( 'NONE',  ( -829.9999999999992042, -600.0000000000000000, -319.9999999999996021 ) ) ;
#38440 = CARTESIAN_POINT ( 'NONE',  ( 805.9055244015594326, 20.37622189194865285, -315.8990559732753240 ) ) ;
#38441 = CARTESIAN_POINT ( 'NONE',  ( 755.2512626584698410, -319.5436935675104451, -315.2512626584710915 ) ) ;
#38442 =( NAMED_UNIT ( * ) SI_UNIT ( $, .STERADIAN. ) SOLID_ANGLE_UNIT ( ) );
#38443 = CARTESIAN_POINT ( 'NONE',  ( -180.7583438952258348, 394.6698570112193920, -224.9999999999999716 ) ) ;
#38444 = CARTESIAN_POINT ( 'NONE',  ( 759.7806653035534055, -78.99823902205662307, -324.8639956371180801 ) ) ;
#38445 = CARTESIAN_POINT ( 'NONE',  ( 781.2370466360911223, -236.7363362996981380, 304.9990715423533629 ) ) ;
#38446 = CARTESIAN_POINT ( 'NONE',  ( 752.4576283171824116, -165.0783235625962391, -317.7880784355627952 ) ) ;
#38447 = CARTESIAN_POINT ( 'NONE',  ( 815.2698199232961542, -184.8164208402380950, 342.5225473063383106 ) ) ;
#38448 = CARTESIAN_POINT ( 'NONE',  ( 815.2698199232961542, -448.8164208402371855, -342.5225473063383106 ) ) ;
#38449 = DIRECTION ( 'NONE',  ( 0.000000000000000000, 0.000000000000000000, 1.000000000000000000 ) ) ;
#38450 = CARTESIAN_POINT ( 'NONE',  ( 785.3687786644884454, -299.3618753856922581, 315.3201227861279676 ) ) ;
#38451 = CARTESIAN_POINT ( 'NONE',  ( 796.9571628226829034, -71.46360902697141171, 321.2382568024804641 ) ) ;
#38452 = CARTESIAN_POINT ( 'NONE',  ( 755.0636971347428243, -412.2709662947829088, -341.7834795799807353 ) ) ;
#38453 = CARTESIAN_POINT ( 'NONE',  ( -33.13011601220117086, -513.1383975375929367, -367.9999999999999432 ) ) ;
#38454 = FACE_OUTER_BOUND ( 'NONE', #32630, .T. ) ;
#38456 = CARTESIAN_POINT ( 'NONE',  ( 759.9864689768902508, -314.0891481129650629, 354.9819416627836404 ) ) ;
#38455 = CARTESIAN_POINT ( 'NONE',  ( 756.1348686366196716, -137.2601417444144829, 347.5531968255698416 ) ) ;
#38457 = EDGE_LOOP ( 'NONE', ( #44856, #19366, #45363, #38591 ) ) ;
#38458 = CARTESIAN_POINT ( 'NONE',  ( 783.0433043558608688, -264.8965053807776826, -315.1538015810313027 ) ) ;
#38459 = CARTESIAN_POINT ( 'NONE',  ( 785.3141322388236176, -93.72551174932934259, 364.4286716492789537 ) ) ;
#38460 = CARTESIAN_POINT ( 'NONE',  ( 747.3154664389472828, -283.9874144716867477, -326.4474001241230781 ) ) ;
#38461 = FACE_OUTER_BOUND ( 'NONE', #31182, .T. ) ;
#38462 = CARTESIAN_POINT ( 'NONE',  ( 795.6651683502461765, -418.7146871989590409, 371.3240766477733814 ) ) ;
#38463 = ORIENTED_EDGE ( 'NONE', *, *, #21597, .T. ) ;
#38464 = CARTESIAN_POINT ( 'NONE',  ( 803.6646147819161570, -281.9073299311468759, 348.8264449731210561 ) ) ;
#38465 = CARTESIAN_POINT ( 'NONE',  ( 756.3353852180819104, -149.9073299311473875, -331.1735550268788302 ) ) ;
#38466 = CARTESIAN_POINT ( 'NONE',  ( 767.8955696845333705, -216.4527844766016926, -362.1676090361162323 ) ) ;
#38467 = CARTESIAN_POINT ( 'NONE',  ( 774.6312213355099630, -407.3618753856920307, 364.6798772138717482 ) ) ;
#38468 = EDGE_CURVE ( 'NONE', #13695, #966, #44195, .T. ) ;
#38469 = CARTESIAN_POINT ( 'NONE',  ( 744.7301800767019131, -100.8164208402383792, -337.4774526936615757 ) ) ;
#38470 = AXIS2_PLACEMENT_3D ( 'NONE', #726, #14824, #42979 ) ;
#38471 = CARTESIAN_POINT ( 'NONE',  ( 764.8639956371174549, -104.0891481129656739, -319.7806653035542581 ) ) ;
#38472 = VERTEX_POINT ( 'NONE', #31629 ) ;
#38473 = CARTESIAN_POINT ( 'NONE',  ( 793.0897708529556667, -390.5545181178794678, -361.3366627262616362 ) ) ;
#38475 = CARTESIAN_POINT ( 'NONE',  ( 793.9708237608222134, -430.9181544815157849, 319.2295555964448681 ) ) ;
#38474 = CARTESIAN_POINT ( 'NONE',  ( 785.3141322388236176, -117.7255117493292715, 364.4286716492789537 ) ) ;
#38476 = CARTESIAN_POINT ( 'NONE',  ( 795.9930595647434757, -123.0783235625963385, 320.7433823573372820 ) ) ;
#38479 = CARTESIAN_POINT ( 'NONE',  ( 803.8556311672234642, -369.6237781080500895, 365.6418435158340117 ) ) ;
#38478 = DIRECTION ( 'NONE',  ( 1.000000000000000000, 0.000000000000000000, 0.000000000000000000 ) ) ;
#38477 = DIRECTION ( 'NONE',  ( -1.000000000000000000, -0.000000000000000000, 0.000000000000000000 ) ) ;
#38480 = EDGE_LOOP ( 'NONE', ( #7873, #80, #18920, #43365 ) ) ;
#38481 = CARTESIAN_POINT ( 'NONE',  ( 769.9779781133707957, -355.0999726633341993, -316.7813123517150871 ) ) ;
#38482 = CARTESIAN_POINT ( 'NONE',  ( 755.0636971347428243, -340.2709662947831362, -341.7834795799807353 ) ) ;
#38483 = CARTESIAN_POINT ( 'NONE',  ( 814.8207195650702488, -170.1908817542438328, -336.2433038121456548 ) ) ;
#38484 = CARTESIAN_POINT ( 'NONE',  ( 750.9282345327678740, -40.91815448151695023, 319.8311093483690115 ) ) ;
#38486 = DIRECTION ( 'NONE',  ( 0.000000000000000000, 0.000000000000000000, 1.000000000000000000 ) ) ;
#38485 = DIRECTION ( 'NONE',  ( 0.000000000000000000, 0.000000000000000000, 1.000000000000000000 ) ) ;
#38487 = CARTESIAN_POINT ( 'NONE',  ( 794.1144889064781864, -298.1692326535049347, -360.9840315886528401 ) ) ;
#38488 = CARTESIAN_POINT ( 'NONE',  ( 788.7366044899766848, -443.9073299311464780, -316.5762568750059813 ) ) ;
#38489 = CARTESIAN_POINT ( 'NONE',  ( 764.1737431748507561, -154.3726999360620198, -371.6461892240376415 ) ) ;
#38490 = CARTESIAN_POINT ( 'NONE',  ( -879.9999999999992042, 240.0000000000002274, -179.9999999999999716 ) ) ;
#38491 = CARTESIAN_POINT ( 'NONE',  ( 311.1634899080286232, 240.0000000000000000, -199.9999999999963336 ) ) ;
#38492 = CARTESIAN_POINT ( 'NONE',  ( 766.9102291470427417, -378.5545181178795247, 318.6633372737382501 ) ) ;
#38493 = CARTESIAN_POINT ( 'NONE',  ( 766.4474001241216001, -355.0999726633341993, 307.3154664389482491 ) ) ;
#38494 = CARTESIAN_POINT ( 'NONE',  ( 796.9462024416508257, -204.4527844766016926, -308.9653473494370246 ) ) ;
#38495 = CYLINDRICAL_SURFACE ( 'NONE', #21675, 10.00000000000000888 ) ;
#38496 = CARTESIAN_POINT ( 'NONE',  ( 748.6759233522253680, -136.3726999360621051, 324.3348316497537098 ) ) ;
#38497 = CARTESIAN_POINT ( 'NONE',  ( 800.9747183278959710, -348.9982390220558273, -311.9810565676471583 ) ) ;
#38498 = DIRECTION ( 'NONE',  ( 0.000000000000000000, 0.000000000000000000, 1.000000000000000000 ) ) ;
#38499 = CARTESIAN_POINT ( 'NONE',  ( 1238.921997096861332, 579.9999999999998863, -320.0000000000000000 ) ) ;
#38500 = CARTESIAN_POINT ( 'NONE',  ( 785.3687786644884454, -179.3618753856927128, 315.3201227861279676 ) ) ;
#38501 = CIRCLE ( 'NONE', #15656, 6.118999999999985562 ) ;
#38502 = VERTEX_POINT ( 'NONE', #28161 ) ;
#38503 = CARTESIAN_POINT ( 'NONE',  ( 815.3608509340175488, -410.7363362996976548, 341.2497674668889545 ) ) ;
#38504 = CARTESIAN_POINT ( 'NONE',  ( 810.1134526219336749, -368.5328690171409676, -357.8822607201570349 ) ) ;
#38505 = CARTESIAN_POINT ( 'NONE',  ( 763.0537975583475827, -120.4527844766019484, -371.0346526505627480 ) ) ;
#38506 = ADVANCED_FACE ( 'NONE', ( #42254, #10612, #24688, #14313, #35317, #3695, #5635, #29059, #25809, #4355, #39922, #4795, #19959, #22330, #5869 ), #34033, .F. ) ;
#38507 = CARTESIAN_POINT ( 'NONE',  ( 754.9967657858570647, -433.5436935675099903, -365.0032342141425374 ) ) ;
#38508 = CARTESIAN_POINT ( 'NONE',  ( 506.1531787467675940, 50.81038600091411439, -217.3872392842761769 ) ) ;
#38509 = CARTESIAN_POINT ( 'NONE',  ( 815.0009284576459549, -6.351050835323991173, 338.7629533639073429 ) ) ;
#38510 = EDGE_LOOP ( 'NONE', ( #19428, #35272 ) ) ;
#38511 = ADVANCED_FACE ( 'NONE', ( #32523 ), #9338, .F. ) ;
#38512 = CARTESIAN_POINT ( 'NONE',  ( 744.8212110874229666, -162.8965053807780521, -336.2046728542121627 ) ) ;
#38513 = FACE_BOUND ( 'NONE', #6529, .T. ) ;
#38514 = CARTESIAN_POINT ( 'NONE',  ( 812.6845335610512393, -295.9874144716866908, 353.5525998758768651 ) ) ;
#38515 = CARTESIAN_POINT ( 'NONE',  ( 801.9419747391806368, -114.4527844766020053, 351.9812246680014027 ) ) ;
#38516 = ORIENTED_EDGE ( 'NONE', *, *, #30652, .F. ) ;
#38517 = CARTESIAN_POINT ( 'NONE',  ( 756.7813123517142913, -19.98741447168758256, -329.9779781133712504 ) ) ;
#38518 = CARTESIAN_POINT ( 'NONE',  ( 756.3353852180819104, -293.9073299311468759, 331.1735550268788302 ) ) ;
#38519 = ADVANCED_FACE ( 'NONE', ( #25352 ), #11276, .F. ) ;
#38520 = CARTESIAN_POINT ( 'NONE',  ( 767.6429770376289525, -9.180057203875058747, -306.8695393053162093 ) ) ;
#38521 = AXIS2_PLACEMENT_3D ( 'NONE', #15701, #5082, #30235 ) ;
#38522 = CARTESIAN_POINT ( 'NONE',  ( 792.6574999928877787, -450.0087184351455107, 371.5677366416246059 ) ) ;
#38523 = VERTEX_POINT ( 'NONE', #16261 ) ;
#38524 = CARTESIAN_POINT ( 'NONE',  ( 776.2046728542105711, -404.1908817542431507, -304.8212110874238761 ) ) ;
#38525 = ORIENTED_EDGE ( 'NONE', *, *, #35177, .F. ) ;
#38526 = CARTESIAN_POINT ( 'NONE',  ( 805.1927285166397041, -40.81642084023859951, 341.8018195045277707 ) ) ;
#38527 = CARTESIAN_POINT ( 'NONE',  ( 755.5713283507202505, -269.3618753856924286, -334.6858677611754729 ) ) ;
#38529 = CARTESIAN_POINT ( 'NONE',  ( 744.9990715423526808, -258.3510508353231785, 341.2370466360926002 ) ) ;
#38528 = CARTESIAN_POINT ( 'NONE',  ( 810.7187646348534145, -354.4527844766012095, 356.7737145352016341 ) ) ;
#38530 = CARTESIAN_POINT ( 'NONE',  ( 813.2346286133761168, -77.26014174441466764, 328.9521613784389160 ) ) ;
#38531 = CARTESIAN_POINT ( 'NONE',  ( 800.9840315886518738, -244.9181544815162681, -354.1144889064786412 ) ) ;
#38532 = CARTESIAN_POINT ( 'NONE',  ( 795.1360043628807261, -236.0891481129651766, -360.2193346964456282 ) ) ;
#38533 = VECTOR ( 'NONE', #42650, 1000.000000000000227 ) ;
#38534 = CARTESIAN_POINT ( 'NONE',  ( 989.9999999999992042, -590.0000000000001137, 350.0000000000000000 ) ) ;
#38535 = CARTESIAN_POINT ( 'NONE',  ( 759.9864689768902508, -98.08914811296568814, -354.9819416627836404 ) ) ;
#38536 = EDGE_CURVE ( 'NONE', #3087, #35125, #36431, .T. ) ;
#38537 = CARTESIAN_POINT ( 'NONE',  ( 781.8018195045266339, -238.2709662947833920, 365.1927285166406705 ) ) ;
#38538 = CARTESIAN_POINT ( 'NONE',  ( 787.5162901302840055, -395.3618753856918602, 305.4481719005792684 ) ) ;
#38539 = CARTESIAN_POINT ( 'NONE',  ( -598.8365100919716042, 260.0000000000001705, -197.2499999999901092 ) ) ;
#38540 = EDGE_CURVE ( 'NONE', #9031, #44609, #34642, .T. ) ;
#38541 = CARTESIAN_POINT ( 'NONE',  ( 778.7629533639073998, -56.73633629969872771, -375.0009284576466371 ) ) ;
#38542 = CARTESIAN_POINT ( 'NONE',  ( -786.4999999999993179, -494.6608068873671300, -357.6536686473015720 ) ) ;
#38543 = DIRECTION ( 'NONE',  ( -0.000000000000000000, -0.000000000000000000, -1.000000000000000000 ) ) ;
#38544 = CARTESIAN_POINT ( 'NONE',  ( 758.4439275373578084, -252.5545181178799226, 353.2243759319684386 ) ) ;
#38545 = CARTESIAN_POINT ( 'NONE',  ( 797.6776695296629214, -115.5436935675110988, 357.6776695296636603 ) ) ;
#38546 = VERTEX_POINT ( 'NONE', #4571 ) ;
#38547 = CARTESIAN_POINT ( 'NONE',  ( 754.7162404726377645, -14.73633629969885384, -339.4709603349214717 ) ) ;
#38548 = CARTESIAN_POINT ( 'NONE',  ( 801.1904061080338124, -68.08914811296577341, -368.3070685750236066 ) ) ;
#38549 = CARTESIAN_POINT ( 'NONE',  ( 804.1601925771018387, -295.4419599262320730, 346.5483106153029098 ) ) ;
#38550 = CARTESIAN_POINT ( 'NONE',  ( -784.4999999999993179, -544.8427095258973623, -350.0000000000000000 ) ) ;
#38551 = CARTESIAN_POINT ( 'NONE',  ( 745.5313806188320314, -15.28179084515340058, 333.7943932421247268 ) ) ;
#38552 = CARTESIAN_POINT ( 'NONE',  ( 767.7687537140311633, -215.9073299311471317, -372.7932403749916830 ) ) ;
#38553 = CARTESIAN_POINT ( 'NONE',  ( 804.7487373415286811, -163.5436935675109567, 364.7487373415288516 ) ) ;
#38554 = CARTESIAN_POINT ( 'NONE',  ( 762.3223304703356007, -79.54369356751119824, 322.3223304703362828 ) ) ;
#38555 = VECTOR ( 'NONE', #32533, 999.9999999999998863 ) ;
#38556 = CARTESIAN_POINT ( 'NONE',  ( 794.9999999999993179, 239.9999999999998863, -235.0000000000000000 ) ) ;
#38557 = EDGE_CURVE ( 'NONE', #16040, #13477, #32994, .T. ) ;
#38558 = CARTESIAN_POINT ( 'NONE',  ( 758.0141637701419768, -279.0783235625958127, -367.2620300519063790 ) ) ;
#38559 = ADVANCED_FACE ( 'NONE', ( #11742 ), #26022, .T. ) ;
#38560 = CARTESIAN_POINT ( 'NONE',  ( 766.9102291470427417, 5.445481882119263872, 318.6633372737382501 ) ) ;
#38561 = CARTESIAN_POINT ( 'NONE',  ( 751.6929314249748586, -294.9982390220560546, -318.8095938919659034 ) ) ;
#38562 = DIRECTION ( 'NONE',  ( 0.000000000000000000, 0.000000000000000000, -1.000000000000000000 ) ) ;
#38563 = CARTESIAN_POINT ( 'NONE',  ( 764.0069404352550464, -375.0783235625955285, 359.2566176426627180 ) ) ;
#38564 = CARTESIAN_POINT ( 'NONE',  ( 749.2812353651451076, -54.45278447660219001, 323.2262854647983090 ) ) ;
#38565 = CARTESIAN_POINT ( 'NONE',  ( 810.1134526219336749, -32.53286901714208312, -357.8822607201570349 ) ) ;
#38566 = CARTESIAN_POINT ( 'NONE',  ( 802.1676090361156639, -374.6346026584192828, -327.8955696845344505 ) ) ;
#38567 = ADVANCED_FACE ( 'NONE', ( #18662 ), #42909, .F. ) ;
#38568 = CARTESIAN_POINT ( 'NONE',  ( 760.5453621957607311, -21.07832356259667250, 323.8424801807151425 ) ) ;
#38569 = CARTESIAN_POINT ( 'NONE',  ( 761.9338519418445230, -62.53286901714199786, -370.4231160770881957 ) ) ;
#38570 = CARTESIAN_POINT ( 'NONE',  ( 773.3843516231979720, -205.4419599262324425, -364.4086373105754433 ) ) ;
#38571 = CARTESIAN_POINT ( 'NONE',  ( 766.5853460496234675, -205.9874144716870035, 372.3518521366060554 ) ) ;
#38572 = CARTESIAN_POINT ( 'NONE',  ( 757.8323909638828582, -26.63460265842046226, 352.1044303154654358 ) ) ;
#38573 = ORIENTED_EDGE ( 'NONE', *, *, #40559, .T. ) ;
#38574 = CARTESIAN_POINT ( 'NONE',  ( 755.0488828828309806, -209.8055962898687881, -344.1219089521771934 ) ) ;
#38575 = PRODUCT_DEFINITION_CONTEXT ( 'detailed design', #7222, 'design' ) ;
#38576 = CARTESIAN_POINT ( 'NONE',  ( 797.6776695296629214, -187.5436935675108430, 357.6776695296636603 ) ) ;
#38577 = CARTESIAN_POINT ( 'NONE',  ( 793.4146539503750546, -25.98741447168755769, -307.6481478633938877 ) ) ;
#38578 = PRODUCT_RELATED_PRODUCT_CATEGORY ( 'part', '', ( #2245 ) ) ;
#38579 = CARTESIAN_POINT ( 'NONE',  ( 767.8955696845334842, -336.4527844766012663, 362.1676090361161755 ) ) ;
#38580 = CARTESIAN_POINT ( 'NONE',  ( -468.8365100919714337, 260.0000000000001705, -199.9999999999908766 ) ) ;
#38581 = ORIENTED_EDGE ( 'NONE', *, *, #22188, .F. ) ;
#38582 = CARTESIAN_POINT ( 'NONE',  ( 758.6633372737375112, -44.53286901714205470, 326.9102291470432533 ) ) ;
#38583 = CARTESIAN_POINT ( 'NONE',  ( 809.0717654672305343, -316.9181544815160692, -360.1688906516309885 ) ) ;
#38584 = CARTESIAN_POINT ( 'NONE',  ( 792.2312462859673587, -251.9073299311470748, 307.2067596250082602 ) ) ;
#38585 = CARTESIAN_POINT ( 'NONE',  ( 755.5913626894240451, -325.6454272087888739, 346.6156483768012890 ) ) ;
#38586 = CARTESIAN_POINT ( 'NONE',  ( 802.7791456095903868, -436.7146871989589272, 329.0155153010375102 ) ) ;
#38587 = CARTESIAN_POINT ( 'NONE',  ( 787.5531968255692163, -141.8272453906075157, -316.1348686366205811 ) ) ;
#38588 = CARTESIAN_POINT ( 'NONE',  ( 791.9812246680005501, -140.6346026584201070, -361.9419747391813189 ) ) ;
#38589 = AXIS2_PLACEMENT_3D ( 'NONE', #25307, #43757, #32482 ) ;
#38590 = CARTESIAN_POINT ( 'NONE',  ( 764.8639956371174549, -344.0891481129648355, -319.7806653035542581 ) ) ;
#38591 = ORIENTED_EDGE ( 'NONE', *, *, #16520, .T. ) ;
#38592 = CARTESIAN_POINT ( 'NONE',  ( 787.5162901302840055, -299.3618753856922581, 305.4481719005792684 ) ) ;
#38593 = CARTESIAN_POINT ( 'NONE',  ( 754.8983024940795303, -330.8965053807774552, 336.9254006560228163 ) ) ;
#38594 = CARTESIAN_POINT ( 'NONE',  ( -39.63011601220123481, -512.9681489794448908, -350.0000000000000000 ) ) ;
#38595 = CARTESIAN_POINT ( 'NONE',  ( 793.9708237608222134, -118.9181544815167229, 319.2295555964448681 ) ) ;
#38596 = CARTESIAN_POINT ( 'NONE',  ( 762.1405469898971887, -1.543693567511449150, 357.8594530101015607 ) ) ;
#38597 = VERTEX_POINT ( 'NONE', #2170 ) ;
#38598 = CARTESIAN_POINT ( 'NONE',  ( 781.2370466360911223, -380.7363362996977116, -304.9990715423533629 ) ) ;
#38599 = CARTESIAN_POINT ( 'NONE',  ( -598.8365100919716042, 256.5000000000001705, -206.1189999999899385 ) ) ;
#38600 = CARTESIAN_POINT ( 'NONE',  ( 772.4468031744293057, -225.8272453906072599, 363.8651313633793620 ) ) ;
#38601 = CARTESIAN_POINT ( 'NONE',  ( 802.2119215644370342, -246.0090635724253900, 367.5423716828165084 ) ) ;
#38602 = CARTESIAN_POINT ( 'NONE',  ( 780.5290396650775619, -180.3510508353234343, 365.2837595273619513 ) ) ;
#38603 = CARTESIAN_POINT ( 'NONE',  ( 765.0180583372156207, -336.9982390220558273, -360.0135310231089534 ) ) ;
#38604 = CIRCLE ( 'NONE', #8375, 7.999999999999785061 ) ;
#38605 = CARTESIAN_POINT ( 'NONE',  ( 911.9749999999993406, 219.9999999999998863, 339.9999999999999432 ) ) ;
#38606 = CARTESIAN_POINT ( 'NONE',  ( 760.7433823573367135, -228.0090635724254753, -355.9930595647440441 ) ) ;
#38607 = CARTESIAN_POINT ( 'NONE',  ( 744.7301800767019131, -28.81642084023863148, 337.4774526936615757 ) ) ;
#38608 = CARTESIAN_POINT ( 'NONE',  ( 792.3570229623688874, -69.18005720387488111, 373.1304606946836202 ) ) ;
#38609 = CARTESIAN_POINT ( 'NONE',  ( -468.8365100919714337, 260.0000000000001705, -206.1189999999908764 ) ) ;
#38610 = CARTESIAN_POINT ( 'NONE',  ( 782.5225473063383106, -406.2709662947828519, -375.2698199232970637 ) ) ;
#38611 = CARTESIAN_POINT ( 'NONE',  ( -208.8365100919714052, 240.0000000000000853, -199.9999999999926956 ) ) ;
#38612 = CARTESIAN_POINT ( 'NONE',  ( 749.5768839229115201, -348.5545181178796383, 358.0661480581553064 ) ) ;
#38613 = CARTESIAN_POINT ( 'NONE',  ( 775.4999999999993179, -544.8427095258973623, -369.9999999999999432 ) ) ;
#38614 = CARTESIAN_POINT ( 'NONE',  ( 772.4837098697144029, -311.3618753856922581, 374.5518280994205611 ) ) ;
#38615 = CARTESIAN_POINT ( 'NONE',  ( 746.8695393053150156, -53.90732993114765037, -327.6429770376306010 ) ) ;
#38616 = CARTESIAN_POINT ( 'NONE',  ( 774.6312213355099630, -287.3618753856923718, -364.6798772138717482 ) ) ;
#38617 = PLANE ( 'NONE',  #40954 ) ;
#38618 = CARTESIAN_POINT ( 'NONE',  ( 791.9812246680005501, -380.6346026584192828, 361.9419747391813189 ) ) ;
#38619 = VECTOR ( 'NONE', #14822, 1000.000000000000000 ) ;
#38620 = CARTESIAN_POINT ( 'NONE',  ( 776.9254006560222479, -164.1908817542438612, 314.8983024940802125 ) ) ;
#38621 = CARTESIAN_POINT ( 'NONE',  ( 754.3581564841646241, -41.46360902697149697, -316.1443688327762516 ) ) ;
#38622 = CARTESIAN_POINT ( 'NONE',  ( 802.7791456095903868, -100.7146871989600356, -329.0155153010375102 ) ) ;
#38623 = CARTESIAN_POINT ( 'NONE',  ( 786.2056067578752163, -59.80559628986927834, 374.4686193811670023 ) ) ;
#38624 = CARTESIAN_POINT ( 'NONE',  ( 759.7806653035535192, -414.9982390220555430, 324.8639956371181370 ) ) ;
#38625 = AXIS2_PLACEMENT_3D ( 'NONE', #30933, #40867, #23521 ) ;
#38626 = CARTESIAN_POINT ( 'NONE',  ( 811.0346526505617248, 9.365397341579424051, 323.0537975583478101 ) ) ;
#38627 = CARTESIAN_POINT ( 'NONE',  ( 927.9999999999992042, 219.9999999999998863, 360.0000000000000000 ) ) ;
#38628 = CARTESIAN_POINT ( 'NONE',  ( 791.1614460488616487, -155.2601417444144261, 373.5763878283158874 ) ) ;
#38629 = FACE_OUTER_BOUND ( 'NONE', #19532, .T. ) ;
#38631 = ORIENTED_EDGE ( 'NONE', *, *, #38265, .T. ) ;
#38630 = CARTESIAN_POINT ( 'NONE',  ( 789.9200121543843807, -97.98741447168734453, -317.0176451133914384 ) ) ;
#38632 = CARTESIAN_POINT ( 'NONE',  ( 803.4237431249931660, -63.18005720387488822, -331.2633955100225194 ) ) ;
#38633 = CARTESIAN_POINT ( 'NONE',  ( 803.2186876482843445, -391.9874144716864066, -350.0220218866286928 ) ) ;
#38635 = CARTESIAN_POINT ( 'NONE',  ( 764.8639956371174549, -224.0891481129652902, 319.7806653035542581 ) ) ;
#38634 = CARTESIAN_POINT ( 'NONE',  ( 781.8018195045266339, -238.2709662947833920, 365.1927285166406705 ) ) ;
#38636 = ORIENTED_EDGE ( 'NONE', *, *, #44758, .F. ) ;
#38637 = CARTESIAN_POINT ( 'NONE',  ( 778.7502325331095108, -384.3510508353227806, -304.6391490659818828 ) ) ;
#38638 = CARTESIAN_POINT ( 'NONE',  ( 807.5423716828161105, -441.0783235625953580, 362.2119215644372048 ) ) ;
#38639 = CARTESIAN_POINT ( 'NONE',  ( -180.7583438952258348, 394.6698570112193920, -274.9999999999999432 ) ) ;
#38640 = ORIENTED_EDGE ( 'NONE', *, *, #13433, .F. ) ;
#38641 = CARTESIAN_POINT ( 'NONE',  ( 778.1981804954714335, -442.2709662947826814, 314.8072714833589885 ) ) ;
#38642 = AXIS2_PLACEMENT_3D ( 'NONE', #38212, #30580, #45137 ) ;
#38643 = VERTEX_POINT ( 'NONE', #32752 ) ;
#38644 = VERTEX_POINT ( 'NONE', #40132 ) ;
#38645 = CARTESIAN_POINT ( 'NONE',  ( 755.2512626584698410, -247.5436935675106724, -315.2512626584710915 ) ) ;
#38646 = CARTESIAN_POINT ( 'NONE',  ( 808.0189434323515343, -158.0891481129655176, 319.0252816721025511 ) ) ;
#38647 = ORIENTED_EDGE ( 'NONE', *, *, #24398, .T. ) ;
#38648 = CARTESIAN_POINT ( 'NONE',  ( 802.1676090361155502, -230.6346026584197944, -327.8955696845344505 ) ) ;
#38649 = ORIENTED_EDGE ( 'NONE', *, *, #18500, .T. ) ;
#38650 = CARTESIAN_POINT ( 'NONE',  ( 795.1360043628807261, -356.0891481129647218, -360.2193346964456282 ) ) ;
#38651 = CARTESIAN_POINT ( 'NONE',  ( 785.3141322388236176, 2.274488250670355871, -364.4286716492789537 ) ) ;
#38652 = CARTESIAN_POINT ( 'NONE',  ( 796.7845633553578182, -225.6237781080506011, 358.5707757039688204 ) ) ;
#38653 = CARTESIAN_POINT ( 'NONE',  ( -769.9999999999992042, 240.0000000000000568, -319.9999999999999432 ) ) ;
#38654 = CYLINDRICAL_SURFACE ( 'NONE', #38341, 8.024999999999948841 ) ;
#38655 = ORIENTED_EDGE ( 'NONE', *, *, #8842, .F. ) ;
#38656 = CARTESIAN_POINT ( 'NONE',  ( 804.6798772138708955, -15.72551174932958951, -334.6312213355107019 ) ) ;
#38657 = LINE ( 'NONE', #34952, #32897 ) ;
#38658 = CYLINDRICAL_SURFACE ( 'NONE', #1203, 19.99999999999990763 ) ;
#38659 = AXIS2_PLACEMENT_3D ( 'NONE', #31278, #30595, #13283 ) ;
#38660 = ORIENTED_EDGE ( 'NONE', *, *, #12031, .F. ) ;
#38661 = CARTESIAN_POINT ( 'NONE',  ( 814.2805881961230625, -265.6454272087889876, -331.2368401574024119 ) ) ;
#38662 = AXIS2_PLACEMENT_3D ( 'NONE', #2412, #5414, #40999 ) ;
#38663 = CARTESIAN_POINT ( 'NONE',  ( 768.9521613784389729, -129.8272453906075725, 373.2346286133773106 ) ) ;
#38665 = CARTESIAN_POINT ( 'NONE',  ( 781.8018195045266339, -238.2709662947833920, -365.1927285166406705 ) ) ;
#38664 = CARTESIAN_POINT ( 'NONE',  ( 831.1634899080286232, 258.0939999999998804, -193.8809999999999718 ) ) ;
#38666 = CARTESIAN_POINT ( 'NONE',  ( 780.5290396650775619, -396.3510508353228374, -365.2837595273619513 ) ) ;
#38667 = FACE_BOUND ( 'NONE', #10596, .T. ) ;
#38668 = DIRECTION ( 'NONE',  ( 8.326672684688676025E-16, 1.000000000000000000, 0.000000000000000000 ) ) ;
#38669 = CARTESIAN_POINT ( 'NONE',  ( 766.0291762391763086, -130.9181544815166660, -360.7704444035551319 ) ) ;
#38670 = CARTESIAN_POINT ( 'NONE',  ( 773.7305795820266212, -393.2817908451522726, 374.8230680027170365 ) ) ;
#38671 = LINE ( 'NONE', #10039, #2657 ) ;
#38672 = CARTESIAN_POINT ( 'NONE',  ( 773.7943932421234194, 24.19440371013046231, -305.5313806188329409 ) ) ;
#38673 = CARTESIAN_POINT ( 'NONE',  ( 772.5602148656447525, -321.7255117493286320, -305.7998596910095443 ) ) ;
#38674 = DIRECTION ( 'NONE',  ( 0.000000000000000000, -0.7651688349527138167, 0.6438296778008192334 ) ) ;
#38675 = DIRECTION ( 'NONE',  ( 0.000000000000000000, 1.000000000000000000, -0.000000000000000000 ) ) ;
#38676 = CARTESIAN_POINT ( 'NONE',  ( 778.2165204200184689, -94.81642084023843609, -364.9363028652563230 ) ) ;
#38677 = VECTOR ( 'NONE', #11767, 1000.000000000000000 ) ;
#38678 = CARTESIAN_POINT ( 'NONE',  ( 814.4686193811664907, -243.2817908451526705, 346.2056067578752732 ) ) ;
#38679 = CARTESIAN_POINT ( 'NONE',  ( 801.9858362298568863, -219.0783235625960401, -312.7379699480935642 ) ) ;
#38680 = CARTESIAN_POINT ( 'NONE',  ( 749.2812353651451076, -198.4527844766017495, 323.2262854647983090 ) ) ;
#38681 = CARTESIAN_POINT ( 'NONE',  ( 749.2812353651451076, -438.4527844766009821, -323.2262854647983090 ) ) ;
#38682 = DIRECTION ( 'NONE',  ( 0.000000000000000000, 0.000000000000000000, -1.000000000000000000 ) ) ;
#38683 = VECTOR ( 'NONE', #2888, 1000.000000000000000 ) ;
#38684 = CARTESIAN_POINT ( 'NONE',  ( 804.4286716492782716, -305.3618753856922581, 345.3141322388244703 ) ) ;
#38685 = EDGE_CURVE ( 'NONE', #33479, #2741, #1332, .T. ) ;
#38686 = CARTESIAN_POINT ( 'NONE',  ( 780.5236548040995785, -92.73633629969860692, 314.9735926884559944 ) ) ;
#38687 = CARTESIAN_POINT ( 'NONE',  ( 783.0433043558608688, 23.10349461922137237, -315.1538015810313027 ) ) ;
#38688 = LINE ( 'NONE', #38453, #20297 ) ;
#38689 = DIRECTION ( 'NONE',  ( 0.000000000000000000, -0.7651688349527138167, 0.6438296778008192334 ) ) ;
#38691 = CARTESIAN_POINT ( 'NONE',  ( 804.9363028652555840, -328.2709662947831362, 338.2165204200192079 ) ) ;
#38690 = CARTESIAN_POINT ( 'NONE',  ( 793.2243759319678702, -122.5328690171417918, 318.4439275373583200 ) ) ;
#38692 = ORIENTED_EDGE ( 'NONE', *, *, #15287, .F. ) ;
#38693 = VECTOR ( 'NONE', #25238, 1000.000000000000000 ) ;
#38694 = CARTESIAN_POINT ( 'NONE',  ( 756.7813123517142913, -259.9874144716869182, -329.9779781133712504 ) ) ;
#38695 = CARTESIAN_POINT ( 'NONE',  ( 781.8018195045266339, -94.27096629478386092, 365.1927285166406705 ) ) ;
#38696 = CARTESIAN_POINT ( 'NONE',  ( 776.2433038121456548, -300.8965053807775689, -374.8207195650711014 ) ) ;
#38697 = DIRECTION ( 'NONE',  ( 0.000000000000000000, -0.3826834323650836756, -0.9238795325112892920 ) ) ;
#38698 = CARTESIAN_POINT ( 'NONE',  ( 745.1769319972822814, -401.8055962898681059, 346.2694204179732083 ) ) ;
#38699 = EDGE_LOOP ( 'NONE', ( #32679, #25860, #12660, #3659 ) ) ;
#38700 = CARTESIAN_POINT ( 'NONE',  ( 791.9812246680005501, -284.6346026584196807, 361.9419747391813189 ) ) ;
#38701 = CARTESIAN_POINT ( 'NONE',  ( 755.0488828828309806, -41.80559628986934229, -344.1219089521771934 ) ) ;
#38702 = CARTESIAN_POINT ( 'NONE',  ( 764.8639956371174549, -176.0891481129653755, -319.7806653035542013 ) ) ;
#38703 = CARTESIAN_POINT ( 'NONE',  ( 794.9819416627830151, -204.9982390220562820, -319.9864689768909898 ) ) ;
#38704 = CARTESIAN_POINT ( 'NONE',  ( 762.3223304703356007, -391.5436935675101608, 322.3223304703362828 ) ) ;
#38705 = CARTESIAN_POINT ( 'NONE',  ( 808.0189434323515343, -158.0891481129655176, -319.0252816721025511 ) ) ;
#38706 = CARTESIAN_POINT ( 'NONE',  ( 768.0187753319979720, -104.6346026584202207, -318.0580252608186242 ) ) ;
#38707 = ORIENTED_EDGE ( 'NONE', *, *, #33498, .T. ) ;
#38708 = CARTESIAN_POINT ( 'NONE',  ( 755.1538015810308480, -374.1908817542432075, -343.0433043558613804 ) ) ;
#38709 = VECTOR ( 'NONE', #30428, 1000.000000000000000 ) ;
#38711 = CARTESIAN_POINT ( 'NONE',  ( 754.7162404726377645, -446.7363362996975980, 339.4709603349214717 ) ) ;
#38710 = CARTESIAN_POINT ( 'NONE',  ( 756.5762568750052424, -123.1800572038747106, 348.7366044899774238 ) ) ;
#38712 = CARTESIAN_POINT ( 'NONE',  ( 784.0799538623451781, -131.8055962898690439, 364.6971507214555572 ) ) ;
#38715 = CARTESIAN_POINT ( 'NONE',  ( 813.9316612368132837, -391.4419599262317888, 348.6739635108323228 ) ) ;
#38714 = CARTESIAN_POINT ( 'NONE',  ( 571.1634899080285095, 259.9999999999999432, -197.2499999999982947 ) ) ;
#38713 = DIRECTION ( 'NONE',  ( 0.000000000000000000, 0.000000000000000000, 1.000000000000000000 ) ) ;
#38716 = VECTOR ( 'NONE', #26461, 1000.000000000000000 ) ;
#38717 = ORIENTED_EDGE ( 'NONE', *, *, #11041, .T. ) ;
#38718 = CARTESIAN_POINT ( 'NONE',  ( 796.1575198192839480, -366.0090635724250774, -359.4546378042384163 ) ) ;
#38719 = CARTESIAN_POINT ( 'NONE',  ( 764.8639956371174549, -368.0891481129647786, -319.7806653035542013 ) ) ;
#38720 = CARTESIAN_POINT ( 'NONE',  ( 786.2694204179717872, -165.2817908451529547, -305.1769319972829067 ) ) ;
#38721 = CARTESIAN_POINT ( 'NONE',  ( 814.2805881961230625, -49.64542720878965554, 331.2368401574024119 ) ) ;
#38723 = CYLINDRICAL_SURFACE ( 'NONE', #21049, 7.999999999999896083 ) ;
#38722 = DIRECTION ( 'NONE',  ( -0.000000000000000000, 1.000000000000000000, -0.000000000000000000 ) ) ;
#38724 = CARTESIAN_POINT ( 'NONE',  ( 780.5290396650775619, -300.3510508353230080, -365.2837595273619513 ) ) ;
#38725 = DIRECTION ( 'NONE',  ( -1.000000000000000000, -0.000000000000000000, -0.000000000000000000 ) ) ;
#38726 = CARTESIAN_POINT ( 'NONE',  ( 807.2620300519052989, -168.0090635724256458, -318.0141637701419768 ) ) ;
#38727 = DIRECTION ( 'NONE',  ( 1.000000000000000000, 0.000000000000000000, 0.000000000000000000 ) ) ;
#38728 = DIRECTION ( 'NONE',  ( 0.000000000000000000, 0.000000000000000000, 1.000000000000000000 ) ) ;
#38729 = CARTESIAN_POINT ( 'NONE',  ( 796.1575198192839480, -366.0090635724250774, 359.4546378042384163 ) ) ;
#38730 = CLOSED_SHELL ( 'NONE', ( #32894, #33738, #3550, #26305, #4169, #34654, #42769, #10019, #6065, #23504, #21622, #34601, #44733, #15446, #22501, #28053, #9698, #34239, #5518, #7393, #4398, #38559, #44784, #19850 ) ) ;
#38731 = CARTESIAN_POINT ( 'NONE',  ( 745.1792804349281596, -326.1908817542433781, 343.7566961878542884 ) ) ;
#38732 = VECTOR ( 'NONE', #31398, 1000.000000000000000 ) ;
#38733 = CARTESIAN_POINT ( 'NONE',  ( 772.5602148656447525, -201.7255117493290015, -305.7998596910095443 ) ) ;
#38734 = ADVANCED_FACE ( 'NONE', ( #37510 ), #8828, .F. ) ;
#38735 = DIRECTION ( 'NONE',  ( 0.000000000000000000, 0.000000000000000000, 1.000000000000000000 ) ) ;
#38736 = DIRECTION ( 'NONE',  ( -0.000000000000000000, 1.000000000000000000, -0.000000000000000000 ) ) ;
#38737 = AXIS2_PLACEMENT_3D ( 'NONE', #38164, #34211, #20366 ) ;
#38738 = CARTESIAN_POINT ( 'NONE',  ( 815.3608509340175488, -146.7363362996984506, 341.2497674668889545 ) ) ;
#38739 = CARTESIAN_POINT ( 'NONE',  ( 815.0009284576459549, -102.3510508353236901, -338.7629533639073429 ) ) ;
#38740 = CARTESIAN_POINT ( 'NONE',  ( 815.2698199232961542, -328.8164208402375834, -342.5225473063383106 ) ) ;
#38741 = ADVANCED_FACE ( 'NONE', ( #37275 ), #8054, .F. ) ;
#38742 = CYLINDRICAL_SURFACE ( 'NONE', #19342, 10.00000000000000888 ) ;
#38743 = CARTESIAN_POINT ( 'NONE',  ( 989.9999999999992042, -590.0000000000001137, -360.0000000000000000 ) ) ;
#38744 = CARTESIAN_POINT ( 'NONE',  ( 800.0135310231082713, -182.0891481129654323, 325.0180583372163028 ) ) ;
#38745 = DIRECTION ( 'NONE',  ( 0.000000000000000000, 1.000000000000000000, 0.000000000000000000 ) ) ;
#38746 = CIRCLE ( 'NONE', #36517, 10.00000000000000888 ) ;
#38747 = CARTESIAN_POINT ( 'NONE',  ( 745.7194118038753459, -445.6454272087883055, 348.7631598425976449 ) ) ;
#38748 = CARTESIAN_POINT ( 'NONE',  ( 786.2056067578752163, -371.8055962898682765, -374.4686193811670023 ) ) ;
#38749 = CARTESIAN_POINT ( 'NONE',  ( 772.4837098697144029, -143.3618753856927697, -374.5518280994205611 ) ) ;
#38750 = VECTOR ( 'NONE', #16527, 1000.000000000000000 ) ;
#38751 = CARTESIAN_POINT ( 'NONE',  ( 748.9653473494363425, -410.6346026584191122, -356.9462024416521331 ) ) ;
#38752 = DIRECTION ( 'NONE',  ( 8.659560562354807133E-17, 0.7071067811865578978, -0.7071067811865372477 ) ) ;
#38753 = CARTESIAN_POINT ( 'NONE',  ( 786.2056067578752163, -11.80559628986942577, 374.4686193811670023 ) ) ;
#38754 = ORIENTED_EDGE ( 'NONE', *, *, #13551, .F. ) ;
#38755 = VECTOR ( 'NONE', #3505, 1000.000000000000000 ) ;
#38756 = CARTESIAN_POINT ( 'NONE',  ( 761.9338519418445230, -182.5328690171416497, -370.4231160770881957 ) ) ;
#38757 = CARTESIAN_POINT ( 'NONE',  ( 919.9999999999993179, 219.9999999999998863, -350.0000000000000000 ) ) ;
#38758 = CARTESIAN_POINT ( 'NONE',  ( 786.2056067578752163, -299.8055962898685038, 374.4686193811670023 ) ) ;
#38759 = CARTESIAN_POINT ( 'NONE',  ( 757.8323909638828582, -122.6346026584201496, 352.1044303154654358 ) ) ;
#38760 = ORIENTED_EDGE ( 'NONE', *, *, #25747, .T. ) ;
#38761 = CARTESIAN_POINT ( 'NONE',  ( 767.8955696845333705, -312.4527844766012663, 362.1676090361162323 ) ) ;
#38762 = CARTESIAN_POINT ( 'NONE',  ( 808.3070685750230950, 5.001760977943074948, -361.1904061080339261 ) ) ;
#38763 = CARTESIAN_POINT ( 'NONE',  ( 793.3938497862117174, -453.0432664090020580, 372.3358127763067955 ) ) ;
#38764 = ORIENTED_EDGE ( 'NONE', *, *, #15112, .T. ) ;
#38765 = CARTESIAN_POINT ( 'NONE',  ( 776.2046728542105711, -428.1908817542430938, -304.8212110874238761 ) ) ;
#38766 = AXIS2_PLACEMENT_3D ( 'NONE', #12626, #26704, #23232 ) ;
#38767 = ORIENTED_EDGE ( 'NONE', *, *, #18268, .T. ) ;
#38768 = APPLICATION_PROTOCOL_DEFINITION ( 'draft international standard', 'automotive_design', 1998, #21377 ) ;
#38769 = CARTESIAN_POINT ( 'NONE',  ( 785.3687786644884454, -11.36187538569323863, 315.3201227861279676 ) ) ;
#38770 = CARTESIAN_POINT ( 'NONE',  ( 756.3353852180819104, -245.9073299311469896, -331.1735550268788302 ) ) ;
#38772 = CARTESIAN_POINT ( 'NONE',  ( 756.1443688327750579, -285.6237781080502600, 314.3581564841659315 ) ) ;
#38771 = CARTESIAN_POINT ( 'NONE',  ( 772.4837098697145166, -359.3618753856921444, 374.5518280994205611 ) ) ;
#38773 = CARTESIAN_POINT ( 'NONE',  ( 754.0944755984390895, -63.62377810805107714, 364.1009440267246760 ) ) ;
#38774 = CARTESIAN_POINT ( 'NONE',  ( 802.5472867521000353, -244.3726999360617924, -350.8726784830461156 ) ) ;
#38775 = CARTESIAN_POINT ( 'NONE',  ( 801.9419747391806368, -258.4527844766016074, -351.9812246680014027 ) ) ;
#38776 = DIRECTION ( 'NONE',  ( 0.000000000000000000, -1.000000000000000000, 0.000000000000000000 ) ) ;
#38777 = CARTESIAN_POINT ( 'NONE',  ( 800.2193346964447755, -114.9982390220565236, -355.1360043628815788 ) ) ;
#38778 = CARTESIAN_POINT ( 'NONE',  ( 800.2193346964447755, -258.9982390220561115, 355.1360043628815788 ) ) ;
#38779 = CARTESIAN_POINT ( 'NONE',  ( 772.5602148656447525, -393.7255117493283478, 305.7998596910095443 ) ) ;
#38780 = AXIS2_PLACEMENT_3D ( 'NONE', #43406, #6987, #32557 ) ;
#38782 = PLANE ( 'NONE',  #13778 ) ;
#38781 = LINE ( 'NONE', #197, #31448 ) ;
#38783 = CARTESIAN_POINT ( 'NONE',  ( 783.7953271457878373, -56.19088175424417386, -375.1787889125761239 ) ) ;
#38784 = DIRECTION ( 'NONE',  ( -0.000000000000000000, 1.000000000000000000, -0.000000000000000000 ) ) ;
#38785 = DIRECTION ( 'NONE',  ( 0.000000000000000000, -1.000000000000000000, 0.000000000000000000 ) ) ;
#38786 = AXIS2_PLACEMENT_3D ( 'NONE', #26866, #40975, #22277 ) ;
#38787 = ADVANCED_FACE ( 'NONE', ( #30340 ), #44432, .F. ) ;
#38788 = CARTESIAN_POINT ( 'NONE',  ( 757.4527132478984868, -256.3726999360617924, 329.1273215169538844 ) ) ;
#38789 = APPLICATION_CONTEXT ( 'automotive_design' ) ;
#38790 = CARTESIAN_POINT ( 'NONE',  ( 802.1676090361156639, -110.6346026584201638, 327.8955696845344505 ) ) ;
#38791 = ORIENTED_EDGE ( 'NONE', *, *, #14169, .T. ) ;
#38792 = CARTESIAN_POINT ( 'NONE',  ( 793.9708237608222134, 1.081845518482914104, -319.2295555964448681 ) ) ;
#38793 = CARTESIAN_POINT ( 'NONE',  ( 808.3070685750232087, -90.99823902205662307, -361.1904061080339829 ) ) ;
#38794 = CARTESIAN_POINT ( 'NONE',  ( 787.6308680596127942, -275.2601417444140566, 364.1105419155492768 ) ) ;
#38795 = PLANE ( 'NONE',  #1982 ) ;
#38796 = CARTESIAN_POINT ( 'NONE',  ( 793.5525998758768083, -31.09997266333516919, 372.6845335610516941 ) ) ;
#38797 = CARTESIAN_POINT ( 'NONE',  ( 759.0252816721024374, -240.9982390220561683, -368.0189434323527280 ) ) ;
#38798 = EDGE_CURVE ( 'NONE', #757, #30488, #20177, .T. ) ;
#38799 = CARTESIAN_POINT ( 'NONE',  ( 810.7187646348534145, -162.4527844766018632, 356.7737145352016341 ) ) ;
#38800 = CARTESIAN_POINT ( 'NONE',  ( 767.8955696845333705, -96.45278447660203369, 362.1676090361162323 ) ) ;
#38801 = AXIS2_PLACEMENT_3D ( 'NONE', #17869, #24324, #18104 ) ;
#38802 =( LENGTH_UNIT ( ) NAMED_UNIT ( * ) SI_UNIT ( .MILLI., .METRE. ) );
#38803 = CARTESIAN_POINT ( 'NONE',  ( 746.7653713866222915, -281.2601417444139997, -351.0478386215610271 ) ) ;
#38804 = AXIS2_PLACEMENT_3D ( 'NONE', #3560, #35403, #3774 ) ;
#38805 = CARTESIAN_POINT ( 'NONE',  ( 810.4231160770870019, -456.5545181178792404, 321.9338519418446936 ) ) ;
#38806 = CARTESIAN_POINT ( 'NONE',  ( 814.5518280994195948, -303.7255117493287457, -332.4837098697145734 ) ) ;
#38807 = CARTESIAN_POINT ( 'NONE',  ( 989.9999999999992042, 249.9999999999998863, -360.0000000000000000 ) ) ;
#38808 = CARTESIAN_POINT ( 'NONE',  ( 798.7617431975189675, -363.6237781080502032, 323.0428371773161871 ) ) ;
#38809 = CARTESIAN_POINT ( 'NONE',  ( 801.1904061080338124, -44.08914811296585157, 368.3070685750236066 ) ) ;
#38811 = VECTOR ( 'NONE', #5873, 1000.000000000000000 ) ;
#38810 = CARTESIAN_POINT ( 'NONE',  ( 756.3353852180819104, -389.9073299311465348, -331.1735550268788302 ) ) ;
#38812 = CARTESIAN_POINT ( 'NONE',  ( 769.1273215169530886, -46.71468719896022748, 317.4527132478988847 ) ) ;
#38813 = CARTESIAN_POINT ( 'NONE',  ( 744.8212110874229666, -90.89650538077827946, -336.2046728542121627 ) ) ;
#38814 = EDGE_CURVE ( 'NONE', #13375, #3205, #40551, .T. ) ;
#38815 = CARTESIAN_POINT ( 'NONE',  ( 778.7502325331095108, -216.3510508353233490, 304.6391490659818828 ) ) ;
#38816 = CARTESIAN_POINT ( 'NONE',  ( 765.0180583372156207, -24.99823902205683268, 360.0135310231089534 ) ) ;
#38817 =( GEOMETRIC_REPRESENTATION_CONTEXT ( 3 ) GLOBAL_UNCERTAINTY_ASSIGNED_CONTEXT ( ( #5166 ) ) GLOBAL_UNIT_ASSIGNED_CONTEXT ( ( #31589, #35274, #45217 ) ) REPRESENTATION_CONTEXT ( 'NONE', 'WORKASPACE' ) );
#38818 = EDGE_CURVE ( 'NONE', #27240, #18651, #27561, .T. ) ;
#38819 = ORIENTED_EDGE ( 'NONE', *, *, #28972, .T. ) ;
#38820 = CARTESIAN_POINT ( 'NONE',  ( 800.0135310231082713, -86.08914811296573077, -325.0180583372163028 ) ) ;
#38821 = CARTESIAN_POINT ( 'NONE',  ( 759.2295555964440155, -208.1692326535051905, -353.9708237608231229 ) ) ;
#38822 = CARTESIAN_POINT ( 'NONE',  ( 767.8955696845333705, -192.4527844766016926, 362.1676090361162323 ) ) ;
#38823 = AXIS2_PLACEMENT_3D ( 'NONE', #18388, #38959, #7309 ) ;
#38824 = PRODUCT ( 'Lower Fixed Bed Shear Blade', 'Lower Fixed Bed Shear Blade', '', ( #18215 ) ) ;
#38825 = CARTESIAN_POINT ( 'NONE',  ( 778.7502325331095108, -48.35105083532386061, -304.6391490659818828 ) ) ;
#38826 = CARTESIAN_POINT ( 'NONE',  ( 785.3141322388236176, -333.7255117493286320, 364.4286716492789537 ) ) ;
#38827 = ADVANCED_FACE ( 'NONE', ( #37737 ), #20851, .F. ) ;
#38828 = CARTESIAN_POINT ( 'NONE',  ( 759.2380499001254748, 21.41625977839825978, 318.3449445151863415 ) ) ;
#38829 = VERTEX_POINT ( 'NONE', #31031 ) ;
#38830 = CARTESIAN_POINT ( 'NONE',  ( 754.8983024940795303, -42.89650538077842157, 336.9254006560228163 ) ) ;
#38831 = CARTESIAN_POINT ( 'NONE',  ( 797.8822607201568644, -294.5545181178797520, -370.1134526219340160 ) ) ;
#38832 = CARTESIAN_POINT ( 'NONE',  ( 751.9810565676468741, -242.0891481129652618, 360.9747183278973921 ) ) ;
#38833 = CARTESIAN_POINT ( 'NONE',  ( 805.9055244015594326, -3.623778108051270319, 315.8990559732753240 ) ) ;
#38834 = CARTESIAN_POINT ( 'NONE',  ( 755.1538015810308480, -134.1908817542439181, -343.0433043558613804 ) ) ;
#38835 = CARTESIAN_POINT ( 'NONE',  ( 804.4286716492782716, -161.3618753856927697, -345.3141322388244703 ) ) ;
#38836 = CARTESIAN_POINT ( 'NONE',  ( 774.6312213355098493, -335.3618753856921444, -364.6798772138717482 ) ) ;
#38837 = EDGE_LOOP ( 'NONE', ( #42798, #7523, #44070, #1251 ) ) ;
#38838 = CARTESIAN_POINT ( 'NONE',  ( 803.6646147819161570, -449.9073299311463643, -348.8264449731210561 ) ) ;
#38839 = CARTESIAN_POINT ( 'NONE',  ( 772.5602148656447525, -297.7255117493286889, 305.7998596910095443 ) ) ;
#38840 = EDGE_CURVE ( 'NONE', #9771, #38829, #17678, .T. ) ;
#38841 = LINE ( 'NONE', #9566, #42501 ) ;
#38842 = CARTESIAN_POINT ( 'NONE',  ( 787.6308680596127942, -323.2601417444138860, 364.1105419155492768 ) ) ;
#38843 = DIRECTION ( 'NONE',  ( -1.000000000000000000, 1.880165489482579047E-16, 0.000000000000000000 ) ) ;
#38844 = EDGE_CURVE ( 'NONE', #5059, #36366, #31260, .T. ) ;
#38845 = CARTESIAN_POINT ( 'NONE',  ( 766.0291762391763086, -154.9181544815165523, 360.7704444035551319 ) ) ;
#38846 = CARTESIAN_POINT ( 'NONE',  ( 756.3353852180819104, -5.907329931147798696, 331.1735550268788302 ) ) ;
#38847 = ORIENTED_EDGE ( 'NONE', *, *, #37644, .T. ) ;
#38848 = CARTESIAN_POINT ( 'NONE',  ( 788.6739635108323228, -391.6454272087885897, -373.9316612368139090 ) ) ;
#38849 = CARTESIAN_POINT ( 'NONE',  ( 800.9747183278959710, 11.00176097794305541, -311.9810565676471583 ) ) ;
#38850 = CARTESIAN_POINT ( 'NONE',  ( 790.0220218866281812, -223.0999726633346256, 363.2186876482849129 ) ) ;
#38851 = CARTESIAN_POINT ( 'NONE',  ( 749.5768839229115201, -252.5545181178799226, 358.0661480581553064 ) ) ;
#38852 = CARTESIAN_POINT ( 'NONE',  ( 790.8726784830453198, -178.7146871989598083, 362.5472867521010585 ) ) ;
#38853 = CARTESIAN_POINT ( 'NONE',  ( 802.1676090361156639, -350.6346026584192828, -327.8955696845344505 ) ) ;
#38854 = CARTESIAN_POINT ( 'NONE',  ( 803.6646147819161570, 6.092670068852159559, 348.8264449731210561 ) ) ;
#38855 = SURFACE_STYLE_USAGE ( .BOTH. , #29367 ) ;
#38856 = CARTESIAN_POINT ( 'NONE',  ( 761.4292242960306112, -233.4636090269708575, -323.2154366446414429 ) ) ;
#38857 = ADVANCED_FACE ( 'NONE', ( #10241 ), #41273, .F. ) ;
#38858 = CARTESIAN_POINT ( 'NONE',  ( 808.0189434323515343, -14.08914811296595460, 319.0252816721025511 ) ) ;
#38859 = CARTESIAN_POINT ( 'NONE',  ( 810.7187646348534145, -66.45278447660216159, 356.7737145352016341 ) ) ;
#38860 = DIRECTION ( 'NONE',  ( 1.000000000000000000, 4.625929269271485914E-16, 0.000000000000000000 ) ) ;
#38861 = CARTESIAN_POINT ( 'NONE',  ( 745.0891759886404770, -412.2709662947829088, -342.4968714119734159 ) ) ;
#38862 = DIRECTION ( 'NONE',  ( 0.000000000000000000, 0.000000000000000000, 1.000000000000000000 ) ) ;
#38863 = CARTESIAN_POINT ( 'NONE',  ( 752.7379699480933368, -348.0090635724251342, 361.9858362298580232 ) ) ;
#38864 = CARTESIAN_POINT ( 'NONE',  ( 759.0252816721024374, -336.9982390220558273, 368.0189434323527280 ) ) ;
#38865 = CARTESIAN_POINT ( 'NONE',  ( 810.7187646348534145, -42.45278447660223264, -356.7737145352016341 ) ) ;
#38866 = CARTESIAN_POINT ( 'NONE',  ( 771.2633955100217236, -287.9073299311468759, -363.4237431249939618 ) ) ;
#38867 = CARTESIAN_POINT ( 'NONE',  ( -181.9156952255813735, 290.0000000000001137, -274.9999999999999432 ) ) ;
#38868 = CARTESIAN_POINT ( 'NONE',  ( 762.3223304703356007, -415.5436935675102177, 322.3223304703362828 ) ) ;
#38869 = CARTESIAN_POINT ( 'NONE',  ( 804.1105419155481968, -195.8272453906074304, 347.6308680596136469 ) ) ;
#38870 = CARTESIAN_POINT ( 'NONE',  ( 781.2370466360911223, -20.73633629969883430, -304.9990715423533629 ) ) ;
#38871 = CARTESIAN_POINT ( 'NONE',  ( 802.7791456095903868, -76.71468719896012090, -329.0155153010375102 ) ) ;
#38872 = CARTESIAN_POINT ( 'NONE',  ( 744.9990715423526808, -114.3510508353236617, 341.2370466360926002 ) ) ;
#38873 = CARTESIAN_POINT ( 'NONE',  ( 771.2633955100217236, -407.9073299311465348, 363.4237431249939618 ) ) ;
#38874 = DIRECTION ( 'NONE',  ( -0.000000000000000000, -0.6438296778008192334, 0.7651688349527135946 ) ) ;
#38875 = CARTESIAN_POINT ( 'NONE',  ( 800.1688906516307043, -154.1692326535053894, 369.0717654672308186 ) ) ;
#38876 = CARTESIAN_POINT ( 'NONE',  ( 805.1927285166397041, -448.8164208402371855, 341.8018195045277707 ) ) ;
#38877 = ORIENTED_EDGE ( 'NONE', *, *, #5233, .F. ) ;
#38878 = CARTESIAN_POINT ( 'NONE',  ( 800.0135310231082713, -86.08914811296573077, -325.0180583372163028 ) ) ;
#38879 = AXIS2_PLACEMENT_3D ( 'NONE', #7835, #11521, #32308 ) ;
#38880 = CARTESIAN_POINT ( 'NONE',  ( 754.9735926884551418, -402.3510508353228374, -340.5236548041000333 ) ) ;
#38882 = CARTESIAN_POINT ( 'NONE',  ( 755.3201227861273992, -219.7255117493289447, 345.3687786644892981 ) ) ;
#38881 = CARTESIAN_POINT ( 'NONE',  ( 767.8955696845333705, -216.4527844766016926, 362.1676090361162323 ) ) ;
#38883 = CARTESIAN_POINT ( 'NONE',  ( 807.5423716828161105, -393.0783235625954717, -362.2119215644372048 ) ) ;
#38884 = CARTESIAN_POINT ( 'NONE',  ( 754.9967657858570647, -1.543693567511449150, 365.0032342141425374 ) ) ;
#38885 = CARTESIAN_POINT ( 'NONE',  ( 794.9999999999993179, -357.6843811873878280, 0.3380660510726891665 ) ) ;
#38886 = EDGE_LOOP ( 'NONE', ( #7302, #30449 ) ) ;
#38887 = CARTESIAN_POINT ( 'NONE',  ( 768.0187753319979720, -416.6346026584192259, 318.0580252608186242 ) ) ;
#38888 = CIRCLE ( 'NONE', #18962, 10.00000000000000888 ) ;
#38889 = ORIENTED_EDGE ( 'NONE', *, *, #27881, .T. ) ;
#38890 = CONICAL_SURFACE ( 'NONE', #36638, 8.025000000000003908, 0.7853981633974482790 ) ;
#38891 = CARTESIAN_POINT ( 'NONE',  ( 800.9747183278959710, -252.9982390220560831, -311.9810565676471583 ) ) ;
#38892 = CARTESIAN_POINT ( 'NONE',  ( 810.7187646348534145, -162.4527844766018632, 356.7737145352016341 ) ) ;
#38893 = CARTESIAN_POINT ( 'NONE',  ( 758.6633372737375112, -380.5328690171409676, 326.9102291470432533 ) ) ;
#38894 = ORIENTED_EDGE ( 'NONE', *, *, #3815, .T. ) ;
#38895 = CARTESIAN_POINT ( 'NONE',  ( 759.8311093483677041, -190.1692326535052189, 310.9282345327691814 ) ) ;
#38896 = CARTESIAN_POINT ( 'NONE',  ( 788.7366044899766848, -251.9073299311470748, -316.5762568750059813 ) ) ;
#38897 = ORIENTED_EDGE ( 'NONE', *, *, #31530, .T. ) ;
#38898 = CARTESIAN_POINT ( 'NONE',  ( 768.0187753319979720, -368.6346026584193964, -318.0580252608186242 ) ) ;
#38899 = CARTESIAN_POINT ( 'NONE',  ( 755.0636971347428243, -28.27096629478409540, -341.7834795799807353 ) ) ;
#38900 = ADVANCED_FACE ( 'NONE', ( #9787 ), #21101, .T. ) ;
#38901 = CARTESIAN_POINT ( 'NONE',  ( 761.2382568024794409, -231.6237781080504874, 356.9571628226838129 ) ) ;
#38902 = DIRECTION ( 'NONE',  ( -1.000000000000000000, 0.000000000000000000, 0.000000000000000000 ) ) ;
#38903 = CYLINDRICAL_SURFACE ( 'NONE', #44779, 10.00000000000000888 ) ;
#38904 = ORIENTED_EDGE ( 'NONE', *, *, #40553, .T. ) ;
#38905 = CARTESIAN_POINT ( 'NONE',  ( 768.0187753319979720, -8.634602658420517329, -318.0580252608186242 ) ) ;
#38906 = DIRECTION ( 'NONE',  ( 0.000000000000000000, 0.000000000000000000, -1.000000000000000000 ) ) ;
#38907 = CARTESIAN_POINT ( 'NONE',  ( -829.9999999999992042, -600.0000000000000000, -319.9999999999996021 ) ) ;
#38908 = ORIENTED_EDGE ( 'NONE', *, *, #6310, .F. ) ;
#38909 = CARTESIAN_POINT ( 'NONE',  ( 757.7880784355613741, -258.0090635724253616, -312.4576283171834916 ) ) ;
#38910 = CARTESIAN_POINT ( 'NONE',  ( 815.3608509340175488, -146.7363362996984506, 341.2497674668889545 ) ) ;
#38911 = VECTOR ( 'NONE', #36223, 1000.000000000000114 ) ;
#38913 = CARTESIAN_POINT ( 'NONE',  ( 771.2633955100217236, -263.9073299311469327, -363.4237431249939618 ) ) ;
#38912 = CARTESIAN_POINT ( 'NONE',  ( 51.16348990802859475, 260.0000000000000568, -206.1189999999945428 ) ) ;
#38914 = CARTESIAN_POINT ( 'NONE',  ( 769.1273215169530886, -382.7146871989591546, -317.4527132478988847 ) ) ;
#38915 = CARTESIAN_POINT ( 'NONE',  ( 784.9999999999992042, 205.0000000000000568, -274.9999999999999432 ) ) ;
#38916 = CARTESIAN_POINT ( 'NONE',  ( 775.8780910478218402, -129.2817908451530400, -364.9511171171680530 ) ) ;
#38917 = EDGE_CURVE ( 'NONE', #3087, #7747, #25043, .T. ) ;
#38918 = CARTESIAN_POINT ( 'NONE',  ( 744.6391490659812007, -374.7363362996978253, 338.7502325331110455 ) ) ;
#38919 = DIRECTION ( 'NONE',  ( 0.000000000000000000, -0.6755902076156404812, -0.7372773368101421809 ) ) ;
#38920 = CARTESIAN_POINT ( 'NONE',  ( 783.7566961878529810, -0.8965053807785533513, -305.1792804349288417 ) ) ;
#38921 = CARTESIAN_POINT ( 'NONE',  ( 772.5602148656447525, -297.7255117493286889, -305.7998596910095443 ) ) ;
#38922 = DIRECTION ( 'NONE',  ( 0.000000000000000000, 0.000000000000000000, 1.000000000000000000 ) ) ;
#38923 = CARTESIAN_POINT ( 'NONE',  ( 803.6646147819161570, -17.90732993114776406, 348.8264449731210561 ) ) ;
#38924 = CARTESIAN_POINT ( 'NONE',  ( 756.5762568750052424, -75.18005720387485269, -348.7366044899774238 ) ) ;
#38925 = AXIS2_PLACEMENT_3D ( 'NONE', #13931, #31019, #44654 ) ;
#38926 = CARTESIAN_POINT ( 'NONE',  ( 749.5768839229115201, -252.5545181178799226, 358.0661480581553064 ) ) ;
#38927 = CARTESIAN_POINT ( 'NONE',  ( 778.7502325331095108, -192.3510508353233774, -304.6391490659818828 ) ) ;
#38928 = CARTESIAN_POINT ( 'NONE',  ( 748.9653473494363425, -218.6346026584197944, 356.9462024416521331 ) ) ;
#38929 = CARTESIAN_POINT ( 'NONE',  ( 796.7737145352015204, -428.6346026584192259, -370.7187646348536987 ) ) ;
#38930 = CYLINDRICAL_SURFACE ( 'NONE', #6252, 10.00000000000006395 ) ;
#38931 = CARTESIAN_POINT ( 'NONE',  ( 785.3141322388236176, -333.7255117493286320, 364.4286716492789537 ) ) ;
#38932 = CARTESIAN_POINT ( 'NONE',  ( 796.1575198192839480, -102.0090635724258448, 359.4546378042384163 ) ) ;
#38933 = CARTESIAN_POINT ( 'NONE',  ( 757.2208543904082489, 7.285312801039605546, -350.9844846989624330 ) ) ;
#38934 = DIRECTION ( 'NONE',  ( -1.000000000000000000, 2.412474565481389965E-32, 2.750100768424434704E-32 ) ) ;
#38935 = DIRECTION ( 'NONE',  ( -1.000000000000000000, 0.000000000000000000, 0.000000000000000000 ) ) ;
#38937 = CARTESIAN_POINT ( 'NONE',  ( 771.2633955100217236, -359.9073299311467053, 363.4237431249939618 ) ) ;
#38936 = CARTESIAN_POINT ( 'NONE',  ( 754.8983024940795303, -138.8965053807781374, 336.9254006560228163 ) ) ;
#38938 = ORIENTED_EDGE ( 'NONE', *, *, #24678, .T. ) ;
#38939 = CARTESIAN_POINT ( 'NONE',  ( 780.5290396650775619, -300.3510508353230080, -365.2837595273619513 ) ) ;
#38940 = CARTESIAN_POINT ( 'NONE',  ( 791.9812246680005501, -140.6346026584201070, 361.9419747391813189 ) ) ;
#38941 = CARTESIAN_POINT ( 'NONE',  ( 797.8594530101008786, -109.5436935675110988, 322.1405469898980982 ) ) ;
#38942 = CARTESIAN_POINT ( 'NONE',  ( 759.8311093483677041, -286.1692326535048778, -310.9282345327691814 ) ) ;
#38943 = CARTESIAN_POINT ( 'NONE',  ( 767.9999999999992042, 178.9475563372491251, 360.0000000000000000 ) ) ;
#38944 = CARTESIAN_POINT ( 'NONE',  ( 746.7653713866222915, -425.2601417444136018, 351.0478386215610271 ) ) ;
#38945 = ORIENTED_EDGE ( 'NONE', *, *, #10584, .F. ) ;
#38946 = CARTESIAN_POINT ( 'NONE',  ( 801.9419747391806368, -306.4527844766013800, 351.9812246680014027 ) ) ;
#38947 = CARTESIAN_POINT ( 'NONE',  ( 798.7617431975189675, -51.62377810805111267, -323.0428371773161871 ) ) ;
#38948 = CARTESIAN_POINT ( 'NONE',  ( 755.3201227861273992, -171.7255117493291152, -345.3687786644892981 ) ) ;
#38949 = CARTESIAN_POINT ( 'NONE',  ( 756.3353852180819104, -221.9073299311470464, -331.1735550268788302 ) ) ;
#38950 = CARTESIAN_POINT ( 'NONE',  ( 762.3223304703356007, -415.5436935675102177, 322.3223304703362828 ) ) ;
#38951 = CARTESIAN_POINT ( 'NONE',  ( 787.4397851343537695, -141.7255117493291721, -374.2001403089903988 ) ) ;
#38952 = ORIENTED_EDGE ( 'NONE', *, *, #34008, .T. ) ;
#38953 = CARTESIAN_POINT ( 'NONE',  ( 797.6776695296629214, -139.5436935675110135, -357.6776695296636603 ) ) ;
#38954 = VERTEX_POINT ( 'NONE', #37969 ) ;
#38955 = CARTESIAN_POINT ( 'NONE',  ( 763.8424801807145741, -402.0090635724250205, -320.5453621957614700 ) ) ;
#38957 = CARTESIAN_POINT ( 'NONE',  ( 766.9102291470427417, -426.5545181178794678, 318.6633372737382501 ) ) ;
#38956 = CARTESIAN_POINT ( 'NONE',  ( 803.6646147819161570, -113.9073299311474301, 348.8264449731210561 ) ) ;
#38958 = CARTESIAN_POINT ( 'NONE',  ( 803.8651313633788504, -125.2601417444145255, 332.4468031744301015 ) ) ;
#38961 = CARTESIAN_POINT ( 'NONE',  ( 773.7943932421234194, -383.8055962898682765, 305.5313806188329409 ) ) ;
#38960 = CYLINDRICAL_SURFACE ( 'NONE', #1137, 10.00000000000006395 ) ;
#38959 = DIRECTION ( 'NONE',  ( 1.000000000000000000, 0.000000000000000000, 0.000000000000000000 ) ) ;
#38962 = ORIENTED_EDGE ( 'NONE', *, *, #44198, .T. ) ;
#38963 = CARTESIAN_POINT ( 'NONE',  ( 759.0159684113467620, -400.9181544815159555, -325.8855110935213020 ) ) ;
#38964 = CARTESIAN_POINT ( 'NONE',  ( 771.1735550268778070, -369.1800572038739574, -316.3353852180827630 ) ) ;
#38965 = CARTESIAN_POINT ( 'NONE',  ( 755.8990559732751535, -155.4636090269711417, -365.9055244015606831 ) ) ;
#38966 = CARTESIAN_POINT ( 'NONE',  ( 744.6391490659812007, -38.73633629969877035, 338.7502325331110455 ) ) ;
#38968 = LINE ( 'NONE', #24164, #28438 ) ;
#38967 = CARTESIAN_POINT ( 'NONE',  ( 879.9999999999992042, 99.99999999999984368, 360.0000000000000000 ) ) ;
#38969 = CARTESIAN_POINT ( 'NONE',  ( 775.9200461376533440, -287.8055962898685038, -315.3028492785443291 ) ) ;
#38970 = CARTESIAN_POINT ( 'NONE',  ( 799.9999999999993179, 205.0000000000000568, -329.9999999999999432 ) ) ;
#38971 = CARTESIAN_POINT ( 'NONE',  ( 752.7379699480933368, -204.0090635724255606, -361.9858362298580232 ) ) ;
#38972 = DIRECTION ( 'NONE',  ( 0.000000000000000000, 0.000000000000000000, 1.000000000000000000 ) ) ;
#38973 = CYLINDRICAL_SURFACE ( 'NONE', #16428, 8.024999999999948841 ) ;
#38974 = CARTESIAN_POINT ( 'NONE',  ( 755.1538015810308480, -350.1908817542433212, 343.0433043558613804 ) ) ;
#38975 = CARTESIAN_POINT ( 'NONE',  ( 807.2620300519052989, -336.0090635724251911, 318.0141637701419768 ) ) ;
#38976 = CARTESIAN_POINT ( 'NONE',  ( 763.2262854647970016, -200.6346026584199365, -309.2812353651462445 ) ) ;
#38977 = DIRECTION ( 'NONE',  ( 0.000000000000000000, 0.000000000000000000, 1.000000000000000000 ) ) ;
#38978 = CARTESIAN_POINT ( 'NONE',  ( 804.4286716492782716, 6.638124614306706306, -345.3141322388244703 ) ) ;
#38979 = CARTESIAN_POINT ( 'NONE',  ( 754.3581564841646241, -161.4636090269711133, 316.1443688327762516 ) ) ;
#38980 = CARTESIAN_POINT ( 'NONE',  ( 766.5853460496234675, -85.98741447168738716, -372.3518521366060554 ) ) ;
#38981 = CARTESIAN_POINT ( 'NONE',  ( 782.5225473063381969, -118.2709662947837899, 375.2698199232970637 ) ) ;
#38982 = CARTESIAN_POINT ( 'NONE',  ( 810.7187646348534145, -354.4527844766012095, -356.7737145352016341 ) ) ;
#38983 = DIRECTION ( 'NONE',  ( 0.000000000000000000, 0.000000000000000000, 1.000000000000000000 ) ) ;
#38984 = DIRECTION ( 'NONE',  ( -1.000000000000000000, -0.000000000000000000, 0.000000000000000000 ) ) ;
#38985 = CARTESIAN_POINT ( 'NONE',  ( 759.7806653035534055, -174.9982390220563673, 324.8639956371180801 ) ) ;
#38986 = CARTESIAN_POINT ( 'NONE',  ( 804.4086373105744769, -1.645427208789804308, 333.3843516231986541 ) ) ;
#38987 = CARTESIAN_POINT ( 'NONE',  ( 813.2346286133761168, -413.2601417444136018, -328.9521613784389160 ) ) ;
#38988 = CARTESIAN_POINT ( 'NONE',  ( 754.9967657858570647, -409.5436935675101040, -365.0032342141425374 ) ) ;
#38989 = FACE_OUTER_BOUND ( 'NONE', #21017, .T. ) ;
#38990 = CARTESIAN_POINT ( 'NONE',  ( 801.9858362298568863, 20.92167643740319605, 312.7379699480935642 ) ) ;
#38991 = EDGE_LOOP ( 'NONE', ( #19158, #23980 ) ) ;
#38992 = CARTESIAN_POINT ( 'NONE',  ( 778.7502325331095108, -192.3510508353233774, -304.6391490659818828 ) ) ;
#38993 = CARTESIAN_POINT ( 'NONE',  ( -786.4999999999993179, -365.3551492539851893, -18.13243251470705886 ) ) ;
#38994 = CARTESIAN_POINT ( 'NONE',  ( 749.8865473780648472, -308.5328690171412518, 322.1177392798429082 ) ) ;
#38995 = CARTESIAN_POINT ( 'NONE',  ( 792.1044303154646968, -108.4527844766020053, 317.8323909638837677 ) ) ;
#38996 = ORIENTED_EDGE ( 'NONE', *, *, #15433, .F. ) ;
#38997 = CARTESIAN_POINT ( 'NONE',  ( 756.3353852180819104, -317.9073299311468190, 331.1735550268788302 ) ) ;
#38998 = CARTESIAN_POINT ( 'NONE',  ( 805.0032342141412300, -37.54369356751132614, -314.9967657858571783 ) ) ;
#38999 = CARTESIAN_POINT ( 'NONE',  ( 772.4837098697145166, -95.36187538569296862, 374.5518280994205611 ) ) ;
#39000 = ORIENTED_EDGE ( 'NONE', *, *, #40778, .F. ) ;
#39001 = CARTESIAN_POINT ( 'NONE',  ( 749.5768839229115201, -444.5545181178792973, -358.0661480581553064 ) ) ;
#39002 = ORIENTED_EDGE ( 'NONE', *, *, #3532, .F. ) ;
#39003 = SHAPE_DEFINITION_REPRESENTATION ( #7477, #18903 ) ;
#39004 = CARTESIAN_POINT ( 'NONE',  ( 774.6858677611749044, -9.725511749329603717, 315.5713283507209894 ) ) ;
#39005 = CARTESIAN_POINT ( 'NONE',  ( 795.1360043628807261, -308.0891481129650629, -360.2193346964456282 ) ) ;
#39007 = CARTESIAN_POINT ( 'NONE',  ( 781.2497674668890113, -300.3510508353230080, 375.3608509340180603 ) ) ;
#39006 = CARTESIAN_POINT ( 'NONE',  ( 745.4481719005789273, -411.7255117493282910, 347.5162901302853697 ) ) ;
#39008 = CARTESIAN_POINT ( 'NONE',  ( 766.5853460496234675, -85.98741447168738716, 372.3518521366060554 ) ) ;
#39009 = CARTESIAN_POINT ( 'NONE',  ( 763.8424801807145741, -282.0090635724253048, -320.5453621957614700 ) ) ;
#39010 = CARTESIAN_POINT ( 'NONE',  ( 788.8264449731200330, -261.1800572038741848, -363.6646147819171233 ) ) ;
#39011 = LINE ( 'NONE', #20965, #42276 ) ;
#39012 = CARTESIAN_POINT ( 'NONE',  ( 758.0580252608178853, -126.4527844766019626, -328.0187753319985404 ) ) ;
#39013 = FACE_OUTER_BOUND ( 'NONE', #16073, .T. ) ;
#39014 = CIRCLE ( 'NONE', #13221, 19.99999999999990763 ) ;
#39015 = CARTESIAN_POINT ( 'NONE',  ( 814.2001403089898304, -401.3618753856920307, 347.4397851343538264 ) ) ;
#39017 = CARTESIAN_POINT ( 'NONE',  ( -180.7583438952258916, 294.6698570112193920, -274.9999999999999432 ) ) ;
#39016 = DIRECTION ( 'NONE',  ( 0.000000000000000000, 0.000000000000000000, 1.000000000000000000 ) ) ;
#39018 = CARTESIAN_POINT ( 'NONE',  ( 748.6759233522253680, -64.37269993606231822, -324.3348316497537098 ) ) ;
#39019 = PLANE ( 'NONE',  #31510 ) ;
#39020 = DIRECTION ( 'NONE',  ( -1.880165489482579047E-16, -1.000000000000000000, -0.000000000000000000 ) ) ;
#39021 = CARTESIAN_POINT ( 'NONE',  ( 787.5531968255692163, -261.8272453906071746, 316.1348686366205811 ) ) ;
#39022 = CARTESIAN_POINT ( 'NONE',  ( 797.6776695296629214, -163.5436935675109567, 357.6776695296636603 ) ) ;
#39023 = ORIENTED_EDGE ( 'NONE', *, *, #39102, .F. ) ;
#39024 = CARTESIAN_POINT ( 'NONE',  ( 766.9102291470427417, -18.55451811788065797, -318.6633372737382501 ) ) ;
#39025 = CARTESIAN_POINT ( 'NONE',  ( 814.2001403089898304, -113.3618753856929260, -347.4397851343538264 ) ) ;
#39026 = CARTESIAN_POINT ( 'NONE',  ( 756.7813123517142913, -307.9874144716866340, 329.9779781133712504 ) ) ;
#39027 = DIRECTION ( 'NONE',  ( -1.880165489482579047E-16, -1.000000000000000000, -0.000000000000000000 ) ) ;
#39028 = CARTESIAN_POINT ( 'NONE',  ( 810.4231160770870019, -24.55451811788064020, 321.9338519418446936 ) ) ;
#39029 = CARTESIAN_POINT ( 'NONE',  ( 746.8695393053150156, -221.9073299311470464, -327.6429770376306010 ) ) ;
#39030 = EDGE_CURVE ( 'NONE', #17123, #42371, #34723, .T. ) ;
#39031 = CARTESIAN_POINT ( 'NONE',  ( 751.6929314249748586, -198.9982390220562252, 318.8095938919659034 ) ) ;
#39032 = CARTESIAN_POINT ( 'NONE',  ( 805.1927285166397041, -88.81642084023842187, 341.8018195045277707 ) ) ;
#39033 = CARTESIAN_POINT ( 'NONE',  ( 773.4999999999993179, 26.27639943461401018, 900.0000000000001137 ) ) ;
#39034 = CARTESIAN_POINT ( 'NONE',  ( 781.2497674668890113, -300.3510508353230080, -375.3608509340180603 ) ) ;
#39035 = CARTESIAN_POINT ( 'NONE',  ( 764.1737431748507561, -442.3726999360611103, 371.6461892240376415 ) ) ;
#39036 = CARTESIAN_POINT ( 'NONE',  ( 747.2067596250078623, -315.1800572038740711, -352.2312462859687230 ) ) ;
#39037 = CARTESIAN_POINT ( 'NONE',  ( 911.9999999999994316, 219.9999999999998863, -360.0000000000000000 ) ) ;
#39038 = CARTESIAN_POINT ( 'NONE',  ( 773.3843516231979720, -349.4419599262320162, 364.4086373105754433 ) ) ;
#39039 = CARTESIAN_POINT ( 'NONE',  ( 763.2262854647970016, -32.63460265842044095, 309.2812353651462445 ) ) ;
#39040 = CARTESIAN_POINT ( 'NONE',  ( 797.6776695296629214, -403.5436935675101608, -357.6776695296636603 ) ) ;
#39041 = CARTESIAN_POINT ( 'NONE',  ( 766.7756240680305382, -62.53286901714199786, 361.5560724626415663 ) ) ;
#39042 = CARTESIAN_POINT ( 'NONE',  ( 768.0187753319979720, -200.6346026584199365, -318.0580252608186242 ) ) ;
#39043 = CARTESIAN_POINT ( 'NONE',  ( 768.8385539511368734, -71.26014174441469606, -306.4236121716840557 ) ) ;
#39044 = CARTESIAN_POINT ( 'NONE',  ( 752.4576283171824116, -213.0783235625960401, 317.7880784355627952 ) ) ;
#39045 = CARTESIAN_POINT ( 'NONE',  ( 759.9864689768902508, -26.08914811296592262, 354.9819416627836404 ) ) ;
#39046 = VECTOR ( 'NONE', #26560, 1000.000000000000000 ) ;
#39047 = ORIENTED_EDGE ( 'NONE', *, *, #22135, .F. ) ;
#39048 = CARTESIAN_POINT ( 'NONE',  ( 756.7813123517142913, -187.9874144716870603, -329.9779781133712504 ) ) ;
#39049 = CARTESIAN_POINT ( 'NONE',  ( 778.2165204200184689, -214.8164208402380666, 364.9363028652563230 ) ) ;
#39050 = EDGE_CURVE ( 'NONE', #6536, #37165, #17173, .T. ) ;
#39051 = CARTESIAN_POINT ( 'NONE',  ( 758.0141637701419768, -39.07832356259662276, -367.2620300519063790 ) ) ;
#39052 = CARTESIAN_POINT ( 'NONE',  ( 755.3201227861273992, -315.7255117493286320, 345.3687786644892981 ) ) ;
#39053 = CARTESIAN_POINT ( 'NONE',  ( 790.0183182880230106, -452.9681489794449476, -362.9048749981275250 ) ) ;
#39054 = CARTESIAN_POINT ( 'NONE',  ( 919.9999999999993179, 219.9999999999998863, 350.0000000000000000 ) ) ;
#39055 = ORIENTED_EDGE ( 'NONE', *, *, #28677, .F. ) ;
#39056 = CARTESIAN_POINT ( 'NONE',  ( 764.0069404352550464, -63.07832356259653750, 359.2566176426627180 ) ) ;
#39057 = CARTESIAN_POINT ( 'NONE',  ( 778.7629533639073998, -344.7363362996978253, -375.0009284576466371 ) ) ;
#39058 = EDGE_CURVE ( 'NONE', #20274, #3603, #34503, .T. ) ;
#39059 = CARTESIAN_POINT ( 'NONE',  ( 754.9967657858570647, -241.5436935675106440, 365.0032342141425943 ) ) ;
#39060 = CARTESIAN_POINT ( 'NONE',  ( 746.0683387631852383, 4.558040073766884248, 331.3260364891676204 ) ) ;
#39061 = CARTESIAN_POINT ( 'NONE',  ( 757.0176451133909268, -157.0999726633347962, -349.9200121543848354 ) ) ;
#39062 = CARTESIAN_POINT ( 'NONE',  ( 756.5762568750052424, -147.1800572038746395, -348.7366044899774238 ) ) ;
#39063 = CARTESIAN_POINT ( 'NONE',  ( 804.4286716492782716, -353.3618753856922012, -345.3141322388244703 ) ) ;
#39064 = VERTEX_POINT ( 'NONE', #31495 ) ;
#39065 = CARTESIAN_POINT ( 'NONE',  ( 801.9419747391806368, -450.4527844766009821, -351.9812246680014027 ) ) ;
#39066 = CARTESIAN_POINT ( 'NONE',  ( 814.2001403089898304, -281.3618753856923718, 347.4397851343538264 ) ) ;
#39067 = CARTESIAN_POINT ( 'NONE',  ( 793.5337260303429048, -457.7979077669877483, 366.8220830107578649 ) ) ;
#39068 = CARTESIAN_POINT ( 'NONE',  ( 780.5290396650775619, -348.3510508353228943, 365.2837595273619513 ) ) ;
#39069 = CARTESIAN_POINT ( 'NONE',  ( 998.9999999999992042, 479.9999999999999432, 360.0000000000000000 ) ) ;
#39070 = CARTESIAN_POINT ( 'NONE',  ( 802.9823548866075953, -169.0999726633347393, 330.0799878456151077 ) ) ;
#39071 = CARTESIAN_POINT ( 'NONE',  ( 755.3201227861273992, -27.72551174932954510, 345.3687786644892981 ) ) ;
#39072 = EDGE_LOOP ( 'NONE', ( #31251, #3425, #8108, #35343 ) ) ;
#39073 = CARTESIAN_POINT ( 'NONE',  ( 745.1792804349281596, -374.1908817542432075, -343.7566961878542884 ) ) ;
#39074 = CARTESIAN_POINT ( 'NONE',  ( 814.2001403089898304, 6.638124614306706306, -347.4397851343538264 ) ) ;
#39075 = CARTESIAN_POINT ( 'NONE',  ( 802.2119215644370342, -270.0090635724253048, 367.5423716828165084 ) ) ;
#39076 = CARTESIAN_POINT ( 'NONE',  ( 790.8726784830453198, -202.7146871989597514, 362.5472867521010585 ) ) ;
#39077 = CARTESIAN_POINT ( 'NONE',  ( 778.1981804954714335, -346.2709662947830793, -314.8072714833589885 ) ) ;
#39078 = EDGE_CURVE ( 'NONE', #18205, #911, #2925, .T. ) ;
#39079 = CARTESIAN_POINT ( 'NONE',  ( 774.6312213355099630, 0.6381246143067236254, 364.6798772138717482 ) ) ;
#39080 = DIRECTION ( 'NONE',  ( -1.000000000000000000, -0.000000000000000000, -0.000000000000000000 ) ) ;
#39081 = CARTESIAN_POINT ( 'NONE',  ( 793.9708237608222134, -214.9181544815164386, -319.2295555964448681 ) ) ;
#39082 = CARTESIAN_POINT ( 'NONE',  ( 804.7487373415286811, -19.54369356751139364, 364.7487373415288516 ) ) ;
#39083 = CARTESIAN_POINT ( 'NONE',  ( 787.4999999999992042, -462.9681489794447202, 270.0000000000000568 ) ) ;
#39084 = CARTESIAN_POINT ( 'NONE',  ( 782.5225473063383106, -430.2709662947827383, -375.2698199232970637 ) ) ;
#39085 = DIRECTION ( 'NONE',  ( 0.000000000000000000, 1.000000000000000000, 0.000000000000000000 ) ) ;
#39086 = CARTESIAN_POINT ( 'NONE',  ( 760.0363995740630116, -370.9181544815159555, 368.7758568127991907 ) ) ;
#39087 = CARTESIAN_POINT ( 'NONE',  ( 809.7763221938408833, -453.1000272243879863, -336.1997354883953903 ) ) ;
#39088 = CARTESIAN_POINT ( 'NONE',  ( 745.7998596910086917, -341.3618753856922012, 332.5602148656461168 ) ) ;
#39089 = CARTESIAN_POINT ( 'NONE',  ( 814.2001403089898304, -65.36187538569306810, -347.4397851343538264 ) ) ;
#39090 = CARTESIAN_POINT ( 'NONE',  ( 767.8955696845333705, -288.4527844766014937, -362.1676090361162323 ) ) ;
#39091 = FACE_BOUND ( 'NONE', #42430, .T. ) ;
#39092 = CARTESIAN_POINT ( 'NONE',  ( 757.8323909638827445, -434.6346026584190554, 352.1044303154654358 ) ) ;
#39093 = CARTESIAN_POINT ( 'NONE',  ( 757.4527132478984868, -184.3726999360619629, 329.1273215169538844 ) ) ;
#39094 = CARTESIAN_POINT ( 'NONE',  ( 812.3518521366052028, -73.09997266333502353, -326.5853460496235243 ) ) ;
#39095 = CARTESIAN_POINT ( 'NONE',  ( 763.2154366446407039, -69.62377810805107003, -321.4292242960311228 ) ) ;
#39096 = CARTESIAN_POINT ( 'NONE',  ( 808.7758568127978833, -100.1692326535055315, 320.0363995740631822 ) ) ;
#39097 = CARTESIAN_POINT ( 'NONE',  ( 788.7366044899766848, -395.9073299311465348, 316.5762568750059813 ) ) ;
#39098 = EDGE_CURVE ( 'NONE', #35055, #29607, #30811, .T. ) ;
#39099 = CARTESIAN_POINT ( 'NONE',  ( 785.3687786644884454, 12.63812461430668321, -315.3201227861279676 ) ) ;
#39100 = ORIENTED_EDGE ( 'NONE', *, *, #12287, .T. ) ;
#39101 = CARTESIAN_POINT ( 'NONE',  ( 762.1405469898971887, -97.54369356751112718, -357.8594530101015607 ) ) ;
#39102 = EDGE_CURVE ( 'NONE', #10345, #1685, #5129, .T. ) ;
#39103 = CARTESIAN_POINT ( 'NONE',  ( 783.0433043558608688, -384.8965053807772847, -315.1538015810313027 ) ) ;
#39105 = CARTESIAN_POINT ( 'NONE',  ( 771.2633955100217236, -239.9073299311470748, 363.4237431249939618 ) ) ;
#39104 = CARTESIAN_POINT ( 'NONE',  ( 785.3687786644884454, -227.3618753856925707, 315.3201227861279676 ) ) ;
#39106 = EDGE_LOOP ( 'NONE', ( #35571, #24726, #30614, #32346 ) ) ;
#39107 = CARTESIAN_POINT ( 'NONE',  ( 815.0009284576459549, -414.3510508353227237, -338.7629533639073429 ) ) ;
#39108 = DIRECTION ( 'NONE',  ( -1.000000000000000000, 0.000000000000000000, 0.000000000000000000 ) ) ;
#39109 = ORIENTED_EDGE ( 'NONE', *, *, #14545, .F. ) ;
#39110 = CARTESIAN_POINT ( 'NONE',  ( 762.3223304703356007, -415.5436935675102177, 322.3223304703362828 ) ) ;
#39111 = ORIENTED_EDGE ( 'NONE', *, *, #44388, .F. ) ;
#39112 = EDGE_CURVE ( 'NONE', #40969, #5059, #29473, .T. ) ;
#39113 = CARTESIAN_POINT ( 'NONE',  ( 746.8695393053150156, -245.9073299311469896, -327.6429770376306010 ) ) ;
#39114 = CARTESIAN_POINT ( 'NONE',  ( 772.4837098697145166, -167.3618753856927412, 374.5518280994205611 ) ) ;
#39115 = CARTESIAN_POINT ( 'NONE',  ( 763.8424801807145741, -258.0090635724253616, 320.5453621957614700 ) ) ;
#39116 = CARTESIAN_POINT ( 'NONE',  ( 754.8983024940795303, -378.8965053807772847, 336.9254006560228163 ) ) ;
#39117 = VERTEX_POINT ( 'NONE', #13722 ) ;
#39118 = CARTESIAN_POINT ( 'NONE',  ( 802.5472867521000353, -52.37269993606237506, -350.8726784830461156 ) ) ;
#39119 = CARTESIAN_POINT ( 'NONE',  ( 759.7806653035535192, -246.9982390220560831, -324.8639956371181370 ) ) ;
#39120 = ORIENTED_EDGE ( 'NONE', *, *, #9907, .F. ) ;
#39121 = CARTESIAN_POINT ( 'NONE',  ( 797.8594530101008786, -373.5436935675101040, -322.1405469898980982 ) ) ;
#39122 = CARTESIAN_POINT ( 'NONE',  ( 781.7834795799800531, -10.81642084023869543, -315.0636971347436202 ) ) ;
#39123 = CARTESIAN_POINT ( 'NONE',  ( 789.9200121543843807, -217.9874144716870035, 317.0176451133914384 ) ) ;
#39124 = CARTESIAN_POINT ( 'NONE',  ( -208.8365100919714052, 240.0000000000000853, -202.7499999999925251 ) ) ;
#39125 = CARTESIAN_POINT ( 'NONE',  ( 989.9999999999992042, -434.4637272565419153, -347.3621835540870393 ) ) ;
#39126 = ORIENTED_EDGE ( 'NONE', *, *, #3842, .F. ) ;
#39127 = CARTESIAN_POINT ( 'NONE',  ( 795.1360043628807261, -20.08914811296592973, -360.2193346964456282 ) ) ;
#39128 = CARTESIAN_POINT ( 'NONE',  ( 775.4999999999993179, -544.8427095258973623, -350.0000000000000000 ) ) ;
#39129 = DIRECTION ( 'NONE',  ( -0.000000000000000000, 0.9235249282889856914, -0.3835384033298670503 ) ) ;
#39130 = EDGE_LOOP ( 'NONE', ( #28529, #9041 ) ) ;
#39131 = CARTESIAN_POINT ( 'NONE',  ( 757.7880784355613741, -282.0090635724253048, -312.4576283171834916 ) ) ;
#39132 = EDGE_CURVE ( 'NONE', #10075, #12108, #6552, .T. ) ;
#39133 = CARTESIAN_POINT ( 'NONE',  ( 813.5763878283155464, -147.8272453906075157, 351.1614460488615350 ) ) ;
#39135 = CARTESIAN_POINT ( 'NONE',  ( 758.0580252608178853, -270.4527844766014937, -328.0187753319985404 ) ) ;
#39134 = DIRECTION ( 'NONE',  ( 1.000000000000000000, 0.000000000000000000, 0.000000000000000000 ) ) ;
#39136 = ADVANCED_FACE ( 'NONE', ( #24541 ), #38654, .F. ) ;
#39137 = LINE ( 'NONE', #7487, #28113 ) ;
#39138 = CARTESIAN_POINT ( 'NONE',  ( 793.9708237608222134, -118.9181544815167229, -319.2295555964448681 ) ) ;
#39139 = DIRECTION ( 'NONE',  ( -1.000000000000000000, 0.000000000000000000, 0.000000000000000000 ) ) ;
#39140 = CARTESIAN_POINT ( 'NONE',  ( 788.4001350590139054, -443.1233509495419298, -363.5803521658918385 ) ) ;
#39141 = CARTESIAN_POINT ( 'NONE',  ( 810.7187646348534145, -306.4527844766013800, -356.7737145352016341 ) ) ;
#39142 = DIRECTION ( 'NONE',  ( -0.000000000000000000, 1.000000000000000000, -0.000000000000000000 ) ) ;
#39143 = CARTESIAN_POINT ( 'NONE',  ( 805.1927285166397041, -16.81642084023866701, 341.8018195045277707 ) ) ;
#39144 = CARTESIAN_POINT ( 'NONE',  ( 745.5313806188320314, -255.2817908451526705, 333.7943932421247268 ) ) ;
#39145 = CARTESIAN_POINT ( 'NONE',  ( 815.1787889125755555, -198.8965053807779384, -343.7953271457877804 ) ) ;
#39146 = CARTESIAN_POINT ( 'NONE',  ( 815.2698199232961542, -232.8164208402379245, 342.5225473063383106 ) ) ;
#39147 = CARTESIAN_POINT ( 'NONE',  ( 814.2001403089898304, -449.3618753856918602, -347.4397851343538264 ) ) ;
#39148 = LINE ( 'NONE', #31524, #29864 ) ;
#39149 = CARTESIAN_POINT ( 'NONE',  ( 767.8955696845333705, -312.4527844766012663, 362.1676090361162323 ) ) ;
#39150 = CARTESIAN_POINT ( 'NONE',  ( 802.5472867521000353, -100.3726999360622187, 350.8726784830461156 ) ) ;
#39151 = CARTESIAN_POINT ( 'NONE',  ( 802.5472867521000353, -100.3726999360622187, 350.8726784830461156 ) ) ;
#39152 = CARTESIAN_POINT ( 'NONE',  ( 801.9419747391806368, -450.4527844766009821, -351.9812246680014027 ) ) ;
#39153 = LINE ( 'NONE', #10974, #42432 ) ;
#39154 = EDGE_CURVE ( 'NONE', #31261, #29612, #43256, .T. ) ;
#39155 = DIRECTION ( 'NONE',  ( 1.000000000000000000, 0.000000000000000000, -0.000000000000000000 ) ) ;
#39157 = CARTESIAN_POINT ( 'NONE',  ( 762.3223304703356007, -367.5436935675102745, 322.3223304703362828 ) ) ;
#39156 = CARTESIAN_POINT ( 'NONE',  ( 803.2186876482843445, -151.9874144716871740, 350.0220218866286928 ) ) ;
#39158 = EDGE_LOOP ( 'NONE', ( #22269, #15542, #25967, #43159, #39379, #139, #16189, #21074, #20398, #16898, #5348, #15737 ) ) ;
#39159 = CARTESIAN_POINT ( 'NONE',  ( 802.1676090361156639, -38.63460265842041252, -327.8955696845344505 ) ) ;
#39160 = ADVANCED_FACE ( 'NONE', ( #304 ), #43026, .F. ) ;
#39161 = CARTESIAN_POINT ( 'NONE',  ( 756.7813123517142913, -283.9874144716867477, -329.9779781133712504 ) ) ;
#39162 = CARTESIAN_POINT ( 'NONE',  ( 788.7366044899766848, -131.9073299311473875, 316.5762568750059813 ) ) ;
#39163 = CARTESIAN_POINT ( 'NONE',  ( 808.7758568127978833, -292.1692326535048210, -320.0363995740631822 ) ) ;
#39164 = DIRECTION ( 'NONE',  ( 1.000000000000000000, 0.000000000000000000, 0.000000000000000000 ) ) ;
#39165 = CARTESIAN_POINT ( 'NONE',  ( 793.4146539503750546, -409.9874144716863498, 307.6481478633938877 ) ) ;
#39166 = ORIENTED_EDGE ( 'NONE', *, *, #13973, .T. ) ;
#39167 = CARTESIAN_POINT ( 'NONE',  ( 791.9812246680005501, -308.6346026584195670, 361.9419747391813189 ) ) ;
#39168 = CARTESIAN_POINT ( 'NONE',  ( 755.8398074228967971, -91.44195992623282621, -333.4516893846970333 ) ) ;
#39169 = CARTESIAN_POINT ( 'NONE',  ( 759.7806653035534055, -150.9982390220563957, -324.8639956371180801 ) ) ;
#39170 = CARTESIAN_POINT ( 'NONE',  ( 788.7366044899766848, -203.9073299311471885, -316.5762568750059813 ) ) ;
#39171 = CARTESIAN_POINT ( 'NONE',  ( 755.0636971347428243, -412.2709662947829088, 341.7834795799807353 ) ) ;
#39172 = EDGE_CURVE ( 'NONE', #36537, #27668, #31710, .T. ) ;
#39173 = CARTESIAN_POINT ( 'NONE',  ( 767.6429770376289525, -153.1800572038746395, -306.8695393053162093 ) ) ;
#39174 = EDGE_LOOP ( 'NONE', ( #33129, #15463 ) ) ;
#39175 = CARTESIAN_POINT ( 'NONE',  ( 755.0636971347428243, -148.2709662947837330, -341.7834795799807353 ) ) ;
#39176 = ORIENTED_EDGE ( 'NONE', *, *, #29090, .T. ) ;
#39177 = CARTESIAN_POINT ( 'NONE',  ( 787.5531968255692163, -405.8272453906067199, -316.1348686366205811 ) ) ;
#39178 = CARTESIAN_POINT ( 'NONE',  ( 804.4086373105744769, -433.6454272087884760, 333.3843516231986541 ) ) ;
#39179 = CARTESIAN_POINT ( 'NONE',  ( 758.6633372737375112, -140.5328690171417634, 326.9102291470432533 ) ) ;
#39182 = CARTESIAN_POINT ( 'NONE',  ( 798.0661480581538854, -386.5328690171409676, 309.5768839229118043 ) ) ;
#39181 = LINE ( 'NONE', #43313, #41734 ) ;
#39180 = DIRECTION ( 'NONE',  ( 1.000000000000000000, 0.000000000000000000, 0.000000000000000000 ) ) ;
#39183 = ORIENTED_EDGE ( 'NONE', *, *, #33660, .T. ) ;
#39184 = CARTESIAN_POINT ( 'NONE',  ( 773.4516893846965786, -403.6454272087884760, -315.8398074228977066 ) ) ;
#39185 = CYLINDRICAL_SURFACE ( 'NONE', #29252, 19.99999999999990763 ) ;
#39186 = CARTESIAN_POINT ( 'NONE',  ( 745.5313806188320314, -183.2817908451528695, -333.7943932421247268 ) ) ;
#39187 = CARTESIAN_POINT ( 'NONE',  ( 762.1177392798416577, -18.55451811788065797, 309.8865473780659272 ) ) ;
#39189 = DIRECTION ( 'NONE',  ( 1.000000000000000000, 0.000000000000000000, 0.000000000000000000 ) ) ;
#39188 = DIRECTION ( 'NONE',  ( 0.000000000000000000, 0.000000000000000000, -1.000000000000000000 ) ) ;
#39190 = CARTESIAN_POINT ( 'NONE',  ( 755.0488828828309806, -305.8055962898684470, -344.1219089521771934 ) ) ;
#39191 = CARTESIAN_POINT ( 'NONE',  ( 757.8323909638827445, -434.6346026584190554, -352.1044303154654358 ) ) ;
#39192 = CARTESIAN_POINT ( 'NONE',  ( 773.7305795820266212, -177.2817908451528695, -374.8230680027170365 ) ) ;
#39193 = CARTESIAN_POINT ( 'NONE',  ( 759.9999999999992042, -512.9681489794448908, -309.9999999999998863 ) ) ;
#39194 = DIRECTION ( 'NONE',  ( 1.000000000000000000, 0.000000000000000000, 0.000000000000000000 ) ) ;
#39195 = CARTESIAN_POINT ( 'NONE',  ( 755.1538015810308480, -374.1908817542432075, 343.0433043558613804 ) ) ;
#39196 = CARTESIAN_POINT ( 'NONE',  ( 768.9521613784389729, -345.8272453906069472, 373.2346286133773106 ) ) ;
#39197 = CARTESIAN_POINT ( 'NONE',  ( 745.0891759886404770, -220.2709662947834772, -342.4968714119734159 ) ) ;
#39198 = FACE_OUTER_BOUND ( 'NONE', #39072, .T. ) ;
#39199 = DIRECTION ( 'NONE',  ( 0.000000000000000000, 0.000000000000000000, -1.000000000000000000 ) ) ;
#39200 = CARTESIAN_POINT ( 'NONE',  ( 755.8990559732751535, -155.4636090269711417, 365.9055244015606831 ) ) ;
#39201 = CARTESIAN_POINT ( 'NONE',  ( 793.4146539503750546, -97.98741447168734453, -307.6481478633938877 ) ) ;
#39202 = CARTESIAN_POINT ( 'NONE',  ( 796.9462024416508257, -108.4527844766019911, 308.9653473494370246 ) ) ;
#39203 = CARTESIAN_POINT ( 'NONE',  ( 744.7301800767019131, -340.8164208402376971, -337.4774526936615757 ) ) ;
#39204 = DIRECTION ( 'NONE',  ( 0.000000000000000000, 0.000000000000000000, -1.000000000000000000 ) ) ;
#39205 = CARTESIAN_POINT ( 'NONE',  ( -746.4999999999993179, -359.5698779088871788, -26.28906389436294688 ) ) ;
#39206 = CARTESIAN_POINT ( 'NONE',  ( 767.8955696845333705, -216.4527844766016926, 362.1676090361162323 ) ) ;
#39207 = CARTESIAN_POINT ( 'NONE',  ( 773.4516893846965786, 4.354572791210176597, 315.8398074228977066 ) ) ;
#39208 = CARTESIAN_POINT ( 'NONE',  ( 778.7502325331095108, -408.3510508353227806, -304.6391490659818828 ) ) ;
#39209 = CARTESIAN_POINT ( 'NONE',  ( 787.4397851343537695, -429.7255117493282910, -374.2001403089903988 ) ) ;
#39210 = CARTESIAN_POINT ( 'NONE',  ( 311.1634899080286232, 256.5000000000000000, -193.8809999999963338 ) ) ;
#39211 = CARTESIAN_POINT ( 'NONE',  ( 813.9316612368132837, -7.441959926233078448, 348.6739635108323228 ) ) ;
#39212 = VERTEX_POINT ( 'NONE', #77 ) ;
#39213 = CIRCLE ( 'NONE', #19273, 7.999999999999896083 ) ;
#39214 = CARTESIAN_POINT ( 'NONE',  ( 815.0009284576459549, -198.3510508353234059, -338.7629533639073429 ) ) ;
#39215 = FILL_AREA_STYLE ('',( #32278 ) ) ;
#39216 = CARTESIAN_POINT ( 'NONE',  ( 746.7653713866222915, -305.2601417444139429, 351.0478386215610271 ) ) ;
#39217 = CARTESIAN_POINT ( 'NONE',  ( 804.4286716492782716, -161.3618753856927697, 345.3141322388244703 ) ) ;
#39218 = ORIENTED_EDGE ( 'NONE', *, *, #6355, .T. ) ;
#39219 = CARTESIAN_POINT ( 'NONE',  ( 771.1735550268778070, -321.1800572038740142, 316.3353852180827630 ) ) ;
#39220 = CARTESIAN_POINT ( 'NONE',  ( 814.9108240113580450, -40.27096629478405987, -337.5031285880265273 ) ) ;
#39221 = CARTESIAN_POINT ( 'NONE',  ( 751.9810565676468741, -74.08914811296577341, 360.9747183278973921 ) ) ;
#39222 = ADVANCED_BREP_SHAPE_REPRESENTATION ( '', ( #1418, #33391, #17697, #3320, #26858 ), #34210 ) ;
#39223 = CARTESIAN_POINT ( 'NONE',  ( 786.2694204179717872, -453.2817908451519315, -305.1769319972829067 ) ) ;
#39224 = ORIENTED_EDGE ( 'NONE', *, *, #10590, .T. ) ;
#39225 = SHAPE_DEFINITION_REPRESENTATION ( #17417, #36841 ) ;
#39226 = CARTESIAN_POINT ( 'NONE',  ( 762.3223304703356007, -31.54369356751135456, 322.3223304703362828 ) ) ;
#39227 = CARTESIAN_POINT ( 'NONE',  ( 767.8955696845333705, -288.4527844766014937, -362.1676090361162323 ) ) ;
#39229 = CARTESIAN_POINT ( 'NONE',  ( 811.6461892240364477, -292.7146871989594956, 324.1737431748509835 ) ) ;
#39228 = CARTESIAN_POINT ( 'NONE',  ( 763.0537975583476964, -384.4527844766011526, 371.0346526505628617 ) ) ;
#39230 = CARTESIAN_POINT ( 'NONE',  ( 776.2433038121456548, -60.89650538077837894, 374.8207195650711014 ) ) ;
#39231 = CARTESIAN_POINT ( 'NONE',  ( 766.0291762391763086, -274.9181544815161828, -360.7704444035551319 ) ) ;
#39232 = CARTESIAN_POINT ( 'NONE',  ( 800.0135310231082713, -278.0891481129651197, -325.0180583372163028 ) ) ;
#39233 = CARTESIAN_POINT ( 'NONE',  ( 759.7806653035535192, -438.9982390220554294, -324.8639956371181370 ) ) ;
#39234 = CARTESIAN_POINT ( 'NONE',  ( 794.9819416627830151, -132.9982390220564810, -319.9864689768909898 ) ) ;
#39235 = CARTESIAN_POINT ( 'NONE',  ( 919.9999999999993179, 154.9999999999998863, -360.0000000000000000 ) ) ;
#39236 = CARTESIAN_POINT ( 'NONE',  ( 801.1904061080336987, -380.0891481129646650, 368.3070685750235498 ) ) ;
#39238 = DIRECTION ( 'NONE',  ( 1.000000000000000000, 0.000000000000000000, 0.000000000000000000 ) ) ;
#39237 = DIRECTION ( 'NONE',  ( -0.000000000000000000, -3.700743415417198493E-16, 1.000000000000000000 ) ) ;
#39239 = CARTESIAN_POINT ( 'NONE',  ( 811.3240766477731540, -76.37269993606228979, -355.6651683502462902 ) ) ;
#39240 = DIRECTION ( 'NONE',  ( 0.000000000000000000, 0.000000000000000000, 1.000000000000000000 ) ) ;
#39241 = CARTESIAN_POINT ( 'NONE',  ( -786.4999999999993179, 26.27639943461401018, 900.0000000000001137 ) ) ;
#39242 = CARTESIAN_POINT ( 'NONE',  ( 775.8780910478218402, -249.2817908451526421, 364.9511171171680530 ) ) ;
#39243 = CARTESIAN_POINT ( 'NONE',  ( 765.0180583372156207, -168.9982390220563673, 360.0135310231089534 ) ) ;
#39244 = EDGE_LOOP ( 'NONE', ( #15979, #25907, #13716, #44543 ) ) ;
#39245 = CARTESIAN_POINT ( 'NONE',  ( 796.9571628226829034, -47.46360902697148987, -321.2382568024804641 ) ) ;
#39246 = VECTOR ( 'NONE', #21046, 1000.000000000000000 ) ;
#39247 = CARTESIAN_POINT ( 'NONE',  ( 759.0252816721024374, -96.99823902205660886, -368.0189434323527280 ) ) ;
#39248 = CARTESIAN_POINT ( 'NONE',  ( 795.9930595647434757, -339.0783235625956422, 320.7433823573372820 ) ) ;
#39249 = CARTESIAN_POINT ( 'NONE',  ( 759.9999999999992042, -512.9681489794448908, 329.9999999999999432 ) ) ;
#39250 = CARTESIAN_POINT ( 'NONE',  ( 811.3240766477731540, -28.37269993606244967, 355.6651683502462902 ) ) ;
#39251 = CARTESIAN_POINT ( 'NONE',  ( 792.2312462859673587, -227.9073299311471033, -307.2067596250082602 ) ) ;
#39252 = CARTESIAN_POINT ( 'NONE',  ( 804.9363028652555840, -112.2709662947838325, 338.2165204200192079 ) ) ;
#39253 =( NAMED_UNIT ( * ) PLANE_ANGLE_UNIT ( ) SI_UNIT ( $, .RADIAN. ) );
#39254 = CARTESIAN_POINT ( 'NONE',  ( 744.9990715423526808, -306.3510508353230648, -341.2370466360926002 ) ) ;
#39255 = CARTESIAN_POINT ( 'NONE',  ( 781.2370466360911223, -452.7363362996975411, 304.9990715423533629 ) ) ;
#39256 = CARTESIAN_POINT ( 'NONE',  ( 751.6929314249748586, -318.9982390220557704, -318.8095938919659034 ) ) ;
#39257 = CARTESIAN_POINT ( 'NONE',  ( 780.5290396650775619, -348.3510508353228943, 365.2837595273619513 ) ) ;
#39258 = CARTESIAN_POINT ( 'NONE',  ( 811.0346526505617248, -62.63460265842032726, 323.0537975583478101 ) ) ;
#39259 = CARTESIAN_POINT ( 'NONE',  ( 791.9812246680005501, -428.6346026584192259, -361.9419747391813189 ) ) ;
#39260 = CARTESIAN_POINT ( 'NONE',  ( 755.8398074228967971, -43.44195992623296831, 333.4516893846970333 ) ) ;
#39261 = CARTESIAN_POINT ( 'NONE',  ( 751.2241431872005251, -88.16923265350555994, -359.9636004259367610 ) ) ;
#39262 = CARTESIAN_POINT ( 'NONE',  ( 788.7631598425961101, -217.4419599262324141, 305.7194118038759143 ) ) ;
#39263 = CARTESIAN_POINT ( 'NONE',  ( 755.3201227861273992, -3.725511749329622813, 345.3687786644892981 ) ) ;
#39264 = VERTEX_POINT ( 'NONE', #28240 ) ;
#39265 = CARTESIAN_POINT ( 'NONE',  ( 757.2208543904082489, -184.7146871989598083, -350.9844846989624330 ) ) ;
#39266 = CARTESIAN_POINT ( 'NONE',  ( 791.9812246680005501, -188.6346026584199365, 361.9419747391813189 ) ) ;
#39267 = CARTESIAN_POINT ( 'NONE',  ( 815.1787889125755555, -30.89650538077846065, -343.7953271457877804 ) ) ;
#39268 = CARTESIAN_POINT ( 'NONE',  ( 754.8072714833583632, -340.8164208402376403, 338.1981804954721156 ) ) ;
#39269 = AXIS2_PLACEMENT_3D ( 'NONE', #8221, #22290, #36386 ) ;
#39270 = CARTESIAN_POINT ( 'NONE',  ( 808.5285127195401174, -452.9681489794448339, -336.5948204574517035 ) ) ;
#39271 = DIRECTION ( 'NONE',  ( -0.000000000000000000, 1.000000000000000000, -0.000000000000000000 ) ) ;
#39272 = ORIENTED_EDGE ( 'NONE', *, *, #28615, .T. ) ;
#39273 = CARTESIAN_POINT ( 'NONE',  ( 766.7756240680305382, -62.53286901714199786, 361.5560724626415663 ) ) ;
#39274 = CARTESIAN_POINT ( 'NONE',  ( 804.1009440267234822, -335.4636090269705733, -314.0944755984392600 ) ) ;
#39275 = CARTESIAN_POINT ( 'NONE',  ( 749.2812353651451076, -294.4527844766013800, 323.2262854647983090 ) ) ;
#39276 = CARTESIAN_POINT ( 'NONE',  ( 761.9338519418445230, 9.467130982857780097, 370.4231160770881957 ) ) ;
#39277 = ADVANCED_FACE ( 'NONE', ( #39817 ), #24785, .F. ) ;
#39278 = CARTESIAN_POINT ( 'NONE',  ( 800.9840315886518738, -196.9181544815164386, -354.1144889064786412 ) ) ;
#39279 = CARTESIAN_POINT ( 'NONE',  ( 795.1360043628807261, -164.0891481129655176, -360.2193346964456282 ) ) ;
#39280 = CARTESIAN_POINT ( 'NONE',  ( 801.9419747391806368, -354.4527844766012095, -351.9812246680014027 ) ) ;
#39281 = VERTEX_POINT ( 'NONE', #10703 ) ;
#39282 = CARTESIAN_POINT ( 'NONE',  ( 761.2382568024794409, 8.376221891948691933, -356.9571628226838129 ) ) ;
#39283 = CARTESIAN_POINT ( 'NONE',  ( 758.8095938919642549, -296.0891481129650629, 311.6929314249763365 ) ) ;
#39284 = DIRECTION ( 'NONE',  ( -1.000000000000000000, -0.000000000000000000, -0.000000000000000000 ) ) ;
#39285 = CARTESIAN_POINT ( 'NONE',  ( 756.1348686366196716, -353.2601417444137724, 347.5531968255698416 ) ) ;
#39286 = DIRECTION ( 'NONE',  ( 0.000000000000000000, -0.000000000000000000, -1.000000000000000000 ) ) ;
#39287 = CARTESIAN_POINT ( 'NONE',  ( 798.5707757039680246, -173.4636090269710849, 356.7845633553585003 ) ) ;
#39288 = CARTESIAN_POINT ( 'NONE',  ( 755.3201227861273992, -51.72551174932946338, 345.3687786644892981 ) ) ;
#39289 = EDGE_LOOP ( 'NONE', ( #37515, #22627, #43132, #25163 ) ) ;
#39290 = CARTESIAN_POINT ( 'NONE',  ( 757.7880784355613741, -402.0090635724250205, -312.4576283171834916 ) ) ;
#39291 = VECTOR ( 'NONE', #19563, 1000.000000000000000 ) ;
#39292 = CARTESIAN_POINT ( 'NONE',  ( 745.4481719005789273, -3.725511749329622813, -347.5162901302853697 ) ) ;
#39293 = CARTESIAN_POINT ( 'NONE',  ( 797.8822607201568644, -270.5545181178798657, 370.1134526219340160 ) ) ;
#39294 = CARTESIAN_POINT ( 'NONE',  ( 795.9930595647434757, -219.0783235625960401, 320.7433823573372820 ) ) ;
#39295 = CARTESIAN_POINT ( 'NONE',  ( 774.6312213355099630, -359.3618753856920875, -364.6798772138717482 ) ) ;
#39296 = CARTESIAN_POINT ( 'NONE',  ( 771.1735550268778070, 14.81994279612486309, 316.3353852180827630 ) ) ;
#39297 = FACE_OUTER_BOUND ( 'NONE', #12057, .T. ) ;
#39298 = CARTESIAN_POINT ( 'NONE',  ( 783.0745993439762742, -224.1908817542436623, -365.1016975059196739 ) ) ;
#39299 = CARTESIAN_POINT ( 'NONE',  ( 745.7998596910086917, -29.36187538569318178, 332.5602148656461168 ) ) ;
#39300 = CARTESIAN_POINT ( 'NONE',  ( 767.7687537140311633, -95.90732993114751537, 372.7932403749916830 ) ) ;
#39301 = AXIS2_PLACEMENT_3D ( 'NONE', #35639, #39826, #3787 ) ;
#39302 = CARTESIAN_POINT ( 'NONE',  ( 187.1337867209877857, 62.85347435602256638, -357.4246812887967053 ) ) ;
#39303 = CARTESIAN_POINT ( 'NONE',  ( 810.7187646348534145, -450.4527844766009821, -356.7737145352016341 ) ) ;
#39304 = CARTESIAN_POINT ( 'NONE',  ( 181.1634899080285948, 258.0939999999999941, -206.1189999999954239 ) ) ;
#39305 = CARTESIAN_POINT ( 'NONE',  ( 805.6418435158337843, -389.4636090269704027, 363.8556311672236916 ) ) ;
#39306 = LINE ( 'NONE', #43666, #8798 ) ;
#39307 = CARTESIAN_POINT ( 'NONE',  ( 749.2812353651451076, -318.4527844766014368, 323.2262854647983090 ) ) ;
#39308 = CARTESIAN_POINT ( 'NONE',  ( 754.9967657858570647, -73.54369356751118403, -365.0032342141425374 ) ) ;
#39309 = EDGE_CURVE ( 'NONE', #41960, #19541, #42803, .T. ) ;
#39310 = CARTESIAN_POINT ( 'NONE',  ( 756.3353852180819104, -269.9073299311468190, -331.1735550268788302 ) ) ;
#39311 = DIRECTION ( 'NONE',  ( 0.000000000000000000, 0.000000000000000000, 1.000000000000000000 ) ) ;
#39312 = CARTESIAN_POINT ( 'NONE',  ( 758.0580252608178853, -438.4527844766009821, 328.0187753319985404 ) ) ;
#39313 = CARTESIAN_POINT ( 'NONE',  ( 809.0717654672305343, -76.91815448151683654, -360.1688906516309885 ) ) ;
#39314 = CARTESIAN_POINT ( 'NONE',  ( 755.8398074228967971, -91.44195992623282621, -333.4516893846970333 ) ) ;
#39315 = CARTESIAN_POINT ( 'NONE',  ( 791.1614460488616487, -107.2601417444145824, 373.5763878283158874 ) ) ;
#39316 = CARTESIAN_POINT ( 'NONE',  ( 800.2193346964446619, -402.9982390220555999, 355.1360043628816925 ) ) ;
#39317 = CARTESIAN_POINT ( 'NONE',  ( 795.6651683502461765, -154.7146871989598935, 371.3240766477733814 ) ) ;
#39318 = CARTESIAN_POINT ( 'NONE',  ( 768.0187753319979720, 15.36539734157940629, -318.0580252608186242 ) ) ;
#39320 = ORIENTED_EDGE ( 'NONE', *, *, #15003, .F. ) ;
#39319 = CARTESIAN_POINT ( 'NONE',  ( 787.6308680596127942, -107.2601417444145824, -364.1105419155492768 ) ) ;
#39321 = CARTESIAN_POINT ( 'NONE',  ( 758.0580252608178853, -102.4527844766020337, -328.0187753319985404 ) ) ;
#39322 = CARTESIAN_POINT ( 'NONE',  ( 805.0264073115434940, -414.3510508353227237, -339.4763451958999099 ) ) ;
#39324 = CARTESIAN_POINT ( 'NONE',  ( 774.6312213355098493, -239.3618753856924855, 364.6798772138717482 ) ) ;
#39323 = CARTESIAN_POINT ( 'NONE',  ( 771.1735550268778070, -225.1800572038743269, 316.3353852180827630 ) ) ;
#39325 = VECTOR ( 'NONE', #43328, 1000.000000000000000 ) ;
#39326 = CARTESIAN_POINT ( 'NONE',  ( 759.8311093483677041, -406.1692326535045368, -310.9282345327691814 ) ) ;
#39327 = CARTESIAN_POINT ( 'NONE',  ( -598.8365100919716042, 240.0000000000001705, -199.9999999999899671 ) ) ;
#39328 = ORIENTED_EDGE ( 'NONE', *, *, #28880, .T. ) ;
#39329 = CARTESIAN_POINT ( 'NONE',  ( 771.1735550268778070, -417.1800572038736163, 316.3353852180827630 ) ) ;
#39330 = CARTESIAN_POINT ( 'NONE',  ( 755.2512626584698410, -247.5436935675106724, -315.2512626584710915 ) ) ;
#39331 = ORIENTED_EDGE ( 'NONE', *, *, #12847, .F. ) ;
#39332 = CARTESIAN_POINT ( 'NONE',  ( 763.0537975583475827, -264.4527844766016074, -371.0346526505627480 ) ) ;
#39333 = CARTESIAN_POINT ( 'NONE',  ( 815.2698199232962679, -184.8164208402381234, 342.5225473063383674 ) ) ;
#39334 = CARTESIAN_POINT ( 'NONE',  ( 779.4763451958990572, -272.7363362996981095, 365.0264073115438919 ) ) ;
#39335 = ADVANCED_FACE ( 'NONE', ( #14406 ), #38903, .T. ) ;
#39336 = VERTEX_POINT ( 'NONE', #22226 ) ;
#39337 = CARTESIAN_POINT ( 'NONE',  ( 755.3028492785439312, -87.28179084515316788, -335.9200461376539693 ) ) ;
#39338 = CARTESIAN_POINT ( 'NONE',  ( 815.1787889125755555, -198.8965053807779384, 343.7953271457877804 ) ) ;
#39339 = CARTESIAN_POINT ( 'NONE',  ( 792.1044303154646968, -252.4527844766015789, -317.8323909638837677 ) ) ;
#39340 = ORIENTED_EDGE ( 'NONE', *, *, #36226, .F. ) ;
#39341 = CARTESIAN_POINT ( 'NONE',  ( 755.5713283507202505, -389.3618753856919739, -334.6858677611754729 ) ) ;
#39342 = CARTESIAN_POINT ( 'NONE',  ( 785.3687786644884454, -59.36187538569306810, -315.3201227861279676 ) ) ;
#39343 = CARTESIAN_POINT ( 'NONE',  ( 773.3843516231979720, -229.4419599262323572, 364.4086373105754433 ) ) ;
#39344 = LINE ( 'NONE', #4467, #34395 ) ;
#39345 = DIRECTION ( 'NONE',  ( -0.000000000000000000, 1.000000000000000000, -0.000000000000000000 ) ) ;
#39346 = EDGE_LOOP ( 'NONE', ( #13525, #6366, #17323, #2283 ) ) ;
#39347 = CARTESIAN_POINT ( 'NONE',  ( 792.1044303154645831, -12.45278447660232146, -317.8323909638837677 ) ) ;
#39348 = LINE ( 'NONE', #21782, #36653 ) ;
#39349 = PLANE ( 'NONE',  #16706 ) ;
#39350 = EDGE_LOOP ( 'NONE', ( #12976, #33232 ) ) ;
#39351 = CARTESIAN_POINT ( 'NONE',  ( 804.1009440267234822, -287.4636090269708575, -314.0944755984392600 ) ) ;
#39352 = CARTESIAN_POINT ( 'NONE',  ( 766.4474001241216001, -187.0999726633346825, 307.3154664389482491 ) ) ;
#39354 = CARTESIAN_POINT ( 'NONE',  ( 785.3687786644884454, -251.3618753856923149, -315.3201227861279676 ) ) ;
#39353 = DIRECTION ( 'NONE',  ( 0.000000000000000000, 0.3826834323650836756, 0.9238795325112892920 ) ) ;
#39355 = CARTESIAN_POINT ( 'NONE',  ( 787.5531968255692163, -117.8272453906076151, -316.1348686366205811 ) ) ;
#39356 = EDGE_CURVE ( 'NONE', #18371, #30790, #22632, .T. ) ;
#39357 = CARTESIAN_POINT ( 'NONE',  ( 763.0537975583475827, -24.45278447660229304, 371.0346526505627480 ) ) ;
#39358 = CIRCLE ( 'NONE', #19422, 12.00000000000001066 ) ;
#39359 = DIRECTION ( 'NONE',  ( -0.000000000000000000, 1.000000000000000000, -0.000000000000000000 ) ) ;
#39360 = CARTESIAN_POINT ( 'NONE',  ( 787.5162901302840055, -323.3618753856922581, -305.4481719005793252 ) ) ;
#39361 = DIRECTION ( 'NONE',  ( -8.326672684688676025E-16, -1.000000000000000000, 0.000000000000000000 ) ) ;
#39362 = CARTESIAN_POINT ( 'NONE',  ( 797.6776695296629214, 4.456306432488530866, 357.6776695296636603 ) ) ;
#39363 = VECTOR ( 'NONE', #9904, 1000.000000000000000 ) ;
#39364 = CARTESIAN_POINT ( 'NONE',  ( 811.3240766477731540, -244.3726999360617924, 355.6651683502462902 ) ) ;
#39365 = CARTESIAN_POINT ( 'NONE',  ( 756.1443688327750579, -213.6237781080506011, -314.3581564841659315 ) ) ;
#39366 = CARTESIAN_POINT ( 'NONE',  ( 796.7737145352015204, -212.6346026584198796, 370.7187646348536987 ) ) ;
#39367 = CARTESIAN_POINT ( 'NONE',  ( 771.3260364891663130, 4.354572791210176597, -306.0683387631859773 ) ) ;
#39368 = ADVANCED_FACE ( 'NONE', ( #35404 ), #3775, .F. ) ;
#39369 = CARTESIAN_POINT ( 'NONE',  ( 190.7583438952259485, 394.6698570112193920, -274.9999999999999432 ) ) ;
#39370 = CARTESIAN_POINT ( 'NONE',  ( 797.8594530101008786, -325.5436935675105019, 322.1405469898980982 ) ) ;
#39371 = CARTESIAN_POINT ( 'NONE',  ( 769.0155153010367712, -82.37269993606227558, 362.7791456095907279 ) ) ;
#39372 = CARTESIAN_POINT ( 'NONE',  ( 766.0291762391763086, -82.91815448151682233, 360.7704444035551319 ) ) ;
#39373 = CARTESIAN_POINT ( 'NONE',  ( 797.6776695296629214, -451.5436935675099903, -357.6776695296636603 ) ) ;
#39374 = CYLINDRICAL_SURFACE ( 'NONE', #23258, 20.00000000000001776 ) ;
#39375 = AXIS2_PLACEMENT_3D ( 'NONE', #33189, #37321, #19100 ) ;
#39376 = DIRECTION ( 'NONE',  ( 0.000000000000000000, 0.000000000000000000, 1.000000000000000000 ) ) ;
#39378 = CARTESIAN_POINT ( 'NONE',  ( 755.0636971347428243, -364.2709662947830793, 341.7834795799807353 ) ) ;
#39377 = CARTESIAN_POINT ( 'NONE',  ( 754.8983024940795303, -162.8965053807780521, 336.9254006560228163 ) ) ;
#39379 = ORIENTED_EDGE ( 'NONE', *, *, #9206, .T. ) ;
#39380 = CARTESIAN_POINT ( 'NONE',  ( 788.7366044899766848, -35.90732993114770011, -316.5762568750059813 ) ) ;
#39381 = CARTESIAN_POINT ( 'NONE',  ( 775.9200461376533440, -287.8055962898685038, -315.3028492785443291 ) ) ;
#39382 = UNCERTAINTY_MEASURE_WITH_UNIT (LENGTH_MEASURE( 1.000000000000000082E-05 ), #6539, 'distance_accuracy_value', 'NONE');
#39383 = CARTESIAN_POINT ( 'NONE',  ( 788.8264449731200330, -141.1800572038746395, 363.6646147819171233 ) ) ;
#39384 = CARTESIAN_POINT ( 'NONE',  ( 764.3348316497523456, -310.7146871989593251, -308.6759233522265617 ) ) ;
#39385 = DIRECTION ( 'NONE',  ( 0.000000000000000000, 0.000000000000000000, 1.000000000000000000 ) ) ;
#39386 = CARTESIAN_POINT ( 'NONE',  ( 808.7758568127978833, -436.1692326535044231, 320.0363995740631822 ) ) ;
#39387 = EDGE_CURVE ( 'NONE', #36831, #5978, #10945, .T. ) ;
#39388 = ORIENTED_EDGE ( 'NONE', *, *, #13125, .F. ) ;
#39389 = CARTESIAN_POINT ( 'NONE',  ( 778.2165204200184689, -334.8164208402376403, 364.9363028652563230 ) ) ;
#39390 = EDGE_CURVE ( 'NONE', #17002, #8608, #22013, .T. ) ;
#39391 = CARTESIAN_POINT ( 'NONE',  ( 803.8651313633788504, -77.26014174441466764, -332.4468031744301015 ) ) ;
#39392 = CARTESIAN_POINT ( 'NONE',  ( 797.8594530101008786, -445.5436935675098766, 322.1405469898980982 ) ) ;
#39393 = CARTESIAN_POINT ( 'NONE',  ( 811.0346526505616112, -158.6346026584199933, -323.0537975583477532 ) ) ;
#39394 =( REPRESENTATION_RELATIONSHIP ('NONE','NONE', #39835, #26911 ) REPRESENTATION_RELATIONSHIP_WITH_TRANSFORMATION ( #43577 )SHAPE_REPRESENTATION_RELATIONSHIP( ) );
#39395 = VERTEX_POINT ( 'NONE', #39125 ) ;
#39396 = AXIS2_PLACEMENT_3D ( 'NONE', #42655, #43100, #15392 ) ;
#39397 = CARTESIAN_POINT ( 'NONE',  ( 792.1044303154646968, -156.4527844766018916, -317.8323909638837677 ) ) ;
#39398 = ORIENTED_EDGE ( 'NONE', *, *, #4128, .F. ) ;
#39399 = CARTESIAN_POINT ( 'NONE',  ( 802.5472867521000353, -412.3726999360612808, -350.8726784830461156 ) ) ;
#39400 = CARTESIAN_POINT ( 'NONE',  ( 793.0897708529556667, -462.5545181178792973, 361.3366627262616362 ) ) ;
#39401 = CARTESIAN_POINT ( 'NONE',  ( 754.9967657858570647, -217.5436935675107293, 365.0032342141425374 ) ) ;
#39402 = CARTESIAN_POINT ( 'NONE',  ( 786.6156483768007774, -121.4419599262327267, 315.5913626894246136 ) ) ;
#39405 = CARTESIAN_POINT ( 'NONE',  ( 758.0141637701419768, -375.0783235625955285, 367.2620300519063790 ) ) ;
#39404 = FACE_OUTER_BOUND ( 'NONE', #17737, .T. ) ;
#39403 = FACE_OUTER_BOUND ( 'NONE', #12777, .T. ) ;
#39406 = ORIENTED_EDGE ( 'NONE', *, *, #22762, .T. ) ;
#39407 = CARTESIAN_POINT ( 'NONE',  ( 786.5483106153019435, -391.6454272087885897, -364.1601925771022366 ) ) ;
#39408 = CYLINDRICAL_SURFACE ( 'NONE', #5613, 6.118999999999985562 ) ;
#39409 = CARTESIAN_POINT ( 'NONE',  ( 807.2620300519052989, -168.0090635724256458, -318.0141637701419768 ) ) ;
#39410 = CARTESIAN_POINT ( 'NONE',  ( 795.8262568251477660, -70.37269993606230400, 308.3538107759623585 ) ) ;
#39411 = VECTOR ( 'NONE', #15998, 999.9999999999998863 ) ;
#39413 = CARTESIAN_POINT ( 'NONE',  ( 919.9999999999993179, 154.9999999999998863, 360.0000000000000000 ) ) ;
#39412 = DIRECTION ( 'NONE',  ( -1.000000000000000000, -0.000000000000000000, 0.000000000000000000 ) ) ;
#39414 = ADVANCED_FACE ( 'NONE', ( #983 ), #18101, .F. ) ;
#39415 = CARTESIAN_POINT ( 'NONE',  ( 790.8726784830453198, -322.7146871989593819, -362.5472867521010585 ) ) ;
#39416 = CARTESIAN_POINT ( 'NONE',  ( 759.7806653035534055, -438.9982390220553157, -324.8639956371180801 ) ) ;
#39417 = CARTESIAN_POINT ( 'NONE',  ( 783.7953271457878373, -176.1908817542438328, -375.1787889125761239 ) ) ;
#39418 = DIRECTION ( 'NONE',  ( 0.000000000000000000, 0.000000000000000000, 1.000000000000000000 ) ) ;
#39419 = DIRECTION ( 'NONE',  ( -1.000000000000000000, -0.000000000000000000, 0.000000000000000000 ) ) ;
#39420 = CARTESIAN_POINT ( 'NONE',  ( 766.0291762391763086, -370.9181544815159555, 360.7704444035551319 ) ) ;
#39421 = EDGE_CURVE ( 'NONE', #6074, #3415, #36321, .T. ) ;
#39422 = CARTESIAN_POINT ( 'NONE',  ( 750.9282345327678740, -352.9181544815159555, 319.8311093483690115 ) ) ;
#39423 = CARTESIAN_POINT ( 'NONE',  ( 800.9747183278959710, -204.9982390220562820, -311.9810565676471583 ) ) ;
#39424 = DIRECTION ( 'NONE',  ( 0.000000000000000000, 0.000000000000000000, -1.000000000000000000 ) ) ;
#39425 = CARTESIAN_POINT ( 'NONE',  ( 759.7806653035534055, -30.99823902205680071, -324.8639956371180801 ) ) ;
#39426 = CARTESIAN_POINT ( 'NONE',  ( 745.1792804349281596, -134.1908817542439181, 343.7566961878542884 ) ) ;
#39427 = CARTESIAN_POINT ( 'NONE',  ( 803.8556311672234642, -105.6237781080509421, -365.6418435158340117 ) ) ;
#39428 = CARTESIAN_POINT ( 'NONE',  ( 749.2812353651451076, -102.4527844766020337, 323.2262854647983090 ) ) ;
#39429 = CARTESIAN_POINT ( 'NONE',  ( 755.2512626584698410, -343.5436935675103314, -315.2512626584710915 ) ) ;
#39430 = EDGE_CURVE ( 'NONE', #9209, #18435, #28724, .T. ) ;
#39431 = EDGE_CURVE ( 'NONE', #34950, #15624, #18340, .T. ) ;
#39432 = CARTESIAN_POINT ( 'NONE',  ( 769.9999999999992042, 205.0000000000000568, -339.9999999999999432 ) ) ;
#39433 = CARTESIAN_POINT ( 'NONE',  ( 794.9999999999993179, 197.3292319334027241, 273.4704985657796783 ) ) ;
#39434 = CARTESIAN_POINT ( 'NONE',  ( 794.9819416627830151, -204.9982390220562820, 319.9864689768909898 ) ) ;
#39435 =( GEOMETRIC_REPRESENTATION_CONTEXT ( 3 ) GLOBAL_UNCERTAINTY_ASSIGNED_CONTEXT ( ( #29649 ) ) GLOBAL_UNIT_ASSIGNED_CONTEXT ( ( #16477, #40520, #9086 ) ) REPRESENTATION_CONTEXT ( 'NONE', 'WORKASPACE' ) );
#39436 = AXIS2_PLACEMENT_3D ( 'NONE', #31454, #6971, #31671 ) ;
#39437 = CARTESIAN_POINT ( 'NONE',  ( 799.9636004259356241, -454.9181544815156713, 311.2241431872006956 ) ) ;
#39438 = CARTESIAN_POINT ( 'NONE',  ( 795.6651683502461765, -394.7146871989591546, -371.3240766477733814 ) ) ;
#39439 = CARTESIAN_POINT ( 'NONE',  ( 792.3570229623688874, -405.1800572038737300, -373.1304606946836202 ) ) ;
#39440 = LINE ( 'NONE', #18871, #18071 ) ;
#39441 = CARTESIAN_POINT ( 'NONE',  ( 759.8311093483677041, -22.16923265350575889, 310.9282345327691814 ) ) ;
#39442 = ORIENTED_EDGE ( 'NONE', *, *, #30060, .F. ) ;
#39443 = CARTESIAN_POINT ( 'NONE',  ( 756.7813123517142913, -187.9874144716870603, -329.9779781133712504 ) ) ;
#39444 = CARTESIAN_POINT ( 'NONE',  ( 771.2633955100217236, -119.9073299311474443, -363.4237431249939618 ) ) ;
#39445 = CARTESIAN_POINT ( 'NONE',  ( 804.4286716492782716, -41.36187538569314626, 345.3141322388244703 ) ) ;
#39446 = CARTESIAN_POINT ( 'NONE',  ( 766.5853460496234675, -205.9874144716870035, -372.3518521366060554 ) ) ;
#39447 = CARTESIAN_POINT ( 'NONE',  ( 771.2368401574024119, -301.4419599262320730, 374.2805881961240857 ) ) ;
#39448 = CARTESIAN_POINT ( 'NONE',  ( 767.8955696845334842, -168.4527844766018347, 362.1676090361161755 ) ) ;
#39449 = EDGE_LOOP ( 'NONE', ( #32463, #709, #2466, #2612 ) ) ;
#39450 = VECTOR ( 'NONE', #25394, 1000.000000000000000 ) ;
#39451 = CARTESIAN_POINT ( 'NONE',  ( 778.1981804954714335, -322.2709662947830225, 314.8072714833589885 ) ) ;
#39452 = AXIS2_PLACEMENT_3D ( 'NONE', #16065, #32955, #44007 ) ;
#39453 = CARTESIAN_POINT ( 'NONE',  ( 747.2067596250078623, -51.18005720387493085, -352.2312462859687230 ) ) ;
#39454 = CARTESIAN_POINT ( 'NONE',  ( 782.5225473063383106, -94.27096629478387513, 375.2698199232970637 ) ) ;
#39455 = ORIENTED_EDGE ( 'NONE', *, *, #114, .F. ) ;
#39456 = CARTESIAN_POINT ( 'NONE',  ( 811.3240766477731540, -460.3726999360611103, -355.6651683502462902 ) ) ;
#39457 = EDGE_LOOP ( 'NONE', ( #36494, #44371, #9908, #43280 ) ) ;
#39458 = APPLICATION_PROTOCOL_DEFINITION ( 'draft international standard', 'automotive_design', 1998, #19885 ) ;
#39460 = CARTESIAN_POINT ( 'NONE',  ( 802.9823548866075953, -361.0999726633341425, 330.0799878456151077 ) ) ;
#39459 = CARTESIAN_POINT ( 'NONE',  ( 801.9419747391806368, -42.45278447660223264, 351.9812246680014027 ) ) ;
#39461 = CARTESIAN_POINT ( 'NONE',  ( 797.6776695296629214, -283.5436935675105019, -357.6776695296636603 ) ) ;
#39462 = CARTESIAN_POINT ( 'NONE',  ( 796.9462024416508257, -396.4527844766010958, 308.9653473494370246 ) ) ;
#39463 = CARTESIAN_POINT ( 'NONE',  ( 766.5853460496234675, -61.98741447168745822, 372.3518521366060554 ) ) ;
#39464 = CARTESIAN_POINT ( 'NONE',  ( 793.9708237608222134, -286.9181544815161828, -319.2295555964448681 ) ) ;
#39465 = CARTESIAN_POINT ( 'NONE',  ( 785.3687786644884454, -275.3618753856923149, -315.3201227861279676 ) ) ;
#39466 = DIRECTION ( 'NONE',  ( 0.000000000000000000, 0.7372773368101328550, -0.6755902076156506952 ) ) ;
#39467 = CARTESIAN_POINT ( 'NONE',  ( 803.4237431249931660, -111.1800572038747532, -331.2633955100225194 ) ) ;
#39468 = VECTOR ( 'NONE', #41808, 1000.000000000000000 ) ;
#39469 = CYLINDRICAL_SURFACE ( 'NONE', #4827, 7.999999999999896083 ) ;
#39470 = EDGE_LOOP ( 'NONE', ( #22553, #14769, #28863, #9454 ) ) ;
#39471 = CARTESIAN_POINT ( 'NONE',  ( 745.7998596910086917, -389.3618753856919739, 332.5602148656461168 ) ) ;
#39472 = AXIS2_PLACEMENT_3D ( 'NONE', #4016, #39601, #7957 ) ;
#39474 = DIRECTION ( 'NONE',  ( -0.000000000000000000, 1.000000000000000000, -0.000000000000000000 ) ) ;
#39473 = CARTESIAN_POINT ( 'NONE',  ( 799.9999999999993179, -462.9681489794448339, 309.9999999999998863 ) ) ;
#39475 = EDGE_CURVE ( 'NONE', #5289, #42219, #39590, .T. ) ;
#39476 = CARTESIAN_POINT ( 'NONE',  ( 815.3608509340175488, -74.73633629969866377, -341.2497674668889545 ) ) ;
#39477 = DIRECTION ( 'NONE',  ( 1.000000000000000000, 0.000000000000000000, 0.000000000000000000 ) ) ;
#39478 = DIRECTION ( 'NONE',  ( -0.000000000000000000, 1.000000000000000000, -0.000000000000000000 ) ) ;
#39479 = CARTESIAN_POINT ( 'NONE',  ( 755.3028492785439312, -279.2817908451526137, 335.9200461376539693 ) ) ;
#39480 = CARTESIAN_POINT ( 'NONE',  ( 759.9864689768902508, -170.0891481129654608, 354.9819416627836404 ) ) ;
#39481 = ORIENTED_EDGE ( 'NONE', *, *, #40552, .T. ) ;
#39482 = CARTESIAN_POINT ( 'NONE',  ( 763.0428371773158460, -35.46360902697151829, -358.7617431975195359 ) ) ;
#39483 = CARTESIAN_POINT ( 'NONE',  ( 766.7756240680305382, -326.5328690171411381, 361.5560724626415663 ) ) ;
#39484 = LINE ( 'NONE', #21679, #18242 ) ;
#39485 = AXIS2_PLACEMENT_3D ( 'NONE', #11076, #18689, #1125 ) ;
#39486 = CARTESIAN_POINT ( 'NONE',  ( 804.1009440267234822, -47.46360902697148987, 314.0944755984392600 ) ) ;
#39487 = CARTESIAN_POINT ( 'NONE',  ( 758.8095938919642549, -248.0891481129651481, -311.6929314249763365 ) ) ;
#39488 = EDGE_CURVE ( 'NONE', #26042, #7675, #28945, .T. ) ;
#39489 = AXIS2_PLACEMENT_3D ( 'NONE', #17443, #35428, #18126 ) ;
#39490 = AXIS2_PLACEMENT_3D ( 'NONE', #37052, #41609, #5404 ) ;
#39491 = CARTESIAN_POINT ( 'NONE',  ( 754.9967657858570647, -193.5436935675108714, 365.0032342141425374 ) ) ;
#39492 = CARTESIAN_POINT ( 'NONE',  ( 800.0135310231082713, -110.0891481129656597, 325.0180583372163028 ) ) ;
#39493 = DIRECTION ( 'NONE',  ( 1.000000000000000000, 0.000000000000000000, 0.000000000000000000 ) ) ;
#39494 = CARTESIAN_POINT ( 'NONE',  ( 811.6461892240364477, -292.7146871989594956, -324.1737431748509835 ) ) ;
#39495 = CARTESIAN_POINT ( 'NONE',  ( 802.2119215644370342, -462.0090635724247932, 367.5423716828165084 ) ) ;
#39496 = CARTESIAN_POINT ( 'NONE',  ( 800.9747183278959710, -300.9982390220559409, -311.9810565676471583 ) ) ;
#39497 = DIRECTION ( 'NONE',  ( -1.000000000000000000, -4.625929269271485914E-16, -0.000000000000000000 ) ) ;
#39498 = CARTESIAN_POINT ( 'NONE',  ( 754.9735926884551418, -354.3510508353228943, 340.5236548041000333 ) ) ;
#39499 = DIRECTION ( 'NONE',  ( -1.880165489482579047E-16, -1.000000000000000000, -0.000000000000000000 ) ) ;
#39500 = CARTESIAN_POINT ( 'NONE',  ( 800.0135310231082713, -422.0891481129647218, -325.0180583372163028 ) ) ;
#39501 = VECTOR ( 'NONE', #948, 1000.000000000000000 ) ;
#39502 = CARTESIAN_POINT ( 'NONE',  ( 756.7813123517142913, -43.98741447168752217, 329.9779781133712504 ) ) ;
#39503 = CARTESIAN_POINT ( 'NONE',  ( 757.8323909638827445, -194.6346026584198796, -352.1044303154654358 ) ) ;
#39504 = CIRCLE ( 'NONE', #41697, 6.118999999999985562 ) ;
#39505 = CARTESIAN_POINT ( 'NONE',  ( 788.7631598425961101, -73.44195992623286884, -305.7194118038759143 ) ) ;
#39506 = CARTESIAN_POINT ( 'NONE',  ( 748.3538107759620743, -208.7146871989596946, 355.8262568251490165 ) ) ;
#39507 = CARTESIAN_POINT ( 'NONE',  ( 774.6312213355098493, -47.36187538569312494, 364.6798772138717482 ) ) ;
#39508 = CIRCLE ( 'NONE', #25469, 30.00000000000002842 ) ;
#39509 = ORIENTED_EDGE ( 'NONE', *, *, #6873, .F. ) ;
#39510 = CARTESIAN_POINT ( 'NONE',  ( 805.1016975059191054, -246.8965053807777679, -343.0745993439771837 ) ) ;
#39511 = CARTESIAN_POINT ( 'NONE',  ( 774.6858677611749044, -201.7255117493290015, 315.5713283507209894 ) ) ;
#39512 = CARTESIAN_POINT ( 'NONE',  ( 746.0683387631852383, -43.44195992623296831, -331.3260364891676204 ) ) ;
#39513 = CARTESIAN_POINT ( 'NONE',  ( 785.3687786644885591, -347.3618753856922012, 315.3201227861280813 ) ) ;
#39514 = VECTOR ( 'NONE', #385, 999.9999999999998863 ) ;
#39515 = CARTESIAN_POINT ( 'NONE',  ( 795.1526350630804245, -452.9681489794450044, -359.9976132353968410 ) ) ;
#39516 = CARTESIAN_POINT ( 'NONE',  ( 786.4999999999993179, -110.5936016518799221, 750.6326042729449455 ) ) ;
#39517 = VERTEX_POINT ( 'NONE', #8379 ) ;
#39518 = CARTESIAN_POINT ( 'NONE',  ( 766.7756240680305382, -38.53286901714206891, 361.5560724626415663 ) ) ;
#39519 = CARTESIAN_POINT ( 'NONE',  ( 809.0717654672305343, -340.9181544815160123, -360.1688906516309885 ) ) ;
#39520 = AXIS2_PLACEMENT_3D ( 'NONE', #3357, #2665, #13758 ) ;
#39521 = CIRCLE ( 'NONE', #23289, 6.118999999999985562 ) ;
#39522 = CARTESIAN_POINT ( 'NONE',  ( 747.2067596250078623, -291.1800572038741848, 352.2312462859687230 ) ) ;
#39523 = CARTESIAN_POINT ( 'NONE',  ( 813.9316612368132837, 16.55804007376685050, 348.6739635108323228 ) ) ;
#39524 = CARTESIAN_POINT ( 'NONE',  ( 757.0176451133909268, -181.0999726633347109, -349.9200121543848354 ) ) ;
#39525 = CARTESIAN_POINT ( 'NONE',  ( 797.6776695296629214, -187.5436935675108430, -357.6776695296636603 ) ) ;
#39526 = CARTESIAN_POINT ( 'NONE',  ( 791.9812246680005501, -332.6346026584195101, -361.9419747391813189 ) ) ;
#39527 = ORIENTED_EDGE ( 'NONE', *, *, #18766, .F. ) ;
#39528 = CARTESIAN_POINT ( 'NONE',  ( 786.6156483768007774, 22.55804007376682918, -315.5913626894246136 ) ) ;
#39529 = CARTESIAN_POINT ( 'NONE',  ( 796.9462024416508257, -276.4527844766013800, 308.9653473494370246 ) ) ;
#39530 = CARTESIAN_POINT ( 'NONE',  ( 779.9999999999992042, -452.9681489794448339, 350.0000000000000000 ) ) ;
#39531 = CARTESIAN_POINT ( 'NONE',  ( 755.0488828828309806, -353.8055962898683333, 344.1219089521771934 ) ) ;
#39532 = DIRECTION ( 'NONE',  ( -1.880165489482579047E-16, -1.000000000000000000, -0.000000000000000000 ) ) ;
#39533 = CARTESIAN_POINT ( 'NONE',  ( 796.9571628226829034, -143.4636090269711701, 321.2382568024804641 ) ) ;
#39534 = CARTESIAN_POINT ( 'NONE',  ( 791.9812246680005501, -44.63460265842040542, 361.9419747391813189 ) ) ;
#39535 = ORIENTED_EDGE ( 'NONE', *, *, #7772, .F. ) ;
#39536 = CARTESIAN_POINT ( 'NONE',  ( 747.6481478633932056, -397.0999726633340288, -353.4146539503763620 ) ) ;
#39537 = AXIS2_PLACEMENT_3D ( 'NONE', #17652, #35632, #31263 ) ;
#39538 = CARTESIAN_POINT ( 'NONE',  ( 814.9108240113580450, 7.729033705215793582, -337.5031285880265273 ) ) ;
#39539 = CARTESIAN_POINT ( 'NONE',  ( 809.0717654672305343, -268.9181544815162397, 360.1688906516309885 ) ) ;
#39540 = CARTESIAN_POINT ( 'NONE',  ( 755.8398074228967971, -235.4419599262323857, 333.4516893846970333 ) ) ;
#39541 = VECTOR ( 'NONE', #7998, 1000.000000000000000 ) ;
#39542 = CARTESIAN_POINT ( 'NONE',  ( 788.7366044899766848, -347.9073299311467053, -316.5762568750059813 ) ) ;
#39543 = CARTESIAN_POINT ( 'NONE',  ( -39.63011601220123481, -544.8427095258973623, -350.0000000000000000 ) ) ;
#39544 = CARTESIAN_POINT ( 'NONE',  ( 757.8323909638827445, -2.634602658420536869, 352.1044303154654358 ) ) ;
#39545 = SURFACE_STYLE_FILL_AREA ( #18734 ) ;
#39546 = CARTESIAN_POINT ( 'NONE',  ( 775.8780910478218402, -249.2817908451526421, -364.9511171171680530 ) ) ;
#39547 = VECTOR ( 'NONE', #32002, 1000.000000000000000 ) ;
#39548 = CARTESIAN_POINT ( 'NONE',  ( 763.2262854647970016, -32.63460265842044095, 309.2812353651462445 ) ) ;
#39549 = CARTESIAN_POINT ( 'NONE',  ( 782.5225473063381969, -94.27096629478386092, 375.2698199232970637 ) ) ;
#39550 = DIRECTION ( 'NONE',  ( 0.000000000000000000, 0.7071067811865526798, 0.7071067811865423547 ) ) ;
#39551 = DIRECTION ( 'NONE',  ( 0.000000000000000000, -0.7651688349527138167, -0.6438296778008192334 ) ) ;
#39552 = DIRECTION ( 'NONE',  ( 1.000000000000000000, 0.000000000000000000, 0.000000000000000000 ) ) ;
#39553 = CIRCLE ( 'NONE', #18869, 2.749999999999919176 ) ;
#39554 = CARTESIAN_POINT ( 'NONE',  ( 776.2046728542105711, -380.1908817542431507, 304.8212110874238761 ) ) ;
#39555 = CARTESIAN_POINT ( 'NONE',  ( -809.9999999999993179, -512.9681489794448908, -339.9999999999999432 ) ) ;
#39556 = CARTESIAN_POINT ( 'NONE',  ( 787.5162901302840055, -323.3618753856923149, 305.4481719005792684 ) ) ;
#39557 = CARTESIAN_POINT ( 'NONE',  ( 801.9419747391806368, -306.4527844766013800, -351.9812246680014027 ) ) ;
#39558 = FACE_OUTER_BOUND ( 'NONE', #33468, .T. ) ;
#39559 = CARTESIAN_POINT ( 'NONE',  ( 805.1927285166397041, -424.8164208402372992, 341.8018195045277707 ) ) ;
#39560 = CARTESIAN_POINT ( 'NONE',  ( 802.5472867521000353, -196.3726999360619061, 350.8726784830461156 ) ) ;
#39561 = CARTESIAN_POINT ( 'NONE',  ( 760.0363995740630116, -58.91815448151690759, -368.7758568127991907 ) ) ;
#39562 = CARTESIAN_POINT ( 'NONE',  ( 766.7756240680305382, -86.53286901714194812, -361.5560724626415663 ) ) ;
#39563 = CARTESIAN_POINT ( 'NONE',  ( 752.4576283171824116, -93.07832356259645223, 317.7880784355627952 ) ) ;
#39564 = CARTESIAN_POINT ( 'NONE',  ( 774.6858677611749044, -441.7255117493282910, 315.5713283507209894 ) ) ;
#39565 = CARTESIAN_POINT ( 'NONE',  ( 815.0009284576459549, -150.3510508353235480, 338.7629533639073429 ) ) ;
#39566 = CARTESIAN_POINT ( 'NONE',  ( 788.7366044899766848, 12.09267006885214180, -316.5762568750059813 ) ) ;
#39568 = VERTEX_POINT ( 'NONE', #40026 ) ;
#39567 = CARTESIAN_POINT ( 'NONE',  ( 756.1348686366196716, -137.2601417444144829, -347.5531968255698416 ) ) ;
#39569 = CARTESIAN_POINT ( 'NONE',  ( 792.1044303154645831, -108.4527844766019911, -317.8323909638837677 ) ) ;
#39570 = CARTESIAN_POINT ( 'NONE',  ( 801.3366627262608972, -392.5328690171409107, -353.0897708529566899 ) ) ;
#39572 = CARTESIAN_POINT ( 'NONE',  ( 754.8072714833583632, -220.8164208402380098, 338.1981804954721156 ) ) ;
#39571 = CARTESIAN_POINT ( 'NONE',  ( 762.3223304703356007, -271.5436935675106156, 322.3223304703362828 ) ) ;
#39573 = CYLINDRICAL_SURFACE ( 'NONE', #3530, 9.999999999999980460 ) ;
#39574 = EDGE_LOOP ( 'NONE', ( #37202, #6424, #32922, #19131 ) ) ;
#39575 = CARTESIAN_POINT ( 'NONE',  ( 778.2165204200184689, -430.8164208402374129, 364.9363028652563230 ) ) ;
#39576 = ORIENTED_EDGE ( 'NONE', *, *, #6649, .T. ) ;
#39577 = CIRCLE ( 'NONE', #15242, 2.749999999999919176 ) ;
#39578 = CARTESIAN_POINT ( 'NONE',  ( 746.8695393053151292, -173.9073299311472454, 327.6429770376306578 ) ) ;
#39579 = CARTESIAN_POINT ( 'NONE',  ( 754.7162404726377645, -254.7363362996981095, 339.4709603349214717 ) ) ;
#39580 = ORIENTED_EDGE ( 'NONE', *, *, #8079, .T. ) ;
#39581 = CARTESIAN_POINT ( 'NONE',  ( 769.9779781133707957, -91.09997266333496668, -316.7813123517150871 ) ) ;
#39582 = CARTESIAN_POINT ( 'NONE',  ( 756.1443688327750579, -213.6237781080506011, 314.3581564841659315 ) ) ;
#39583 = CARTESIAN_POINT ( 'NONE',  ( 785.3687786644885591, -251.3618753856923718, -315.3201227861280813 ) ) ;
#39584 = EDGE_CURVE ( 'NONE', #32411, #12435, #30287, .T. ) ;
#39585 = VERTEX_POINT ( 'NONE', #33100 ) ;
#39586 = CARTESIAN_POINT ( 'NONE',  ( 788.7366044899766848, -395.9073299311465348, -316.5762568750059813 ) ) ;
#39587 = CARTESIAN_POINT ( 'NONE',  ( 762.3223304703356007, -55.54369356751127640, -322.3223304703362828 ) ) ;
#39588 = CARTESIAN_POINT ( 'NONE',  ( 787.6308680596127942, -251.2601417444141134, 364.1105419155492768 ) ) ;
#39589 = CARTESIAN_POINT ( 'NONE',  ( -809.9999999999993179, -512.9681489794448908, -329.9999999999999432 ) ) ;
#39590 = LINE ( 'NONE', #29174, #34444 ) ;
#39591 = VECTOR ( 'NONE', #44798, 1000.000000000000000 ) ;
#39592 = CARTESIAN_POINT ( 'NONE',  ( 791.9812246680005501, -20.63460265842048003, -361.9419747391813189 ) ) ;
#39593 = DIRECTION ( 'NONE',  ( -0.000000000000000000, 1.000000000000000000, -0.000000000000000000 ) ) ;
#39594 = ORIENTED_EDGE ( 'NONE', *, *, #25287, .T. ) ;
#39595 = CARTESIAN_POINT ( 'NONE',  ( 744.6391490659812007, -302.7363362996979959, -338.7502325331110455 ) ) ;
#39596 = CARTESIAN_POINT ( 'NONE',  ( 807.2620300519052989, -168.0090635724256458, 318.0141637701419768 ) ) ;
#39598 = CARTESIAN_POINT ( 'NONE',  ( 757.8323909638827445, -266.6346026584197375, -352.1044303154654358 ) ) ;
#39597 = DIRECTION ( 'NONE',  ( -1.000000000000000000, -0.000000000000000000, -0.000000000000000000 ) ) ;
#39599 = FACE_BOUND ( 'NONE', #27214, .T. ) ;
#39600 = CARTESIAN_POINT ( 'NONE',  ( 799.2566176426618085, -144.0090635724257027, -324.0069404352559559 ) ) ;
#39601 = DIRECTION ( 'NONE',  ( 0.000000000000000000, 0.000000000000000000, 1.000000000000000000 ) ) ;
#39602 = CARTESIAN_POINT ( 'NONE',  ( 761.9338519418445230, -14.53286901714214707, -370.4231160770881957 ) ) ;
#39603 = CARTESIAN_POINT ( 'NONE',  ( 805.0032342141413437, -349.5436935675103314, -314.9967657858572352 ) ) ;
#39604 = DIRECTION ( 'NONE',  ( 0.000000000000000000, -1.000000000000000000, 0.000000000000000000 ) ) ;
#39605 = CARTESIAN_POINT ( 'NONE',  ( 778.2165204200184689, -22.81642084023865280, 364.9363028652563230 ) ) ;
#39606 = CARTESIAN_POINT ( 'NONE',  ( 804.1009440267234822, -287.4636090269708575, 314.0944755984392600 ) ) ;
#39607 = CARTESIAN_POINT ( 'NONE',  ( 803.8556311672234642, -249.6237781080505158, -365.6418435158340117 ) ) ;
#39608 = CARTESIAN_POINT ( 'NONE',  ( 777.4774526936600978, -226.2709662947834204, 304.7301800767027657 ) ) ;
#39609 = CARTESIAN_POINT ( 'NONE',  ( 756.1443688327750579, -429.6237781080499190, -314.3581564841659315 ) ) ;
#39610 = AXIS2_PLACEMENT_3D ( 'NONE', #8558, #19172, #29785 ) ;
#39611 = CARTESIAN_POINT ( 'NONE',  ( -879.9999999999992042, 240.0000000000000853, -360.0000000000000000 ) ) ;
#39612 = ORIENTED_EDGE ( 'NONE', *, *, #19077, .F. ) ;
#39613 = CARTESIAN_POINT ( 'NONE',  ( 755.3201227861273992, -315.7255117493286320, 345.3687786644892981 ) ) ;
#39614 = VECTOR ( 'NONE', #33654, 1000.000000000000000 ) ;
#39615 = CARTESIAN_POINT ( 'NONE',  ( 801.5560724626406000, -96.55451811788039151, 326.7756240680316182 ) ) ;
#39616 = CARTESIAN_POINT ( 'NONE',  ( 802.7791456095903868, 19.28531280103956647, -329.0155153010375102 ) ) ;
#39617 = VECTOR ( 'NONE', #18558, 1000.000000000000000 ) ;
#39618 = DIRECTION ( 'NONE',  ( 0.000000000000000000, 0.3826834323650838421, 0.9238795325112891810 ) ) ;
#39619 = LINE ( 'NONE', #18812, #1178 ) ;
#39621 = CARTESIAN_POINT ( 'NONE',  ( 795.1360043628807261, -356.0891481129647218, 360.2193346964456282 ) ) ;
#39620 = CARTESIAN_POINT ( 'NONE',  ( 775.9200461376533440, -143.8055962898690154, 315.3028492785443291 ) ) ;
#39622 = VERTEX_POINT ( 'NONE', #29842 ) ;
#39623 = CIRCLE ( 'NONE', #30762, 20.00000000000001776 ) ;
#39624 = CARTESIAN_POINT ( 'NONE',  ( 759.2295555964440155, -304.1692326535048210, -353.9708237608231229 ) ) ;
#39625 = CARTESIAN_POINT ( 'NONE',  ( 755.3201227861273992, -147.7255117493291152, 345.3687786644892981 ) ) ;
#39626 = CARTESIAN_POINT ( 'NONE',  ( 783.7566961878529810, -312.8965053807775689, -305.1792804349288417 ) ) ;
#39627 = DIRECTION ( 'NONE',  ( 0.000000000000000000, 0.000000000000000000, -1.000000000000000000 ) ) ;
#39628 = CARTESIAN_POINT ( 'NONE',  ( 815.0009284576459549, -438.3510508353226669, 338.7629533639073429 ) ) ;
#39629 = EDGE_LOOP ( 'NONE', ( #17045, #26417, #26298, #18490, #25751, #38754, #21487, #39768, #25178, #6415, #43516, #10243 ) ) ;
#39630 = CARTESIAN_POINT ( 'NONE',  ( 778.1981804954714335, -322.2709662947830225, 314.8072714833589885 ) ) ;
#39631 = CARTESIAN_POINT ( 'NONE',  ( 763.2154366446407039, -93.62377810805098477, -321.4292242960311228 ) ) ;
#39632 = CARTESIAN_POINT ( 'NONE',  ( 801.9419747391806368, -426.4527844766010389, 351.9812246680014027 ) ) ;
#39633 = EDGE_CURVE ( 'NONE', #29759, #14400, #3461, .T. ) ;
#39634 = CARTESIAN_POINT ( 'NONE',  ( 792.2312462859673587, -131.9073299311473875, -307.2067596250082602 ) ) ;
#39635 = ORIENTED_EDGE ( 'NONE', *, *, #5821, .T. ) ;
#39636 = CARTESIAN_POINT ( 'NONE',  ( 768.0187753319979720, -128.6346026584201354, -318.0580252608186242 ) ) ;
#39637 = ORIENTED_EDGE ( 'NONE', *, *, #38258, .F. ) ;
#39638 = CIRCLE ( 'NONE', #1270, 2.749999999999863665 ) ;
#39639 = CARTESIAN_POINT ( 'NONE',  ( 755.5913626894240451, -421.6454272087885329, -346.6156483768012890 ) ) ;
#39640 = CARTESIAN_POINT ( 'NONE',  ( 804.4286716492782716, 6.638124614306706306, 345.3141322388244703 ) ) ;
#39641 = CARTESIAN_POINT ( 'NONE',  ( 813.1304606946830518, -233.9073299311470180, 352.3570229623690580 ) ) ;
#39642 = CARTESIAN_POINT ( 'NONE',  ( 800.7704444035546203, -172.1692326535052757, 326.0291762391768771 ) ) ;
#39645 = CARTESIAN_POINT ( 'NONE',  ( 759.8311093483677041, -382.1692326535045936, 310.9282345327691814 ) ) ;
#39644 = FACE_OUTER_BOUND ( 'NONE', #32166, .T. ) ;
#39643 = LINE ( 'NONE', #36153, #3404 ) ;
#39646 = EDGE_CURVE ( 'NONE', #18435, #44320, #2119, .T. ) ;
#39647 = VERTEX_POINT ( 'NONE', #36992 ) ;
#39648 = CARTESIAN_POINT ( 'NONE',  ( 757.0176451133909268, -397.0999726633340288, -349.9200121543848354 ) ) ;
#39649 = DIRECTION ( 'NONE',  ( 1.000000000000000000, 4.625929269271485914E-16, 0.000000000000000000 ) ) ;
#39650 = CARTESIAN_POINT ( 'NONE',  ( 807.2620300519052989, -216.0090635724255037, -318.0141637701419768 ) ) ;
#39651 = CARTESIAN_POINT ( 'NONE',  ( 815.3608509340175488, -74.73633629969866377, 341.2497674668889545 ) ) ;
#39652 = AXIS2_PLACEMENT_3D ( 'NONE', #11427, #42839, #39385 ) ;
#39654 = DIRECTION ( 'NONE',  ( 1.892425610156518354E-16, 1.000000000000000000, -0.000000000000000000 ) ) ;
#39653 = DIRECTION ( 'NONE',  ( 0.000000000000000000, 0.000000000000000000, 1.000000000000000000 ) ) ;
#39655 = CARTESIAN_POINT ( 'NONE',  ( 756.7813123517142913, -331.9874144716865203, -329.9779781133712504 ) ) ;
#39656 = CARTESIAN_POINT ( 'NONE',  ( 115.7583438952258774, -600.0000000000000000, -244.9999999999999716 ) ) ;
#39657 = CARTESIAN_POINT ( 'NONE',  ( 814.2805881961230625, -193.6454272087891582, -331.2368401574024119 ) ) ;
#39658 = FACE_OUTER_BOUND ( 'NONE', #29392, .T. ) ;
#39659 = DIRECTION ( 'NONE',  ( 0.7071067811865753283, 0.000000000000000000, -0.7071067811865198172 ) ) ;
#39660 = VECTOR ( 'NONE', #29461, 1000.000000000000000 ) ;
#39661 = CARTESIAN_POINT ( 'NONE',  ( 766.9102291470427417, -402.5545181178795247, 318.6633372737382501 ) ) ;
#39662 = CARTESIAN_POINT ( 'NONE',  ( 796.9462024416508257, -228.4527844766016074, -308.9653473494370246 ) ) ;
#39663 = ADVANCED_FACE ( 'NONE', ( #1215 ), #43477, .T. ) ;
#39664 = DIRECTION ( 'NONE',  ( 0.000000000000000000, 0.000000000000000000, 1.000000000000000000 ) ) ;
#39665 = CARTESIAN_POINT ( 'NONE',  ( 804.6798772138708955, -15.72551174932958951, -334.6312213355107019 ) ) ;
#39666 = CARTESIAN_POINT ( 'NONE',  ( 799.9636004259356241, -166.9181544815165523, 311.2241431872006956 ) ) ;
#39667 = EDGE_CURVE ( 'NONE', #36800, #3123, #1961, .T. ) ;
#39668 = CARTESIAN_POINT ( 'NONE',  ( 748.3538107759620743, -88.71468719896009247, -355.8262568251490165 ) ) ;
#39669 = CARTESIAN_POINT ( 'NONE',  ( 748.9653473494363425, -122.6346026584201354, 356.9462024416521331 ) ) ;
#39670 = CARTESIAN_POINT ( 'NONE',  ( 745.0891759886404770, -388.2709662947829656, -342.4968714119734159 ) ) ;
#39671 = CARTESIAN_POINT ( 'NONE',  ( 506.1531787467675940, 50.81038600091411439, 217.3872392842761769 ) ) ;
#39672 = LINE ( 'NONE', #25091, #26426 ) ;
#39673 = EDGE_CURVE ( 'NONE', #40984, #24071, #40691, .T. ) ;
#39674 = CARTESIAN_POINT ( 'NONE',  ( 757.8323909638827445, -218.6346026584197944, 352.1044303154654358 ) ) ;
#39675 = CARTESIAN_POINT ( 'NONE',  ( 791.0478386215596629, -453.8272453906066630, 306.7653713866226326 ) ) ;
#39676 = CARTESIAN_POINT ( 'NONE',  ( 781.2497674668890113, -420.3510508353225532, -375.3608509340180603 ) ) ;
#39677 = CARTESIAN_POINT ( 'NONE',  ( 771.3260364891663130, 4.354572791210176597, -306.0683387631859773 ) ) ;
#39678 = DIRECTION ( 'NONE',  ( 1.000000000000000000, -0.000000000000000000, -0.000000000000000000 ) ) ;
#39679 = CARTESIAN_POINT ( 'NONE',  ( 813.9316612368132837, -31.44195992623299674, 348.6739635108323228 ) ) ;
#39680 = ORIENTED_EDGE ( 'NONE', *, *, #17880, .F. ) ;
#39681 = CIRCLE ( 'NONE', #23405, 2.749999999999835687 ) ;
#39682 = CARTESIAN_POINT ( 'NONE',  ( 761.2382568024794409, -183.6237781080507148, -356.9571628226838129 ) ) ;
#39683 = CARTESIAN_POINT ( 'NONE',  ( 792.1044303154645831, -12.45278447660232146, 317.8323909638837677 ) ) ;
#39684 = CARTESIAN_POINT ( 'NONE',  ( 803.8556311672234642, -201.6237781080506863, -365.6418435158340117 ) ) ;
#39685 = DIRECTION ( 'NONE',  ( -0.000000000000000000, 1.000000000000000000, -0.000000000000000000 ) ) ;
#39686 = CARTESIAN_POINT ( 'NONE',  ( 778.7502325331095108, -336.3510508353228943, 304.6391490659818828 ) ) ;
#39687 = CARTESIAN_POINT ( 'NONE',  ( 800.2193346964446619, -138.9982390220564241, 355.1360043628816925 ) ) ;
#39688 = ORIENTED_EDGE ( 'NONE', *, *, #41073, .F. ) ;
#39689 = VECTOR ( 'NONE', #44599, 1000.000000000000000 ) ;
#39690 = ADVANCED_FACE ( 'NONE', ( #15323 ), #12736, .F. ) ;
#39691 = CARTESIAN_POINT ( 'NONE',  ( 756.3353852180819104, -149.9073299311473875, -331.1735550268788302 ) ) ;
#39692 = CARTESIAN_POINT ( 'NONE',  ( 774.6858677611749044, -345.7255117493285184, 315.5713283507209894 ) ) ;
#39693 = ADVANCED_FACE ( 'NONE', ( #23357, #43698, #22447, #4682, #29620 ), #8833, .T. ) ;
#39694 = CARTESIAN_POINT ( 'NONE',  ( 749.2812353651451076, -54.45278447660219001, -323.2262854647983090 ) ) ;
#39695 = ORIENTED_EDGE ( 'NONE', *, *, #18766, .T. ) ;
#39696 = CARTESIAN_POINT ( 'NONE',  ( 783.7953271457878373, -440.1908817542430370, -375.1787889125761239 ) ) ;
#39697 = VERTEX_POINT ( 'NONE', #32869 ) ;
#39698 = CARTESIAN_POINT ( 'NONE',  ( 758.4439275373578084, -324.5545181178796952, -353.2243759319684386 ) ) ;
#39700 = CARTESIAN_POINT ( 'NONE',  ( 787.5531968255692163, -357.8272453906068904, 316.1348686366205811 ) ) ;
#39699 = CARTESIAN_POINT ( 'NONE',  ( 802.1676090361156639, -62.63460265842031305, 327.8955696845344505 ) ) ;
#39701 = CARTESIAN_POINT ( 'NONE',  ( 765.0180583372156207, -288.9982390220559978, -360.0135310231089534 ) ) ;
#39703 = CARTESIAN_POINT ( 'NONE',  ( 776.2433038121456548, -276.8965053807776258, 374.8207195650711014 ) ) ;
#39702 = CARTESIAN_POINT ( 'NONE',  ( 787.4397851343537695, -405.7255117493283478, 374.2001403089903988 ) ) ;
#39704 = EDGE_CURVE ( 'NONE', #1373, #28817, #529, .T. ) ;
#39705 = CARTESIAN_POINT ( 'NONE',  ( 802.9823548866075953, -289.0999726633343698, -330.0799878456151077 ) ) ;
#39706 = CARTESIAN_POINT ( 'NONE',  ( 757.8323909638827445, -290.6346026584195101, -352.1044303154654358 ) ) ;
#39707 = DIRECTION ( 'NONE',  ( 0.000000000000000000, -0.6594541114781790059, 0.7517448203044204691 ) ) ;
#39708 = CARTESIAN_POINT ( 'NONE',  ( 774.6312213355099630, -167.3618753856927412, -364.6798772138717482 ) ) ;
#39709 = CARTESIAN_POINT ( 'NONE',  ( -200.7583438952259485, 394.6698570112193920, -274.9999999999999432 ) ) ;
#39710 = EDGE_LOOP ( 'NONE', ( #38266, #12102, #10001, #44092 ) ) ;
#39711 = CARTESIAN_POINT ( 'NONE',  ( 749.2812353651451076, -414.4527844766010389, 323.2262854647983090 ) ) ;
#39713 = LINE ( 'NONE', #29519, #35899 ) ;
#39712 = CARTESIAN_POINT ( 'NONE',  ( 794.9999999999993179, -365.3551492539851893, -18.13243251470705886 ) ) ;
#39714 = CARTESIAN_POINT ( 'NONE',  ( 744.6391490659812007, -86.73633629969862113, -338.7502325331110455 ) ) ;
#39715 = CARTESIAN_POINT ( 'NONE',  ( -265.7583438952258916, 430.0000000000002842, -320.0000000000000000 ) ) ;
#39716 = LINE ( 'NONE', #15876, #38555 ) ;
#39717 = CARTESIAN_POINT ( 'NONE',  ( 787.5531968255692163, -285.8272453906071178, 316.1348686366205811 ) ) ;
#39718 = CARTESIAN_POINT ( 'NONE',  ( 792.1044303154645831, -156.4527844766018916, 317.8323909638837677 ) ) ;
#39719 = ORIENTED_EDGE ( 'NONE', *, *, #20624, .T. ) ;
#39720 = CARTESIAN_POINT ( 'NONE',  ( 754.9967657858570647, -97.54369356751114140, -365.0032342141425943 ) ) ;
#39721 = CARTESIAN_POINT ( 'NONE',  ( 769.1273215169530886, -310.7146871989593251, 317.4527132478988847 ) ) ;
#39722 = CIRCLE ( 'NONE', #44125, 10.00000000000000888 ) ;
#39723 = DIRECTION ( 'NONE',  ( 0.000000000000000000, 0.000000000000000000, 1.000000000000000000 ) ) ;
#39724 = CARTESIAN_POINT ( 'NONE',  ( 750.9282345327678740, -40.91815448151695023, 319.8311093483690115 ) ) ;
#39725 = EDGE_CURVE ( 'NONE', #42507, #25509, #29288, .T. ) ;
#39726 = CARTESIAN_POINT ( 'NONE',  ( 814.9108240113580450, -232.2709662947834488, -337.5031285880265273 ) ) ;
#39727 = CARTESIAN_POINT ( 'NONE',  ( 808.0189434323515343, -206.0891481129653471, 319.0252816721025511 ) ) ;
#39728 = CARTESIAN_POINT ( 'NONE',  ( 758.0580252608178853, -126.4527844766019626, 328.0187753319985404 ) ) ;
#39729 = LINE ( 'NONE', #8077, #22519 ) ;
#39730 = CARTESIAN_POINT ( 'NONE',  ( 776.2433038121456548, -300.8965053807775689, -374.8207195650711014 ) ) ;
#39731 = CARTESIAN_POINT ( 'NONE',  ( 805.2837595273609850, -26.73633629969882008, 340.5290396650784714 ) ) ;
#39732 = CARTESIAN_POINT ( 'NONE',  ( 777.4774526936600978, -322.2709662947830225, -304.7301800767027657 ) ) ;
#39733 = DIRECTION ( 'NONE',  ( -4.625929269271485914E-16, 1.000000000000000000, 0.000000000000000000 ) ) ;
#39734 = CARTESIAN_POINT ( 'NONE',  ( 804.9511171171677688, -413.8055962898681059, 335.8780910478229202 ) ) ;
#39735 = ORIENTED_EDGE ( 'NONE', *, *, #10052, .T. ) ;
#39736 = CARTESIAN_POINT ( 'NONE',  ( 797.6776695296629214, -427.5436935675101040, -357.6776695296636603 ) ) ;
#39737 = CARTESIAN_POINT ( 'NONE',  ( 788.7366044899766848, -227.9073299311471033, -316.5762568750059813 ) ) ;
#39738 = CARTESIAN_POINT ( 'NONE',  ( 801.9858362298568863, -99.07832356259642381, -312.7379699480935642 ) ) ;
#39739 = DIRECTION ( 'NONE',  ( 0.000000000000000000, -0.6755902076156505842, -0.7372773368101327440 ) ) ;
#39740 = CARTESIAN_POINT ( 'NONE',  ( 747.3154664389472828, -235.9874144716868898, 326.4474001241230781 ) ) ;
#39741 = CARTESIAN_POINT ( 'NONE',  ( 804.9363028652555840, -40.27096629478405987, 338.2165204200192079 ) ) ;
#39742 = EDGE_CURVE ( 'NONE', #13253, #24672, #19671, .T. ) ;
#39743 = VERTEX_POINT ( 'NONE', #12071 ) ;
#39744 = CARTESIAN_POINT ( 'NONE',  ( 805.1016975059191054, -222.8965053807778531, -343.0745993439771837 ) ) ;
#39745 = CARTESIAN_POINT ( 'NONE',  ( 758.0580252608178853, -222.4527844766016642, 328.0187753319985404 ) ) ;
#39746 = ADVANCED_FACE ( 'NONE', ( #40262 ), #32246, .F. ) ;
#39747 = CARTESIAN_POINT ( 'NONE',  ( 783.7566961878529810, -72.89650538077830788, -305.1792804349288417 ) ) ;
#39748 = CARTESIAN_POINT ( 'NONE',  ( 187.1337867209877857, -416.7569064942979935, -212.5753187112033231 ) ) ;
#39749 = ORIENTED_EDGE ( 'NONE', *, *, #36740, .T. ) ;
#39750 = CARTESIAN_POINT ( 'NONE',  ( 795.8262568251477660, -358.3726999360613945, -308.3538107759623585 ) ) ;
#39751 = VECTOR ( 'NONE', #3278, 1000.000000000000000 ) ;
#39752 = ADVANCED_FACE ( 'NONE', ( #5134 ), #44153, .F. ) ;
#39753 = CARTESIAN_POINT ( 'NONE',  ( 796.7737145352015204, -284.6346026584196807, 370.7187646348536987 ) ) ;
#39754 = CARTESIAN_POINT ( 'NONE',  ( 786.2056067578752163, -11.80559628986942577, 374.4686193811670023 ) ) ;
#39755 = PRODUCT_DEFINITION ( 'UNKNOWN', '', #23069, #9939 ) ;
#39756 = CARTESIAN_POINT ( 'NONE',  ( 799.2566176426618085, -168.0090635724256458, -324.0069404352559559 ) ) ;
#39757 = CARTESIAN_POINT ( 'NONE',  ( 758.0580252608178853, -198.4527844766017495, -328.0187753319985404 ) ) ;
#39758 = CARTESIAN_POINT ( 'NONE',  ( 767.8955696845334842, -384.4527844766011526, -362.1676090361161755 ) ) ;
#39759 = ORIENTED_EDGE ( 'NONE', *, *, #13735, .T. ) ;
#39760 = CARTESIAN_POINT ( 'NONE',  ( 799.4546378042377910, 14.92167643740321381, -356.1575198192848006 ) ) ;
#39761 = ORIENTED_EDGE ( 'NONE', *, *, #109, .F. ) ;
#39762 = CARTESIAN_POINT ( 'NONE',  ( 777.5031285880264704, -334.8164208402376403, 374.9108240113588408 ) ) ;
#39763 = LINE ( 'NONE', #7886, #23325 ) ;
#39764 = CARTESIAN_POINT ( 'NONE',  ( 775.9200461376533440, -359.8055962898683333, 315.3028492785443291 ) ) ;
#39765 = DIRECTION ( 'NONE',  ( 0.000000000000000000, 0.000000000000000000, 1.000000000000000000 ) ) ;
#39766 = CARTESIAN_POINT ( 'NONE',  ( 802.9823548866075953, -145.0999726633347677, 330.0799878456151077 ) ) ;
#39767 = CARTESIAN_POINT ( 'NONE',  ( 771.1735550268778070, -57.18005720387489532, 316.3353852180827630 ) ) ;
#39768 = ORIENTED_EDGE ( 'NONE', *, *, #19956, .T. ) ;
#39769 = CARTESIAN_POINT ( 'NONE',  ( 813.5763878283155464, -411.8272453906067199, -351.1614460488615350 ) ) ;
#39770 = CARTESIAN_POINT ( 'NONE',  ( 772.5602148656447525, 14.27448825067031812, -305.7998596910095443 ) ) ;
#39771 = CARTESIAN_POINT ( 'NONE',  ( 745.7194118038753459, -277.6454272087889308, 348.7631598425976449 ) ) ;
#39772 = CARTESIAN_POINT ( 'NONE',  ( 759.2295555964440155, -208.1692326535051905, 353.9708237608231229 ) ) ;
#39773 = CARTESIAN_POINT ( 'NONE',  ( 803.4237431249931660, -375.1800572038739574, -331.2633955100225194 ) ) ;
#39774 = DIRECTION ( 'NONE',  ( 0.000000000000000000, 0.000000000000000000, -1.000000000000000000 ) ) ;
#39775 = CARTESIAN_POINT ( 'NONE',  ( 804.4286716492782716, 6.638124614306706306, 345.3141322388244703 ) ) ;
#39776 = DIRECTION ( 'NONE',  ( 0.000000000000000000, 0.000000000000000000, 1.000000000000000000 ) ) ;
#39777 = CARTESIAN_POINT ( 'NONE',  ( 776.9254006560222479, -260.1908817542435486, -314.8983024940802125 ) ) ;
#39778 = CARTESIAN_POINT ( 'NONE',  ( 801.1904061080336987, -44.08914811296584446, 368.3070685750235498 ) ) ;
#39779 = CARTESIAN_POINT ( 'NONE',  ( 814.9108240113580450, -112.2709662947838325, 337.5031285880265273 ) ) ;
#39780 = DIRECTION ( 'NONE',  ( 0.000000000000000000, -0.6438296778008192334, 0.7651688349527138167 ) ) ;
#39781 = CIRCLE ( 'NONE', #5068, 4.999999999999984901 ) ;
#39782 = CARTESIAN_POINT ( 'NONE',  ( 814.2805881961230625, -385.6454272087888171, 331.2368401574024119 ) ) ;
#39783 = CARTESIAN_POINT ( 'NONE',  ( 914.9999999999992042, 46.15097736693707020, -350.0000000000000000 ) ) ;
#39784 = CARTESIAN_POINT ( 'NONE',  ( 772.5602148656447525, -369.7255117493284615, 305.7998596910095443 ) ) ;
#39785 = CARTESIAN_POINT ( 'NONE',  ( 794.9819416627830151, -300.9982390220559409, -319.9864689768909898 ) ) ;
#39786 = FACE_OUTER_BOUND ( 'NONE', #28015, .T. ) ;
#39787 = CARTESIAN_POINT ( 'NONE',  ( 804.6798772138708955, -423.7255117493281205, 334.6312213355107019 ) ) ;
#39788 = CARTESIAN_POINT ( 'NONE',  ( 779.4763451958990572, -200.7363362996982801, 365.0264073115438919 ) ) ;
#39789 = CARTESIAN_POINT ( 'NONE',  ( 809.0717654672305343, -52.91815448151692891, -360.1688906516309885 ) ) ;
#39790 = CARTESIAN_POINT ( 'NONE',  ( 805.0264073115434940, -126.3510508353236048, -339.4763451958999099 ) ) ;
#39791 = CARTESIAN_POINT ( 'NONE',  ( 803.8556311672234642, -105.6237781080509421, 365.6418435158340117 ) ) ;
#39792 = CARTESIAN_POINT ( 'NONE',  ( 767.8955696845334842, -432.4527844766009252, 362.1676090361161755 ) ) ;
#39793 = CARTESIAN_POINT ( 'NONE',  ( 764.3348316497523456, -166.7146871989598367, 308.6759233522265617 ) ) ;
#39794 = CARTESIAN_POINT ( 'NONE',  ( 788.8264449731200330, -45.18005720387493085, -363.6646147819171233 ) ) ;
#39795 = CARTESIAN_POINT ( 'NONE',  ( 804.9511171171677688, -125.8055962898690581, -335.8780910478229202 ) ) ;
#39796 = CARTESIAN_POINT ( 'NONE',  ( 805.1927285166397041, -112.8164208402383508, -341.8018195045277707 ) ) ;
#39797 = CARTESIAN_POINT ( 'NONE',  ( 796.7845633553578182, -417.6237781080499190, -358.5707757039688204 ) ) ;
#39799 = CARTESIAN_POINT ( 'NONE',  ( 792.1044303154646968, -252.4527844766015789, 317.8323909638837677 ) ) ;
#39798 = CARTESIAN_POINT ( 'NONE',  ( 802.1676090361156639, -254.6346026584196238, 327.8955696845344505 ) ) ;
#39800 = CARTESIAN_POINT ( 'NONE',  ( 773.4999999999993179, 26.27639943461401018, 900.0000000000001137 ) ) ;
#39801 = ORIENTED_EDGE ( 'NONE', *, *, #6921, .T. ) ;
#39802 = CARTESIAN_POINT ( 'NONE',  ( 786.6156483768007774, 22.55804007376682918, 315.5913626894246136 ) ) ;
#39803 = ORIENTED_EDGE ( 'NONE', *, *, #8040, .T. ) ;
#39804 = CARTESIAN_POINT ( 'NONE',  ( 745.4481719005789273, -195.7255117493290015, 347.5162901302853697 ) ) ;
#39805 = CARTESIAN_POINT ( 'NONE',  ( 757.0176451133909268, -253.0999726633345119, 349.9200121543848354 ) ) ;
#39806 = CARTESIAN_POINT ( 'NONE',  ( 755.8398074228967971, -379.4419599262318457, 333.4516893846970333 ) ) ;
#39807 = ORIENTED_EDGE ( 'NONE', *, *, #14605, .T. ) ;
#39808 = CARTESIAN_POINT ( 'NONE',  ( 804.6971507214547046, -75.28179084515321051, -344.0799538623459739 ) ) ;
#39809 = CARTESIAN_POINT ( 'NONE',  ( 813.2346286133761168, -221.2601417444142271, 328.9521613784389160 ) ) ;
#39810 = CARTESIAN_POINT ( 'NONE',  ( 803.4237431249931660, -279.1800572038741848, -331.2633955100225194 ) ) ;
#39811 = EDGE_LOOP ( 'NONE', ( #45468, #25108, #18603, #7005 ) ) ;
#39812 = CIRCLE ( 'NONE', #44936, 2.749999999999835687 ) ;
#39813 = CARTESIAN_POINT ( 'NONE',  ( 791.9812246680005501, -404.6346026584193396, -361.9419747391813189 ) ) ;
#39814 = CARTESIAN_POINT ( 'NONE',  ( 800.0135310231082713, -62.08914811296580183, -325.0180583372163028 ) ) ;
#39815 = CARTESIAN_POINT ( 'NONE',  ( 796.7845633553578182, -249.6237781080505158, 358.5707757039688204 ) ) ;
#39816 = CARTESIAN_POINT ( 'NONE',  ( 779.9999999999992042, -452.9681489794448339, -339.9999999999999432 ) ) ;
#39817 = FACE_OUTER_BOUND ( 'NONE', #44679, .T. ) ;
#39818 = CARTESIAN_POINT ( 'NONE',  ( 799.9636004259356241, -22.91815448151701062, -311.2241431872006956 ) ) ;
#39819 = FACE_OUTER_BOUND ( 'NONE', #9867, .T. ) ;
#39820 = VERTEX_POINT ( 'NONE', #1653 ) ;
#39821 = CARTESIAN_POINT ( 'NONE',  ( 811.3240766477731540, -316.3726999360615082, -355.6651683502462902 ) ) ;
#39822 = CARTESIAN_POINT ( 'NONE',  ( 745.5313806188320314, -159.2817908451529547, 333.7943932421247268 ) ) ;
#39824 = CARTESIAN_POINT ( 'NONE',  ( 757.8323909638827445, -242.6346026584197659, -352.1044303154654358 ) ) ;
#39823 = CARTESIAN_POINT ( 'NONE',  ( 914.9999999999992042, -431.4567479753239354, 350.0000000000000000 ) ) ;
#39825 =( BOUNDED_CURVE ( )  B_SPLINE_CURVE ( 3, ( #35729, #8033, #32731, #7567 ),
 .UNSPECIFIED., .F., .T. ) 
 B_SPLINE_CURVE_WITH_KNOTS ( ( 4, 4 ),
 ( 1.570796326794896558, 3.141592653589793116 ),
 .UNSPECIFIED. ) 
 CURVE ( )  GEOMETRIC_REPRESENTATION_ITEM ( )  RATIONAL_B_SPLINE_CURVE ( ( 1.000000000000000000, 0.8047378541243649375, 0.8047378541243649375, 1.000000000000000000 ) ) 
 REPRESENTATION_ITEM ( '' )  );
#39826 = DIRECTION ( 'NONE',  ( 0.000000000000000000, -1.000000000000000000, 0.000000000000000000 ) ) ;
#39827 = CARTESIAN_POINT ( 'NONE',  ( 754.7162404726377645, -134.7363362996984790, -339.4709603349214717 ) ) ;
#39828 = CARTESIAN_POINT ( 'NONE',  ( 744.7301800767019131, -28.81642084023863148, 337.4774526936615757 ) ) ;
#39829 = CARTESIAN_POINT ( 'NONE',  ( 701.1634899080286232, 259.9999999999999432, -208.0249999999989825 ) ) ;
#39830 = CARTESIAN_POINT ( 'NONE',  ( 778.7502325331095108, -24.35105083532392811, -304.6391490659818828 ) ) ;
#39831 = CARTESIAN_POINT ( 'NONE',  ( 812.7932403749906598, -351.1800572038740142, -327.7687537140311633 ) ) ;
#39832 = DIRECTION ( 'NONE',  ( 0.000000000000000000, 0.000000000000000000, 1.000000000000000000 ) ) ;
#39833 = CARTESIAN_POINT ( 'NONE',  ( 803.6646147819161570, 6.092670068852159559, 348.8264449731210561 ) ) ;
#39834 = CARTESIAN_POINT ( 'NONE',  ( 813.5763878283155464, -267.8272453906071746, 351.1614460488615350 ) ) ;
#39835 = SHAPE_REPRESENTATION ( 'MAS-320', ( #2446, #15708, #35614, #4665, #41529, #18686, #245, #17965, #20873, #3913, #37834, #26044, #16460 ), #14266 ) ;
#39836 = CARTESIAN_POINT ( 'NONE',  ( 798.0661480581538854, -242.5328690171414507, -309.5768839229118043 ) ) ;
#39837 = CARTESIAN_POINT ( 'NONE',  ( 763.2262854647970016, -272.6346026584196807, 309.2812353651462445 ) ) ;
#39838 = CARTESIAN_POINT ( 'NONE',  ( 805.0032342141412300, 10.45630643248850866, -314.9967657858571783 ) ) ;
#39839 = LINE ( 'NONE', #18803, #37238 ) ;
#39840 = ORIENTED_EDGE ( 'NONE', *, *, #3597, .T. ) ;
#39841 = CARTESIAN_POINT ( 'NONE',  ( 785.3687786644884454, -323.3618753856923149, 315.3201227861279676 ) ) ;
#39842 = CARTESIAN_POINT ( 'NONE',  ( 796.1575198192839480, -78.00906357242591582, 359.4546378042384163 ) ) ;
#39843 = CARTESIAN_POINT ( 'NONE',  ( 805.0264073115434940, -30.35105083532391390, -339.4763451958999099 ) ) ;
#39844 = DIRECTION ( 'NONE',  ( -0.000000000000000000, -0.000000000000000000, 1.000000000000000000 ) ) ;
#39845 = CYLINDRICAL_SURFACE ( 'NONE', #20292, 7.999999999999896083 ) ;
#39847 = CARTESIAN_POINT ( 'NONE',  ( 802.1676090361156639, -350.6346026584192828, 327.8955696845344505 ) ) ;
#39846 = CARTESIAN_POINT ( 'NONE',  ( 794.1144889064781864, -154.1692326535053894, 360.9840315886528401 ) ) ;
#39848 = EDGE_LOOP ( 'NONE', ( #13531, #25457, #13130, #19269 ) ) ;
#39849 = CARTESIAN_POINT ( 'NONE',  ( 787.6308680596127942, -299.2601417444139997, -364.1105419155492768 ) ) ;
#39850 = CARTESIAN_POINT ( 'NONE',  ( 778.1981804954714335, -154.2709662947836478, 314.8072714833589885 ) ) ;
#39851 = EDGE_CURVE ( 'NONE', #41554, #10806, #267, .T. ) ;
#39852 = CARTESIAN_POINT ( 'NONE',  ( 813.9316612368132837, -319.4419599262320730, -348.6739635108323228 ) ) ;
#39853 = CARTESIAN_POINT ( 'NONE',  ( 791.7608162188021197, 205.0000000000000568, -339.9999999999999432 ) ) ;
#39854 = CARTESIAN_POINT ( 'NONE',  ( 755.2512626584698410, 16.45630643248849267, 315.2512626584710915 ) ) ;
#39855 = ORIENTED_EDGE ( 'NONE', *, *, #25795, .T. ) ;
#39856 = CARTESIAN_POINT ( 'NONE',  ( 755.0636971347428243, -340.2709662947831362, 341.7834795799807353 ) ) ;
#39857 = CARTESIAN_POINT ( 'NONE',  ( 763.2154366446407039, -69.62377810805107003, -321.4292242960311228 ) ) ;
#39858 = ORIENTED_EDGE ( 'NONE', *, *, #2061, .F. ) ;
#39859 = CARTESIAN_POINT ( 'NONE',  ( 803.6646147819161570, -449.9073299311463643, 348.8264449731210561 ) ) ;
#39860 = CARTESIAN_POINT ( 'NONE',  ( 751.6929314249748586, -198.9982390220562252, -318.8095938919659034 ) ) ;
#39861 = ORIENTED_EDGE ( 'NONE', *, *, #31530, .F. ) ;
#39862 = CARTESIAN_POINT ( 'NONE',  ( 778.1981804954715471, -130.2709662947837614, -314.8072714833591021 ) ) ;
#39863 = VERTEX_POINT ( 'NONE', #12519 ) ;
#39864 = CARTESIAN_POINT ( 'NONE',  ( 798.5707757039680246, -413.4636090269704027, -356.7845633553585003 ) ) ;
#39865 = CARTESIAN_POINT ( 'NONE',  ( 757.8323909638827445, -2.634602658420536869, 352.1044303154654358 ) ) ;
#39866 = CARTESIAN_POINT ( 'NONE',  ( 777.4774526936600978, -226.2709662947834204, 304.7301800767027657 ) ) ;
#39867 = CARTESIAN_POINT ( 'NONE',  ( 779.4709603349208464, -168.3510508353234911, 314.7162404726379918 ) ) ;
#39869 = CARTESIAN_POINT ( 'NONE',  ( 879.9999999999992042, 239.9999999999998863, -244.9999999999999716 ) ) ;
#39868 = PLANE ( 'NONE',  #13723 ) ;
#39870 = ORIENTED_EDGE ( 'NONE', *, *, #39951, .T. ) ;
#39871 = CARTESIAN_POINT ( 'NONE',  ( 758.4439275373578084, -396.5545181178794678, -353.2243759319684386 ) ) ;
#39872 = DIRECTION ( 'NONE',  ( 0.000000000000000000, 0.000000000000000000, 1.000000000000000000 ) ) ;
#39873 = CARTESIAN_POINT ( 'NONE',  ( 791.0478386215596629, -189.8272453906073736, -306.7653713866226326 ) ) ;
#39874 = CARTESIAN_POINT ( 'NONE',  ( 802.2119215644370342, -54.00906357242601530, 367.5423716828165084 ) ) ;
#39876 = DIRECTION ( 'NONE',  ( 0.000000000000000000, 0.000000000000000000, -1.000000000000000000 ) ) ;
#39875 = CARTESIAN_POINT ( 'NONE',  ( 181.1634899080285948, 240.0000000000000284, -202.7499999999952536 ) ) ;
#39877 = CARTESIAN_POINT ( 'NONE',  ( 755.0488828828309806, -329.8055962898683902, -344.1219089521771934 ) ) ;
#39878 = DIRECTION ( 'NONE',  ( 1.000000000000000000, 0.000000000000000000, 0.000000000000000000 ) ) ;
#39879 = CARTESIAN_POINT ( 'NONE',  ( 788.6739635108323228, -199.6454272087891582, -373.9316612368139090 ) ) ;
#39880 = FACE_OUTER_BOUND ( 'NONE', #44620, .T. ) ;
#39881 = PLANE ( 'NONE',  #10526 ) ;
#39882 = CARTESIAN_POINT ( 'NONE',  ( 802.9823548866075953, -385.0999726633340856, 330.0799878456151077 ) ) ;
#39883 = CARTESIAN_POINT ( 'NONE',  ( 808.0189434323515343, -254.0891481129652334, -319.0252816721025511 ) ) ;
#39884 = PLANE ( 'NONE',  #40107 ) ;
#39885 = CARTESIAN_POINT ( 'NONE',  ( 797.6776695296629214, -19.54369356751139364, -357.6776695296636603 ) ) ;
#39886 = CARTESIAN_POINT ( 'NONE',  ( 771.3260364891663130, -187.6454272087892434, 306.0683387631859773 ) ) ;
#39887 = CARTESIAN_POINT ( 'NONE',  ( 747.3154664389472828, -139.9874144716872024, -326.4474001241230781 ) ) ;
#39888 = CARTESIAN_POINT ( 'NONE',  ( 814.5518280994195948, -135.7255117493291152, 332.4837098697145734 ) ) ;
#39889 = CARTESIAN_POINT ( 'NONE',  ( 812.7932403749906598, -375.1800572038739574, -327.7687537140311633 ) ) ;
#39890 = CARTESIAN_POINT ( 'NONE',  ( 911.9999999999993179, 219.9999999999998863, -350.0000000000000000 ) ) ;
#39891 = DIRECTION ( 'NONE',  ( 1.000000000000000000, 4.625929269271485914E-16, 0.000000000000000000 ) ) ;
#39892 = CARTESIAN_POINT ( 'NONE',  ( 803.6646147819161570, -233.9073299311470180, 348.8264449731210561 ) ) ;
#39893 = CARTESIAN_POINT ( 'NONE',  ( 755.5913626894240451, -13.64542720878976390, 346.6156483768012890 ) ) ;
#39894 = CARTESIAN_POINT ( 'NONE',  ( 761.9338519418445230, -422.5328690171408539, -370.4231160770881957 ) ) ;
#39895 = CARTESIAN_POINT ( 'NONE',  ( 755.8990559732751535, -11.46360902697159290, -365.9055244015606831 ) ) ;
#39896 = FACE_OUTER_BOUND ( 'NONE', #10630, .T. ) ;
#39897 = CARTESIAN_POINT ( 'NONE',  ( 766.5853460496234675, -37.98741447168752927, 372.3518521366060554 ) ) ;
#39898 = ORIENTED_EDGE ( 'NONE', *, *, #17738, .T. ) ;
#39899 = CARTESIAN_POINT ( 'NONE',  ( 755.0636971347428243, -268.2709662947833067, 341.7834795799807353 ) ) ;
#39900 = EDGE_CURVE ( 'NONE', #44015, #16954, #37459, .T. ) ;
#39901 = EDGE_CURVE ( 'NONE', #43290, #42109, #5820, .T. ) ;
#39902 = CARTESIAN_POINT ( 'NONE',  ( 776.9566956441375396, -204.8965053807779100, -364.8461984189686405 ) ) ;
#39903 = CARTESIAN_POINT ( 'NONE',  ( 771.1735550268778070, -33.18005720387498769, 316.3353852180827630 ) ) ;
#39904 = CARTESIAN_POINT ( 'NONE',  ( 788.7631598425961101, -241.4419599262322720, -305.7194118038759143 ) ) ;
#39905 = CARTESIAN_POINT ( 'NONE',  ( 795.6651683502461765, -346.7146871989592682, 371.3240766477733814 ) ) ;
#39906 = CARTESIAN_POINT ( 'NONE',  ( 774.6858677611749044, -81.72551174932937101, -315.5713283507209894 ) ) ;
#39907 = ORIENTED_EDGE ( 'NONE', *, *, #14562, .F. ) ;
#39908 = CARTESIAN_POINT ( 'NONE',  ( 803.4237431249931660, -135.1800572038746679, -331.2633955100225194 ) ) ;
#39909 = CARTESIAN_POINT ( 'NONE',  ( 801.9419747391806368, -354.4527844766012095, 351.9812246680014027 ) ) ;
#39910 = CARTESIAN_POINT ( 'NONE',  ( 808.3070685750230950, -90.99823902205663728, -361.1904061080339261 ) ) ;
#39911 = ORIENTED_EDGE ( 'NONE', *, *, #13176, .T. ) ;
#39912 = CARTESIAN_POINT ( 'NONE',  ( 769.9779781133707957, 4.900027336664720679, -316.7813123517150871 ) ) ;
#39913 = ORIENTED_EDGE ( 'NONE', *, *, #43236, .F. ) ;
#39914 = CARTESIAN_POINT ( 'NONE',  ( 800.9840315886518738, -316.9181544815160692, -354.1144889064786412 ) ) ;
#39916 = CARTESIAN_POINT ( 'NONE',  ( 801.5560724626406000, -384.5545181178795247, 326.7756240680316182 ) ) ;
#39915 = CARTESIAN_POINT ( 'NONE',  ( 759.9864689768902508, -74.08914811296577341, 354.9819416627836404 ) ) ;
#39917 = CARTESIAN_POINT ( 'NONE',  ( 756.5762568750052424, -291.1800572038741848, -348.7366044899774238 ) ) ;
#39919 = CARTESIAN_POINT ( 'NONE',  ( 754.0944755984390895, -327.6237781080502600, 364.1009440267246760 ) ) ;
#39918 = CARTESIAN_POINT ( 'NONE',  ( 748.9653473494365699, -410.6346026584191691, 356.9462024416520762 ) ) ;
#39920 = CARTESIAN_POINT ( 'NONE',  ( 779.4763451958990572, -296.7363362996979390, -365.0264073115438919 ) ) ;
#39921 = CARTESIAN_POINT ( 'NONE',  ( 771.1735550268778070, -297.1800572038740711, -316.3353852180827630 ) ) ;
#39922 = FACE_BOUND ( 'NONE', #3447, .T. ) ;
#39923 = CARTESIAN_POINT ( 'NONE',  ( 785.3141322388236176, -165.7255117493291152, -364.4286716492789537 ) ) ;
#39924 = LINE ( 'NONE', #8057, #43918 ) ;
#39925 = CARTESIAN_POINT ( 'NONE',  ( 787.4397851343537695, -429.7255117493282910, 374.2001403089903988 ) ) ;
#39927 = CYLINDRICAL_SURFACE ( 'NONE', #15274, 20.00000000000001776 ) ;
#39926 = LINE ( 'NONE', #29305, #10094 ) ;
#39928 = CARTESIAN_POINT ( 'NONE',  ( 811.3240766477731540, -100.3726999360622187, -355.6651683502462902 ) ) ;
#39929 = DIRECTION ( 'NONE',  ( 0.000000000000000000, -0.000000000000000000, 1.000000000000000000 ) ) ;
#39930 = DIRECTION ( 'NONE',  ( -0.000000000000000000, 1.000000000000000000, -0.000000000000000000 ) ) ;
#39931 = CARTESIAN_POINT ( 'NONE',  ( 766.0291762391763086, -298.9181544815161828, 360.7704444035551319 ) ) ;
#39932 = CARTESIAN_POINT ( 'NONE',  ( 755.0636971347428243, -148.2709662947837330, 341.7834795799807353 ) ) ;
#39933 = EDGE_LOOP ( 'NONE', ( #20582, #14162, #40105, #37738 ) ) ;
#39934 = CARTESIAN_POINT ( 'NONE',  ( 749.2812353651451076, -126.4527844766019626, -323.2262854647983090 ) ) ;
#39935 = CARTESIAN_POINT ( 'NONE',  ( 769.1273215169530886, -334.7146871989593251, 317.4527132478988847 ) ) ;
#39936 = CARTESIAN_POINT ( 'NONE',  ( 799.9999999999993179, -462.9681489794448339, 309.9999999999998863 ) ) ;
#39937 = CARTESIAN_POINT ( 'NONE',  ( 780.5290396650775619, -420.3510508353225532, -365.2837595273619513 ) ) ;
#39938 = EDGE_CURVE ( 'NONE', #12019, #13947, #35170, .T. ) ;
#39939 = CARTESIAN_POINT ( 'NONE',  ( 745.1792804349281596, -62.19088175424416676, 343.7566961878542884 ) ) ;
#39940 = CARTESIAN_POINT ( 'NONE',  ( 745.7998596910086917, -269.3618753856924286, -332.5602148656461168 ) ) ;
#39941 = EDGE_CURVE ( 'NONE', #37112, #12764, #30761, .T. ) ;
#39942 = CARTESIAN_POINT ( 'NONE',  ( 815.2698199232961542, -208.8164208402380666, 342.5225473063383106 ) ) ;
#39943 = CARTESIAN_POINT ( 'NONE',  ( 755.5713283507202505, -101.3618753856929544, 334.6858677611754729 ) ) ;
#39944 = CARTESIAN_POINT ( 'NONE',  ( 803.8556311672234642, -297.6237781080502600, -365.6418435158340117 ) ) ;
#39945 = CARTESIAN_POINT ( 'NONE',  ( 755.5913626894240451, -13.64542720878976390, 346.6156483768012890 ) ) ;
#39946 = CARTESIAN_POINT ( 'NONE',  ( 814.5518280994195948, -351.7255117493284047, -332.4837098697145734 ) ) ;
#39947 = CARTESIAN_POINT ( 'NONE',  ( -728.8365100919714905, 260.0000000000001705, -199.9999999999890861 ) ) ;
#39948 = CARTESIAN_POINT ( 'NONE',  ( 775.9200461376533440, -383.8055962898682765, 315.3028492785443291 ) ) ;
#39949 = VERTEX_POINT ( 'NONE', #2811 ) ;
#39950 = CARTESIAN_POINT ( 'NONE',  ( 759.9864689768902508, -410.0891481129647218, -354.9819416627836404 ) ) ;
#39951 = EDGE_CURVE ( 'NONE', #17108, #22668, #44853, .T. ) ;
#39952 = CARTESIAN_POINT ( 'NONE',  ( 756.5762568750052424, -219.1800572038744122, -348.7366044899774238 ) ) ;
#39953 = CARTESIAN_POINT ( 'NONE',  ( 798.0661480581538854, -122.5328690171417918, -309.5768839229118043 ) ) ;
#39954 = DIRECTION ( 'NONE',  ( 0.000000000000000000, 0.000000000000000000, 1.000000000000000000 ) ) ;
#39955 = CARTESIAN_POINT ( 'NONE',  ( 778.7502325331095108, -240.3510508353232069, 304.6391490659818828 ) ) ;
#39956 = CARTESIAN_POINT ( 'NONE',  ( 805.1927285166399315, -64.81642084023852135, 341.8018195045277707 ) ) ;
#39957 = CARTESIAN_POINT ( 'NONE',  ( 759.9864689768902508, -242.0891481129652618, 354.9819416627836404 ) ) ;
#39958 = CARTESIAN_POINT ( 'NONE',  ( 808.7758568127978833, -52.16923265350567362, -320.0363995740631822 ) ) ;
#39959 = CARTESIAN_POINT ( 'NONE',  ( 775.4999999999993179, -513.1383975375929367, -369.9999999999999432 ) ) ;
#39960 = EDGE_CURVE ( 'NONE', #18073, #21723, #27505, .T. ) ;
#39961 = EDGE_LOOP ( 'NONE', ( #31598, #17843, #6268, #13991, #7922, #24958 ) ) ;
#39962 = VERTEX_POINT ( 'NONE', #6264 ) ;
#39963 = CARTESIAN_POINT ( 'NONE',  ( 748.6759233522253680, -328.3726999360615650, -324.3348316497537098 ) ) ;
#39964 = EDGE_CURVE ( 'NONE', #4785, #9965, #10411, .T. ) ;
#39965 = CARTESIAN_POINT ( 'NONE',  ( 804.7487373415286811, -283.5436935675105019, 364.7487373415288516 ) ) ;
#39966 = CARTESIAN_POINT ( 'NONE',  ( 746.7653713866222915, -17.26014174441486659, 351.0478386215610271 ) ) ;
#39967 = CARTESIAN_POINT ( 'NONE',  ( 780.5236548040995785, -188.7363362996983085, -314.9735926884559944 ) ) ;
#39968 = CARTESIAN_POINT ( 'NONE',  ( 762.1405469898971887, -193.5436935675108714, -357.8594530101015607 ) ) ;
#39969 = CARTESIAN_POINT ( 'NONE',  ( 774.6858677611749044, -369.7255117493284615, -315.5713283507209894 ) ) ;
#39970 = EDGE_LOOP ( 'NONE', ( #2814, #24137, #43514, #40967 ) ) ;
#39971 = VERTEX_POINT ( 'NONE', #38150 ) ;
#39972 = CARTESIAN_POINT ( 'NONE',  ( 772.4837098697144029, -311.3618753856922581, 374.5518280994205611 ) ) ;
#39973 = DIRECTION ( 'NONE',  ( 0.000000000000000000, -0.000000000000000000, -1.000000000000000000 ) ) ;
#39974 = LINE ( 'NONE', #11571, #6173 ) ;
#39975 = CARTESIAN_POINT ( 'NONE',  ( 784.1219089521767955, -189.2817908451528979, 315.0488828828318333 ) ) ;
#39976 = CARTESIAN_POINT ( 'NONE',  ( 804.6798772138708955, -39.72551174932951312, 334.6312213355107019 ) ) ;
#39977 = ORIENTED_EDGE ( 'NONE', *, *, #31202, .F. ) ;
#39978 = CARTESIAN_POINT ( 'NONE',  ( 757.7880784355613741, -426.0090635724247932, -312.4576283171834916 ) ) ;
#39979 = EDGE_CURVE ( 'NONE', #36831, #296, #20579, .T. ) ;
#39980 = CARTESIAN_POINT ( 'NONE',  ( 814.5518280994195948, -39.72551174932951312, -332.4837098697145166 ) ) ;
#39981 = CARTESIAN_POINT ( 'NONE',  ( 763.2154366446407039, -213.6237781080506011, 321.4292242960311228 ) ) ;
#39982 = CARTESIAN_POINT ( 'NONE',  ( 788.8264449731200330, -381.1800572038737869, -363.6646147819171233 ) ) ;
#39983 = CARTESIAN_POINT ( 'NONE',  ( 785.3141322388236176, 2.274488250670355871, -364.4286716492789537 ) ) ;
#39984 = ADVANCED_FACE ( 'NONE', ( #30515 ), #12982, .F. ) ;
#39985 = CARTESIAN_POINT ( 'NONE',  ( 815.2698199232961542, -424.8164208402372992, 342.5225473063383106 ) ) ;
#39986 = DIRECTION ( 'NONE',  ( 0.000000000000000000, 0.000000000000000000, 1.000000000000000000 ) ) ;
#39987 = CARTESIAN_POINT ( 'NONE',  ( 796.1575198192839480, -246.0090635724253900, -359.4546378042384163 ) ) ;
#39988 = CARTESIAN_POINT ( 'NONE',  ( 796.9462024416508257, -156.4527844766018916, -308.9653473494370246 ) ) ;
#39989 = ADVANCED_FACE ( 'NONE', ( #24031 ), #34892, .F. ) ;
#39990 = CARTESIAN_POINT ( 'NONE',  ( 812.7932403749906598, -63.18005720387488822, 327.7687537140311633 ) ) ;
#39991 = CARTESIAN_POINT ( 'NONE',  ( 767.6429770376289525, -105.1800572038747248, 306.8695393053162093 ) ) ;
#39992 = CARTESIAN_POINT ( 'NONE',  ( 763.3756531158825283, 16.45630643248848912, -321.2690078247891847 ) ) ;
#39993 = CARTESIAN_POINT ( 'NONE',  ( 750.9282345327678740, -400.9181544815159555, 319.8311093483690115 ) ) ;
#39994 = CARTESIAN_POINT ( 'NONE',  ( 799.9999999999993179, -512.9681489794448908, 329.9999999999999432 ) ) ;
#39995 = CARTESIAN_POINT ( 'NONE',  ( 787.5162901302840055, -371.3618753856919739, 305.4481719005792684 ) ) ;
#39996 = CARTESIAN_POINT ( 'NONE',  ( 781.8018195045266339, -310.2709662947832499, -365.1927285166406705 ) ) ;
#39997 = CARTESIAN_POINT ( 'NONE',  ( 765.8855110935204493, 25.83076734649409545, 319.0159684113471599 ) ) ;
#39998 = AXIS2_PLACEMENT_3D ( 'NONE', #41972, #24168, #17937 ) ;
#39999 = CARTESIAN_POINT ( 'NONE',  ( 810.4231160770870019, -48.55451811788057626, -321.9338519418446936 ) ) ;
#40000 = CARTESIAN_POINT ( 'NONE',  ( 786.6156483768007774, -121.4419599262327267, -315.5913626894246136 ) ) ;
#40001 = CARTESIAN_POINT ( 'NONE',  ( 751.2241431872005251, -136.1692326535053894, 359.9636004259367610 ) ) ;
#40002 = CARTESIAN_POINT ( 'NONE',  ( 754.8072714833583632, -436.8164208402372992, 338.1981804954721156 ) ) ;
#40003 = CARTESIAN_POINT ( 'NONE',  ( 785.3687786644884454, -11.36187538569323863, -315.3201227861279676 ) ) ;
#40004 = CARTESIAN_POINT ( 'NONE',  ( 798.7617431975189675, -123.6237781080508569, -323.0428371773161871 ) ) ;
#40005 = CARTESIAN_POINT ( 'NONE',  ( 781.8018195045266339, -142.2709662947837330, -365.1927285166406705 ) ) ;
#40006 = CARTESIAN_POINT ( 'NONE',  ( 793.4146539503750546, 22.01258552831228599, -307.6481478633938877 ) ) ;
#40008 = CARTESIAN_POINT ( 'NONE',  ( 795.1360043628808398, -260.0891481129650629, 360.2193346964456282 ) ) ;
#40007 = CARTESIAN_POINT ( 'NONE',  ( 757.8323909638827445, -266.6346026584197375, 352.1044303154654358 ) ) ;
#40009 = CARTESIAN_POINT ( 'NONE',  ( -26.63011601220122060, -512.9681489794448908, -350.0000000000000000 ) ) ;
#40010 = VERTEX_POINT ( 'NONE', #6032 ) ;
#40011 = CARTESIAN_POINT ( 'NONE',  ( 758.6633372737375112, 3.467130982857797417, 326.9102291470432533 ) ) ;
#40012 = VERTEX_POINT ( 'NONE', #34675 ) ;
#40013 = CARTESIAN_POINT ( 'NONE',  ( 812.7932403749906598, -183.1800572038744974, 327.7687537140311633 ) ) ;
#40014 = CARTESIAN_POINT ( 'NONE',  ( 755.3028492785439312, -279.2817908451526137, 335.9200461376539693 ) ) ;
#40015 = CARTESIAN_POINT ( 'NONE',  ( 805.0264073115434940, -414.3510508353227237, 339.4763451958999099 ) ) ;
#40016 = EDGE_LOOP ( 'NONE', ( #31983, #40574, #27598, #38093 ) ) ;
#40017 = CARTESIAN_POINT ( 'NONE',  ( 755.8894580844503253, -87.82724539060770041, -332.3691319403863531 ) ) ;
#40018 = VECTOR ( 'NONE', #9855, 1000.000000000000000 ) ;
#40019 = CARTESIAN_POINT ( 'NONE',  ( 771.2368401574024119, -205.4419599262324425, 374.2805881961240857 ) ) ;
#40020 = CARTESIAN_POINT ( 'NONE',  ( 804.6798772138710092, -279.7255117493288026, -334.6312213355106451 ) ) ;
#40021 = ORIENTED_EDGE ( 'NONE', *, *, #8949, .F. ) ;
#40022 = CARTESIAN_POINT ( 'NONE',  ( 800.2193346964447755, -378.9982390220555999, -355.1360043628815788 ) ) ;
#40023 = CARTESIAN_POINT ( 'NONE',  ( 757.8323909638827445, -50.63460265842036989, -352.1044303154654358 ) ) ;
#40024 = CARTESIAN_POINT ( 'NONE',  ( 804.1601925771018387, -271.4419599262321867, 346.5483106153029098 ) ) ;
#40025 = DIRECTION ( 'NONE',  ( 4.625929269271485914E-16, -1.000000000000000000, 0.000000000000000000 ) ) ;
#40026 = CARTESIAN_POINT ( 'NONE',  ( -879.9999999999992042, 430.0000000000002842, -244.9999999999999716 ) ) ;
#40027 = CARTESIAN_POINT ( 'NONE',  ( 757.7880784355613741, -18.00906357242611477, -312.4576283171834916 ) ) ;
#40028 = LINE ( 'NONE', #18342, #34983 ) ;
#40029 = VERTEX_POINT ( 'NONE', #37911 ) ;
#40030 = CARTESIAN_POINT ( 'NONE',  ( 768.9521613784389729, -321.8272453906070609, -373.2346286133773106 ) ) ;
#40031 = CARTESIAN_POINT ( 'NONE',  ( 760.0363995740630116, -178.9181544815165239, 368.7758568127991907 ) ) ;
#40033 = CARTESIAN_POINT ( 'NONE',  ( 785.3141322388236176, -309.7255117493287457, -364.4286716492789537 ) ) ;
#40032 = DIRECTION ( 'NONE',  ( 1.000000000000000000, 0.000000000000000000, -0.000000000000000000 ) ) ;
#40034 = CARTESIAN_POINT ( 'NONE',  ( 769.9779781133707957, -139.0999726633348530, -316.7813123517150871 ) ) ;
#40035 = CARTESIAN_POINT ( 'NONE',  ( 808.0189434323515343, -14.08914811296595460, 319.0252816721025511 ) ) ;
#40036 = PLANE ( 'NONE',  #6236 ) ;
#40037 = CARTESIAN_POINT ( 'NONE',  ( 808.3070685750232087, -330.9982390220558273, -361.1904061080339829 ) ) ;
#40038 = LINE ( 'NONE', #36117, #29073 ) ;
#40039 = CARTESIAN_POINT ( 'NONE',  ( 771.1735550268778070, -33.18005720387498769, 316.3353852180827630 ) ) ;
#40040 = CARTESIAN_POINT ( 'NONE',  ( 802.2119215644370342, -270.0090635724253048, 367.5423716828165084 ) ) ;
#40041 = CARTESIAN_POINT ( 'NONE',  ( 786.2056067578752163, -251.8055962898686744, -374.4686193811670023 ) ) ;
#40042 = CARTESIAN_POINT ( 'NONE',  ( 814.5518280994195948, -255.7255117493287742, 332.4837098697145734 ) ) ;
#40043 = CARTESIAN_POINT ( 'NONE',  ( 787.4397851343537695, 2.274488250670355871, -374.2001403089903988 ) ) ;
#40044 = CARTESIAN_POINT ( 'NONE',  ( 190.7583438952258916, 294.6698570112193920, -274.9999999999999432 ) ) ;
#40045 = ORIENTED_EDGE ( 'NONE', *, *, #7796, .F. ) ;
#40046 = CARTESIAN_POINT ( 'NONE',  ( 774.6312213355099630, -359.3618753856920875, 364.6798772138717482 ) ) ;
#40047 = CARTESIAN_POINT ( 'NONE',  ( 793.0897708529556667, -78.55451811788046257, 361.3366627262616362 ) ) ;
#40048 = CARTESIAN_POINT ( 'NONE',  ( 756.1348686366196716, -17.26014174441486659, -347.5531968255698416 ) ) ;
#40049 = CARTESIAN_POINT ( 'NONE',  ( 181.1634899080285948, 256.5000000000000000, -197.2499999999955094 ) ) ;
#40050 = LINE ( 'NONE', #19245, #41746 ) ;
#40051 = CARTESIAN_POINT ( 'NONE',  ( 756.3353852180819104, -389.9073299311465348, 331.1735550268788302 ) ) ;
#40052 = VERTEX_POINT ( 'NONE', #41604 ) ;
#40053 = CARTESIAN_POINT ( 'NONE',  ( 805.1016975059191054, -342.8965053807773984, -343.0745993439771837 ) ) ;
#40054 = CARTESIAN_POINT ( 'NONE',  ( 797.6776695296629214, -163.5436935675109567, 357.6776695296636603 ) ) ;
#40055 = CARTESIAN_POINT ( 'NONE',  ( 748.3538107759620743, -328.7146871989592682, -355.8262568251490165 ) ) ;
#40056 = CARTESIAN_POINT ( 'NONE',  ( 919.9999999999993179, 219.9999999999998863, 350.0000000000000000 ) ) ;
#40057 = CARTESIAN_POINT ( 'NONE',  ( 810.7187646348534145, 5.547215523397618142, 356.7737145352016341 ) ) ;
#40058 = ORIENTED_EDGE ( 'NONE', *, *, #37012, .F. ) ;
#40059 = CARTESIAN_POINT ( 'NONE',  ( 792.1044303154645831, -348.4527844766012663, 317.8323909638837677 ) ) ;
#40060 = CARTESIAN_POINT ( 'NONE',  ( 754.9735926884551418, -66.35105083532378956, -340.5236548041000333 ) ) ;
#40061 = VERTEX_POINT ( 'NONE', #3257 ) ;
#40062 = CARTESIAN_POINT ( 'NONE',  ( 755.5713283507202505, -437.3618753856919170, 334.6858677611754729 ) ) ;
#40063 = CARTESIAN_POINT ( 'NONE',  ( 748.9653473494363425, -170.6346026584199649, -356.9462024416521331 ) ) ;
#40064 = ORIENTED_EDGE ( 'NONE', *, *, #30300, .F. ) ;
#40065 = CARTESIAN_POINT ( 'NONE',  ( 781.8018195045267476, -166.2709662947836478, -365.1927285166407273 ) ) ;
#40066 = ORIENTED_EDGE ( 'NONE', *, *, #25832, .T. ) ;
#40067 = CARTESIAN_POINT ( 'NONE',  ( 790.9844846989617508, -430.3726999360611671, -317.2208543904092721 ) ) ;
#40068 = CARTESIAN_POINT ( 'NONE',  ( 804.1105419155481968, -459.8272453906066062, 347.6308680596136469 ) ) ;
#40069 = CARTESIAN_POINT ( 'NONE',  ( 767.6429770376289525, -225.1800572038743269, 306.8695393053162093 ) ) ;
#40070 = CARTESIAN_POINT ( 'NONE',  ( 803.2186876482843445, -151.9874144716871740, 350.0220218866286928 ) ) ;
#40072 = DIRECTION ( 'NONE',  ( 0.000000000000000000, 0.000000000000000000, 1.000000000000000000 ) ) ;
#40071 = DIRECTION ( 'NONE',  ( 0.000000000000000000, -0.3835384033298676054, -0.9235249282889855804 ) ) ;
#40073 = EDGE_LOOP ( 'NONE', ( #4254, #30736, #31968, #31768 ) ) ;
#40074 = CARTESIAN_POINT ( 'NONE',  ( 763.0428371773158460, -419.4636090269702891, -358.7617431975195359 ) ) ;
#40075 = CARTESIAN_POINT ( 'NONE',  ( 767.9999999999992042, 205.0000000000000568, 329.9999999999999432 ) ) ;
#40076 = AXIS2_PLACEMENT_3D ( 'NONE', #33221, #27192, #16576 ) ;
#40077 = CARTESIAN_POINT ( 'NONE',  ( 811.3240766477731540, -196.3726999360619061, -355.6651683502462902 ) ) ;
#40078 = CARTESIAN_POINT ( 'NONE',  ( 757.7880784355613741, -42.00906357242603661, 312.4576283171834916 ) ) ;
#40079 = CARTESIAN_POINT ( 'NONE',  ( 809.0717654672305343, -76.91815448151683654, 360.1688906516309885 ) ) ;
#40081 = LINE ( 'NONE', #14475, #32168 ) ;
#40080 = DIRECTION ( 'NONE',  ( 0.000000000000000000, 0.000000000000000000, -1.000000000000000000 ) ) ;
#40082 = CARTESIAN_POINT ( 'NONE',  ( 803.2186876482843445, -319.9874144716866340, -350.0220218866286928 ) ) ;
#40083 = DIRECTION ( 'NONE',  ( -0.000000000000000000, 1.000000000000000000, -0.000000000000000000 ) ) ;
#40084 = CARTESIAN_POINT ( 'NONE',  ( 764.1737431748507561, -226.3726999360617924, -371.6461892240376415 ) ) ;
#40085 = CARTESIAN_POINT ( 'NONE',  ( -26.63011601220122060, -494.6608068873671300, -357.6536686473015720 ) ) ;
#40086 = CARTESIAN_POINT ( 'NONE',  ( 454.7528517110262101, 199.9999999999999432, 350.0000000000000000 ) ) ;
#40087 = CARTESIAN_POINT ( 'NONE',  ( 773.4516893846965786, -403.6454272087884760, 315.8398074228977066 ) ) ;
#40088 = CARTESIAN_POINT ( 'NONE',  ( 815.2698199232962679, -232.8164208402379529, -342.5225473063383674 ) ) ;
#40089 = CARTESIAN_POINT ( 'NONE',  ( -26.63011601220122060, -496.5085659523897448, -356.8883017825714319 ) ) ;
#40090 = CARTESIAN_POINT ( 'NONE',  ( 756.5762568750052424, -3.180057203875080063, -348.7366044899774238 ) ) ;
#40091 = VECTOR ( 'NONE', #17688, 1000.000000000000114 ) ;
#40092 = CARTESIAN_POINT ( 'NONE',  ( 807.2620300519052989, -192.0090635724255606, 318.0141637701419768 ) ) ;
#40093 = CARTESIAN_POINT ( 'NONE',  ( 801.9858362298568863, -123.0783235625963385, -312.7379699480935642 ) ) ;
#40094 = CARTESIAN_POINT ( 'NONE',  ( 804.7487373415286811, -139.5436935675110135, 364.7487373415288516 ) ) ;
#40095 = CARTESIAN_POINT ( 'NONE',  ( 814.9108240113580450, -376.2709662947829656, -337.5031285880265273 ) ) ;
#40096 = DIRECTION ( 'NONE',  ( 0.000000000000000000, 1.000000000000000000, -0.000000000000000000 ) ) ;
#40097 = DIRECTION ( 'NONE',  ( 0.000000000000000000, 0.000000000000000000, -1.000000000000000000 ) ) ;
#40098 = CARTESIAN_POINT ( 'NONE',  ( 800.0135310231082713, -206.0891481129653471, 325.0180583372163028 ) ) ;
#40099 = CARTESIAN_POINT ( 'NONE',  ( 802.9823548866075953, -25.09997266333519050, 330.0799878456151077 ) ) ;
#40100 = CARTESIAN_POINT ( 'NONE',  ( 754.8072714833581358, -388.8164208402374129, -338.1981804954720587 ) ) ;
#40101 = CARTESIAN_POINT ( 'NONE',  ( 811.3240766477731540, -4.372699936062523385, -355.6651683502462902 ) ) ;
#40102 = DIRECTION ( 'NONE',  ( -1.000000000000000000, -0.000000000000000000, -0.000000000000000000 ) ) ;
#40103 = CARTESIAN_POINT ( 'NONE',  ( 776.2433038121456548, -36.89650538077844288, 374.8207195650711014 ) ) ;
#40104 = CARTESIAN_POINT ( 'NONE',  ( 802.1676090361156639, -302.6346026584196238, 327.8955696845344505 ) ) ;
#40105 = ORIENTED_EDGE ( 'NONE', *, *, #28933, .F. ) ;
#40106 = CARTESIAN_POINT ( 'NONE',  ( 783.0433043558608688, -240.8965053807777963, -315.1538015810313027 ) ) ;
#40107 = AXIS2_PLACEMENT_3D ( 'NONE', #3852, #25550, #32012 ) ;
#40108 = CARTESIAN_POINT ( 'NONE',  ( 800.0135310231082713, -38.08914811296587999, 325.0180583372163028 ) ) ;
#40109 = CARTESIAN_POINT ( 'NONE',  ( 746.0683387631852383, -211.4419599262324709, -331.3260364891676204 ) ) ;
#40110 = DIRECTION ( 'NONE',  ( -0.000000000000000000, -0.000000000000000000, 1.000000000000000000 ) ) ;
#40111 = CARTESIAN_POINT ( 'NONE',  ( 771.2368401574024119, -349.4419599262320162, 374.2805881961240857 ) ) ;
#40112 = VECTOR ( 'NONE', #1821, 1000.000000000000114 ) ;
#40113 = ORIENTED_EDGE ( 'NONE', *, *, #41357, .F. ) ;
#40114 = CARTESIAN_POINT ( 'NONE',  ( 744.8212110874229666, -426.8965053807771142, 336.2046728542121627 ) ) ;
#40115 = CARTESIAN_POINT ( 'NONE',  ( 774.6312213355099630, -335.3618753856920307, 364.6798772138717482 ) ) ;
#40116 = CARTESIAN_POINT ( 'NONE',  ( 767.7687537140311633, -71.90732993114760063, -372.7932403749916830 ) ) ;
#40117 = CARTESIAN_POINT ( 'NONE',  ( 759.7806653035535192, -78.99823902205665149, -324.8639956371181370 ) ) ;
#40118 = ORIENTED_EDGE ( 'NONE', *, *, #25210, .T. ) ;
#40119 = CARTESIAN_POINT ( 'NONE',  ( 755.5913626894240451, -13.64542720878976390, -346.6156483768012890 ) ) ;
#40120 = VERTEX_POINT ( 'NONE', #24264 ) ;
#40121 = CARTESIAN_POINT ( 'NONE',  ( 799.2566176426618085, -312.0090635724251911, -324.0069404352559559 ) ) ;
#40122 = ITEM_DEFINED_TRANSFORMATION ( 'NONE', 'NONE', #16460,  #26858 ) ;
#40123 = VECTOR ( 'NONE', #43751, 1000.000000000000000 ) ;
#40125 = CARTESIAN_POINT ( 'NONE',  ( 805.2837595273609850, -362.7363362996977116, 340.5290396650784714 ) ) ;
#40124 = CARTESIAN_POINT ( 'NONE',  ( 774.6858677611749044, -57.72551174932945628, 315.5713283507209894 ) ) ;
#40126 = CARTESIAN_POINT ( 'NONE',  ( 755.5713283507202505, -317.3618753856922581, -334.6858677611754729 ) ) ;
#40129 = CARTESIAN_POINT ( 'NONE',  ( 744.9990715423526808, -330.3510508353229511, 341.2370466360926002 ) ) ;
#40128 = CARTESIAN_POINT ( 'NONE',  ( -786.4999999999993179, -30.07539427629363260, 756.1153575698151599 ) ) ;
#40127 = CARTESIAN_POINT ( 'NONE',  ( 755.2512626584698410, -439.5436935675101040, 315.2512626584710915 ) ) ;
#40130 = CARTESIAN_POINT ( 'NONE',  ( 805.2837595273609850, -338.7363362996978822, -340.5290396650784714 ) ) ;
#40131 = CARTESIAN_POINT ( 'NONE',  ( 778.2165204200184689, -286.8164208402378677, -364.9363028652563230 ) ) ;
#40132 = CARTESIAN_POINT ( 'NONE',  ( 791.7608162188021197, 178.9475563372491251, -320.0000000000000000 ) ) ;
#40133 = CARTESIAN_POINT ( 'NONE',  ( 762.1405469898971887, -145.5436935675109851, -357.8594530101015607 ) ) ;
#40134 = EDGE_CURVE ( 'NONE', #35503, #9202, #13215, .T. ) ;
#40135 = DIRECTION ( 'NONE',  ( 1.000000000000000000, 0.000000000000000000, 0.000000000000000000 ) ) ;
#40136 = CARTESIAN_POINT ( 'NONE',  ( 747.2067596250078623, -411.1800572038738437, 352.2312462859687230 ) ) ;
#40138 = CARTESIAN_POINT ( 'NONE',  ( 959.5497976682736407, 120.6654763175833693, -2132.806278688367456 ) ) ;
#40137 = DIRECTION ( 'NONE',  ( -1.000000000000000000, 0.000000000000000000, 0.000000000000000000 ) ) ;
#40139 = CARTESIAN_POINT ( 'NONE',  ( 771.3260364891663130, -91.64542720878951343, -306.0683387631859773 ) ) ;
#40140 = LINE ( 'NONE', #39715, #38140 ) ;
#40141 = CARTESIAN_POINT ( 'NONE',  ( 799.9999999999993179, 205.0000000000000568, -255.0000000000000000 ) ) ;
#40142 = EDGE_CURVE ( 'NONE', #38597, #24791, #34200, .T. ) ;
#40143 = CARTESIAN_POINT ( 'NONE',  ( 793.9708237608222134, -310.9181544815160123, 319.2295555964448681 ) ) ;
#40144 = CARTESIAN_POINT ( 'NONE',  ( 768.0187753319979720, -176.6346026584199933, 318.0580252608186242 ) ) ;
#40145 = ORIENTED_EDGE ( 'NONE', *, *, #27263, .F. ) ;
#40146 = VECTOR ( 'NONE', #16715, 1000.000000000000000 ) ;
#40147 = CIRCLE ( 'NONE', #9140, 30.00000000000008171 ) ;
#40148 = CARTESIAN_POINT ( 'NONE',  ( 758.8095938919644823, -128.0891481129655745, -311.6929314249762797 ) ) ;
#40149 = CARTESIAN_POINT ( 'NONE',  ( 755.8398074228967971, -331.4419599262320162, 333.4516893846970333 ) ) ;
#40150 = CARTESIAN_POINT ( 'NONE',  ( 811.3240766477731540, -76.37269993606228979, 355.6651683502462902 ) ) ;
#40151 = CARTESIAN_POINT ( 'NONE',  ( 772.4837098697144029, -263.3618753856924855, -374.5518280994205611 ) ) ;
#40152 = CARTESIAN_POINT ( 'NONE',  ( 756.3353852180819104, -101.9073299311474727, 331.1735550268788302 ) ) ;
#40153 = EDGE_LOOP ( 'NONE', ( #37550, #35919, #27784, #38938 ) ) ;
#40154 = CARTESIAN_POINT ( 'NONE',  ( 800.1688906516307043, -346.1692326535047641, -369.0717654672308186 ) ) ;
#40155 = CARTESIAN_POINT ( 'NONE',  ( 751.6929314249748586, -78.99823902205662307, -318.8095938919659034 ) ) ;
#40156 = CIRCLE ( 'NONE', #6948, 30.00000000000008171 ) ;
#40157 = CARTESIAN_POINT ( 'NONE',  ( 773.4516893846965786, -19.64542720878974791, 315.8398074228977066 ) ) ;
#40158 = CARTESIAN_POINT ( 'NONE',  ( 745.4481719005789273, -363.7255117493284047, -347.5162901302853129 ) ) ;
#40159 = DIRECTION ( 'NONE',  ( 0.000000000000000000, 0.000000000000000000, 1.000000000000000000 ) ) ;
#40160 = CARTESIAN_POINT ( 'NONE',  ( 763.2154366446407039, -405.6237781080500326, 321.4292242960311228 ) ) ;
#40161 = VERTEX_POINT ( 'NONE', #13435 ) ;
#40162 = CARTESIAN_POINT ( 'NONE',  ( 773.3843516231979720, -85.44195992623282621, 364.4086373105754433 ) ) ;
#40163 = CARTESIAN_POINT ( 'NONE',  ( 771.2633955100217236, -431.9073299311464211, -363.4237431249939618 ) ) ;
#40164 = AXIS2_PLACEMENT_3D ( 'NONE', #1725, #37304, #36639 ) ;
#40165 = CARTESIAN_POINT ( 'NONE',  ( 778.7502325331095108, -120.3510508353236048, -304.6391490659818828 ) ) ;
#40166 = CARTESIAN_POINT ( 'NONE',  ( -784.4999999999993179, -563.3203001761230553, -342.3463313526983143 ) ) ;
#40167 = CARTESIAN_POINT ( 'NONE',  ( 761.9338519418445230, -254.5328690171413655, 370.4231160770881957 ) ) ;
#40168 = CARTESIAN_POINT ( 'NONE',  ( 803.6646147819162707, -65.90732993114760063, 348.8264449731211130 ) ) ;
#40169 = EDGE_LOOP ( 'NONE', ( #30232, #3261 ) ) ;
#40170 = CARTESIAN_POINT ( 'NONE',  ( 804.1601925771018387, -247.4419599262323004, -346.5483106153029098 ) ) ;
#40171 = CARTESIAN_POINT ( 'NONE',  ( 785.3687786644884454, -251.3618753856923149, 315.3201227861279676 ) ) ;
#40172 = CARTESIAN_POINT ( 'NONE',  ( 777.4774526936600978, 13.72903370521577138, -304.7301800767027657 ) ) ;
#40173 = CARTESIAN_POINT ( 'NONE',  ( 766.5853460496234675, -61.98741447168745822, -372.3518521366060554 ) ) ;
#40174 = CARTESIAN_POINT ( 'NONE',  ( 799.9999999999993179, 205.0000000000000568, -255.0000000000000000 ) ) ;
#40175 = CIRCLE ( 'NONE', #39436, 20.00000000000004619 ) ;
#40176 = ORIENTED_EDGE ( 'NONE', *, *, #27775, .F. ) ;
#40177 = ORIENTED_EDGE ( 'NONE', *, *, #43330, .T. ) ;
#40178 = CARTESIAN_POINT ( 'NONE',  ( 795.8262568251477660, -382.3726999360613945, -308.3538107759623585 ) ) ;
#40179 = CIRCLE ( 'NONE', #20253, 8.000000000000007105 ) ;
#40180 = CARTESIAN_POINT ( 'NONE',  ( 787.5162901302840055, -299.3618753856923149, 305.4481719005793252 ) ) ;
#40181 = EDGE_CURVE ( 'NONE', #22673, #19543, #16676, .T. ) ;
#40182 = CARTESIAN_POINT ( 'NONE',  ( 758.0141637701419768, -39.07832356259662276, 367.2620300519063790 ) ) ;
#40183 = CARTESIAN_POINT ( 'NONE',  ( 772.4468031744293057, -177.8272453906074304, -363.8651313633793620 ) ) ;
#40184 = CARTESIAN_POINT ( 'NONE',  ( 754.8072714833581358, -172.8164208402381234, -338.1981804954720587 ) ) ;
#40185 = CARTESIAN_POINT ( 'NONE',  ( 804.9363028652555840, -400.2709662947828519, -338.2165204200192079 ) ) ;
#40186 = CIRCLE ( 'NONE', #26876, 6.119000000000013095 ) ;
#40187 = ORIENTED_EDGE ( 'NONE', *, *, #31535, .T. ) ;
#40188 = CARTESIAN_POINT ( 'NONE',  ( 768.0187753319979720, -224.6346026584198228, 318.0580252608186242 ) ) ;
#40189 = CARTESIAN_POINT ( 'NONE',  ( 795.1360043628807261, -452.0891481129646650, -360.2193346964456282 ) ) ;
#40190 = EDGE_LOOP ( 'NONE', ( #33580, #6717 ) ) ;
#40191 = CARTESIAN_POINT ( 'NONE',  ( 801.1904061080336987, -332.0891481129649492, 368.3070685750235498 ) ) ;
#40192 = VECTOR ( 'NONE', #19143, 1000.000000000000000 ) ;
#40193 = CARTESIAN_POINT ( 'NONE',  ( 928.0249999999991815, 219.9999999999998863, -360.0000000000000000 ) ) ;
#40194 = CARTESIAN_POINT ( 'NONE',  ( 769.1273215169530886, -358.7146871989592114, 317.4527132478988847 ) ) ;
#40195 = CARTESIAN_POINT ( 'NONE',  ( 180.7583438952258348, 394.6698570112193920, -224.9999999999999716 ) ) ;
#40196 = LINE ( 'NONE', #2060, #40112 ) ;
#40197 = EDGE_CURVE ( 'NONE', #14073, #811, #34794, .T. ) ;
#40198 = CIRCLE ( 'NONE', #33553, 10.00000000000000888 ) ;
#40199 = CARTESIAN_POINT ( 'NONE',  ( 783.0745993439762742, -200.1908817542436907, 365.1016975059196739 ) ) ;
#40200 = CARTESIAN_POINT ( 'NONE',  ( 804.9363028652555840, -40.27096629478405987, 338.2165204200192079 ) ) ;
#40201 = ORIENTED_EDGE ( 'NONE', *, *, #9440, .T. ) ;
#40202 = CARTESIAN_POINT ( 'NONE',  ( 746.4236121716829757, -399.8272453906067767, -328.8385539511384650 ) ) ;
#40203 = CARTESIAN_POINT ( 'NONE',  ( 763.2262854647970016, -32.63460265842044095, -309.2812353651462445 ) ) ;
#40204 = CARTESIAN_POINT ( 'NONE',  ( 790.8726784830453198, -226.7146871989596661, 362.5472867521010585 ) ) ;
#40205 = CARTESIAN_POINT ( 'NONE',  ( 759.9864689768902508, -410.0891481129647218, -354.9819416627836404 ) ) ;
#40206 = CARTESIAN_POINT ( 'NONE',  ( 805.1927285166399315, -16.81642084023867412, -341.8018195045277707 ) ) ;
#40207 = CARTESIAN_POINT ( 'NONE',  ( 763.0537975583475827, -432.4527844766008684, 371.0346526505627480 ) ) ;
#40208 = CARTESIAN_POINT ( 'NONE',  ( 799.9999999999993179, -512.9681489794448908, -329.9999999999999432 ) ) ;
#40209 = CARTESIAN_POINT ( 'NONE',  ( 802.5472867521000353, -244.3726999360617924, -350.8726784830461156 ) ) ;
#40210 = CARTESIAN_POINT ( 'NONE',  ( 815.2698199232961542, -160.8164208402382371, -342.5225473063383106 ) ) ;
#40211 = CIRCLE ( 'NONE', #6265, 10.00000000000000888 ) ;
#40212 = CARTESIAN_POINT ( 'NONE',  ( 745.4481719005789273, -51.72551174932946338, 347.5162901302853129 ) ) ;
#40213 = CARTESIAN_POINT ( 'NONE',  ( 745.4481719005789273, -123.7255117493292147, 347.5162901302853129 ) ) ;
#40214 = DIRECTION ( 'NONE',  ( -1.084653538143406060E-16, 0.6594541114781790059, 0.7517448203044204691 ) ) ;
#40215 = VECTOR ( 'NONE', #17308, 1000.000000000000000 ) ;
#40216 = PLANE ( 'NONE',  #26901 ) ;
#40217 = EDGE_CURVE ( 'NONE', #14175, #24400, #31482, .T. ) ;
#40218 = CIRCLE ( 'NONE', #38737, 8.024999999999948841 ) ;
#40219 = CARTESIAN_POINT ( 'NONE',  ( 749.5768839229115201, -372.5545181178796383, 358.0661480581553064 ) ) ;
#40220 = ADVANCED_FACE ( 'NONE', ( #7417, #32120 ), #14116, .F. ) ;
#40221 = DIRECTION ( 'NONE',  ( -1.000000000000000000, 0.000000000000000000, 0.000000000000000000 ) ) ;
#40222 = CARTESIAN_POINT ( 'NONE',  ( 796.9462024416508257, -348.4527844766012663, 308.9653473494370246 ) ) ;
#40223 = CARTESIAN_POINT ( 'NONE',  ( 804.9363028652555840, -328.2709662947831362, -338.2165204200192079 ) ) ;
#40224 = CARTESIAN_POINT ( 'NONE',  ( 803.4237431249931660, -447.1800572038736732, 331.2633955100225194 ) ) ;
#40225 = CIRCLE ( 'NONE', #26195, 30.00000000000008171 ) ;
#40226 = CARTESIAN_POINT ( 'NONE',  ( 750.9282345327678740, -112.9181544815167229, -319.8311093483690115 ) ) ;
#40227 = CARTESIAN_POINT ( 'NONE',  ( 784.0799538623451781, -107.8055962898691433, -364.6971507214555572 ) ) ;
#40228 = CARTESIAN_POINT ( 'NONE',  ( 748.3538107759620743, -136.7146871989600072, 355.8262568251490165 ) ) ;
#40229 = CARTESIAN_POINT ( 'NONE',  ( 788.8264449731201466, -429.1800572038737300, 363.6646147819170665 ) ) ;
#40230 = AXIS2_PLACEMENT_3D ( 'NONE', #13295, #20660, #13068 ) ;
#40231 = CARTESIAN_POINT ( 'NONE',  ( 749.8865473780648472, -164.5328690171416781, 322.1177392798429082 ) ) ;
#40232 = CARTESIAN_POINT ( 'NONE',  ( 765.0180583372156207, -24.99823902205683268, -360.0135310231089534 ) ) ;
#40233 = CARTESIAN_POINT ( 'NONE',  ( 755.0488828828309806, -137.8055962898690154, -344.1219089521771934 ) ) ;
#40234 = CARTESIAN_POINT ( 'NONE',  ( 759.7806653035534055, -126.9982390220565094, -324.8639956371180801 ) ) ;
#40235 = CARTESIAN_POINT ( 'NONE',  ( 804.4286716492782716, -137.3618753856928265, 345.3141322388244703 ) ) ;
#40236 = VECTOR ( 'NONE', #8645, 1000.000000000000000 ) ;
#40237 = CARTESIAN_POINT ( 'NONE',  ( 776.9566956441375396, -420.8965053807772279, -364.8461984189686405 ) ) ;
#40239 = CARTESIAN_POINT ( 'NONE',  ( 768.0187753319979720, -248.6346026584197659, 318.0580252608186242 ) ) ;
#40238 = CARTESIAN_POINT ( 'NONE',  ( 795.1360043628807261, -260.0891481129650060, 360.2193346964456282 ) ) ;
#40240 = PLANE ( 'NONE',  #33752 ) ;
#40241 = ORIENTED_EDGE ( 'NONE', *, *, #45565, .F. ) ;
#40242 = CARTESIAN_POINT ( 'NONE',  ( 776.9566956441375396, 11.10349461922141145, 364.8461984189686405 ) ) ;
#40243 = CARTESIAN_POINT ( 'NONE',  ( 768.9521613784389729, -273.8272453906071746, -373.2346286133773106 ) ) ;
#40244 = EDGE_CURVE ( 'NONE', #4463, #29001, #28886, .T. ) ;
#40245 = VERTEX_POINT ( 'NONE', #714 ) ;
#40246 = DIRECTION ( 'NONE',  ( 0.000000000000000000, 0.000000000000000000, -1.000000000000000000 ) ) ;
#40247 = CARTESIAN_POINT ( 'NONE',  ( 787.5162901302840055, -179.3618753856927128, 305.4481719005793252 ) ) ;
#40248 = EDGE_CURVE ( 'NONE', #13947, #30459, #28189, .T. ) ;
#40249 = CARTESIAN_POINT ( 'NONE',  ( 800.9840315886518738, -292.9181544815162397, 354.1144889064786412 ) ) ;
#40250 = CARTESIAN_POINT ( 'NONE',  ( 798.7617431975189675, -411.6237781080499758, 323.0428371773161871 ) ) ;
#40251 = EDGE_LOOP ( 'NONE', ( #16482, #13707, #407, #12237 ) ) ;
#40252 = CARTESIAN_POINT ( 'NONE',  ( 783.0745993439762742, -80.19088175424411702, -365.1016975059196739 ) ) ;
#40253 = CARTESIAN_POINT ( 'NONE',  ( 762.3223304703356007, -271.5436935675106156, -322.3223304703362828 ) ) ;
#40254 = VECTOR ( 'NONE', #17760, 1000.000000000000000 ) ;
#40255 = ORIENTED_EDGE ( 'NONE', *, *, #17246, .T. ) ;
#40256 = CARTESIAN_POINT ( 'NONE',  ( 771.2633955100217236, -407.9073299311465348, -363.4237431249939618 ) ) ;
#40257 = CARTESIAN_POINT ( 'NONE',  ( 756.5762568750052424, -51.18005720387493085, -348.7366044899774238 ) ) ;
#40258 = VECTOR ( 'NONE', #13546, 1000.000000000000000 ) ;
#40259 = CARTESIAN_POINT ( 'NONE',  ( 796.7845633553578182, -273.6237781080504305, 358.5707757039688204 ) ) ;
#40260 = LINE ( 'NONE', #36777, #42517 ) ;
#40261 = AXIS2_PLACEMENT_3D ( 'NONE', #39413, #11691, #25764 ) ;
#40262 = FACE_OUTER_BOUND ( 'NONE', #3439, .T. ) ;
#40263 = EDGE_CURVE ( 'NONE', #36235, #3824, #31877, .T. ) ;
#40264 = CARTESIAN_POINT ( 'NONE',  ( 783.7953271457878373, -8.190881754244330182, -375.1787889125761239 ) ) ;
#40265 = FACE_BOUND ( 'NONE', #18782, .T. ) ;
#40266 = ORIENTED_EDGE ( 'NONE', *, *, #23550, .T. ) ;
#40267 = CARTESIAN_POINT ( 'NONE',  ( 754.3581564841646241, -305.4636090269706870, -316.1443688327762516 ) ) ;
#40268 = CARTESIAN_POINT ( 'NONE',  ( 788.6739635108323228, -175.6454272087892718, 373.9316612368139090 ) ) ;
#40269 = VECTOR ( 'NONE', #30313, 1000.000000000000000 ) ;
#40271 = CARTESIAN_POINT ( 'NONE',  ( 755.5713283507202505, -293.3618753856923718, -334.6858677611754729 ) ) ;
#40270 = FACE_OUTER_BOUND ( 'NONE', #5640, .T. ) ;
#40272 = CARTESIAN_POINT ( 'NONE',  ( 787.5531968255692163, -165.8272453906074873, -316.1348686366205811 ) ) ;
#40273 = VECTOR ( 'NONE', #17007, 1000.000000000000000 ) ;
#40274 = CARTESIAN_POINT ( 'NONE',  ( 767.7687537140311633, -23.90732993114773919, 372.7932403749916830 ) ) ;
#40275 = DIRECTION ( 'NONE',  ( -4.625929269271485914E-16, 1.000000000000000000, 0.000000000000000000 ) ) ;
#40276 = CARTESIAN_POINT ( 'NONE',  ( 746.7653713866222915, -17.26014174441486659, -351.0478386215610271 ) ) ;
#40277 = CARTESIAN_POINT ( 'NONE',  ( 792.3570229623691148, -333.1800572038740142, -373.1304606946836770 ) ) ;
#40278 = DIRECTION ( 'NONE',  ( 0.000000000000000000, 0.000000000000000000, 1.000000000000000000 ) ) ;
#40279 = CARTESIAN_POINT ( 'NONE',  ( 802.1676090361156639, -38.63460265842041252, 327.8955696845344505 ) ) ;
#40280 = CARTESIAN_POINT ( 'NONE',  ( 745.1792804349281596, -302.1908817542433781, 343.7566961878542884 ) ) ;
#40281 = CARTESIAN_POINT ( 'NONE',  ( 758.8095938919642549, -272.0891481129651197, 311.6929314249763365 ) ) ;
#40282 = CARTESIAN_POINT ( 'NONE',  ( 798.0661480581538854, -434.5328690171407970, -309.5768839229118043 ) ) ;
#40283 = DIRECTION ( 'NONE',  ( -1.000000000000000000, -0.000000000000000000, -0.000000000000000000 ) ) ;
#40284 = ORIENTED_EDGE ( 'NONE', *, *, #23827, .T. ) ;
#40285 = CARTESIAN_POINT ( 'NONE',  ( 774.6858677611749044, -369.7255117493284615, 315.5713283507209894 ) ) ;
#40286 = CARTESIAN_POINT ( 'NONE',  ( 754.7162404726377645, -110.7363362996985501, 339.4709603349214717 ) ) ;
#40287 = CARTESIAN_POINT ( 'NONE',  ( 761.2382568024794409, -15.62377810805123524, -356.9571628226838129 ) ) ;
#40288 = AXIS2_PLACEMENT_3D ( 'NONE', #34722, #16488, #17414 ) ;
#40289 = CARTESIAN_POINT ( 'NONE',  ( -37.63011601220122770, -365.3551492539851893, -8.132432514707076621 ) ) ;
#40290 = CARTESIAN_POINT ( 'NONE',  ( 939.9999999999993179, -590.0000000000001137, -350.0000000000000000 ) ) ;
#40291 = CARTESIAN_POINT ( 'NONE',  ( 808.7758568127978833, -124.1692326535054463, 320.0363995740631822 ) ) ;
#40292 = CARTESIAN_POINT ( 'NONE',  ( 774.6312213355099630, -383.3618753856921444, 364.6798772138717482 ) ) ;
#40293 = ORIENTED_EDGE ( 'NONE', *, *, #9416, .F. ) ;
#40294 = CARTESIAN_POINT ( 'NONE',  ( 791.9812246680005501, -44.63460265842040542, -361.9419747391813189 ) ) ;
#40295 = VECTOR ( 'NONE', #29245, 1000.000000000000000 ) ;
#40296 = CARTESIAN_POINT ( 'NONE',  ( 786.6156483768007774, -337.4419599262319593, -315.5913626894246136 ) ) ;
#40297 = CARTESIAN_POINT ( 'NONE',  ( 771.1735550268778070, -153.1800572038746395, 316.3353852180827630 ) ) ;
#40298 = UNCERTAINTY_MEASURE_WITH_UNIT (LENGTH_MEASURE( 1.000000000000000082E-05 ), #17635, 'distance_accuracy_value', 'NONE');
#40299 = CARTESIAN_POINT ( 'NONE',  ( 815.0009284576459549, -318.3510508353230080, -338.7629533639073429 ) ) ;
#40300 = FACE_BOUND ( 'NONE', #18948, .T. ) ;
#40301 = ORIENTED_EDGE ( 'NONE', *, *, #22159, .F. ) ;
#40302 = CARTESIAN_POINT ( 'NONE',  ( 785.3687786644884454, -347.3618753856922012, 315.3201227861279676 ) ) ;
#40303 = VECTOR ( 'NONE', #28115, 1000.000000000000000 ) ;
#40304 = ADVANCED_FACE ( 'NONE', ( #24723 ), #32582, .F. ) ;
#40305 = ORIENTED_EDGE ( 'NONE', *, *, #17027, .F. ) ;
#40306 = CARTESIAN_POINT ( 'NONE',  ( 774.6312213355099630, -431.3618753856918033, 364.6798772138717482 ) ) ;
#40307 = AXIS2_PLACEMENT_3D ( 'NONE', #247, #23406, #34031 ) ;
#40308 = CARTESIAN_POINT ( 'NONE',  ( 763.2262854647970016, -176.6346026584199933, -309.2812353651462445 ) ) ;
#40309 = CARTESIAN_POINT ( 'NONE',  ( 759.0252816721024374, -72.99823902205667991, 368.0189434323527280 ) ) ;
#40310 = VERTEX_POINT ( 'NONE', #38594 ) ;
#40311 = CARTESIAN_POINT ( 'NONE',  ( 755.0636971347428243, -172.2709662947836478, -341.7834795799807353 ) ) ;
#40312 = VERTEX_POINT ( 'NONE', #11105 ) ;
#40313 = CARTESIAN_POINT ( 'NONE',  ( 801.5560724626406000, -408.5545181178794110, -326.7756240680316182 ) ) ;
#40314 = CARTESIAN_POINT ( 'NONE',  ( 797.8594530101008786, 10.45630643248850866, 322.1405469898980982 ) ) ;
#40315 = CARTESIAN_POINT ( 'NONE',  ( 772.5602148656447525, -225.7255117493289163, 305.7998596910095443 ) ) ;
#40316 = CARTESIAN_POINT ( 'NONE',  ( 773.3843516231979720, -157.4419599262326130, 364.4086373105754433 ) ) ;
#40319 = CARTESIAN_POINT ( 'NONE',  ( 798.0661480581538854, -410.5328690171408539, 309.5768839229118043 ) ) ;
#40318 = LINE ( 'NONE', #36613, #11537 ) ;
#40317 = CYLINDRICAL_SURFACE ( 'NONE', #15223, 6.119000000000013095 ) ;
#40320 = VERTEX_POINT ( 'NONE', #7641 ) ;
#40321 = CARTESIAN_POINT ( 'NONE',  ( 796.1575198192839480, -414.0090635724249637, -359.4546378042384163 ) ) ;
#40322 = CARTESIAN_POINT ( 'NONE',  ( 571.1634899080285095, 239.9999999999999432, -202.7499999999980105 ) ) ;
#40323 = CARTESIAN_POINT ( 'NONE',  ( 745.5313806188320314, -207.2817908451527842, -333.7943932421247268 ) ) ;
#40324 = CARTESIAN_POINT ( 'NONE',  ( 755.8990559732751535, -59.46360902697142592, 365.9055244015606831 ) ) ;
#40325 = AXIS2_PLACEMENT_3D ( 'NONE', #33767, #1880, #44379 ) ;
#40327 = CARTESIAN_POINT ( 'NONE',  ( 768.0187753319979720, -176.6346026584199933, -318.0580252608186242 ) ) ;
#40326 = DIRECTION ( 'NONE',  ( -0.000000000000000000, 1.000000000000000000, -0.000000000000000000 ) ) ;
#40328 = CARTESIAN_POINT ( 'NONE',  ( 805.1016975059191054, -342.8965053807773984, -343.0745993439771837 ) ) ;
#40329 = DIRECTION ( 'NONE',  ( 1.000000000000000000, 0.000000000000000000, 0.000000000000000000 ) ) ;
#40330 = CARTESIAN_POINT ( 'NONE',  ( 745.7194118038753459, -229.6454272087890729, -348.7631598425976449 ) ) ;
#40331 = CARTESIAN_POINT ( 'NONE',  ( 791.6690787386836519, -454.6466601436378028, 367.6383479129825673 ) ) ;
#40332 = FACE_BOUND ( 'NONE', #32906, .T. ) ;
#40333 = CARTESIAN_POINT ( 'NONE',  ( 755.3028492785439312, -39.28179084515331709, -335.9200461376539693 ) ) ;
#40334 = VECTOR ( 'NONE', #17176, 1000.000000000000000 ) ;
#40335 = CARTESIAN_POINT ( 'NONE',  ( 805.2837595273609850, -410.7363362996976548, 340.5290396650784714 ) ) ;
#40336 = CARTESIAN_POINT ( 'NONE',  ( 767.6429770376291799, -225.1800572038743553, -306.8695393053162093 ) ) ;
#40337 = CARTESIAN_POINT ( 'NONE',  ( 804.4086373105744769, -241.6454272087890729, 333.3843516231986541 ) ) ;
#40338 = DIRECTION ( 'NONE',  ( -0.000000000000000000, 1.000000000000000000, -0.000000000000000000 ) ) ;
#40339 = CARTESIAN_POINT ( 'NONE',  ( 778.1981804954714335, -10.27096629478414691, -314.8072714833589885 ) ) ;
#40340 = CARTESIAN_POINT ( 'NONE',  ( 752.7379699480933368, -180.0090635724255890, 361.9858362298580232 ) ) ;
#40341 = CARTESIAN_POINT ( 'NONE',  ( 749.8865473780648472, -140.5328690171417634, -322.1177392798429082 ) ) ;
#40342 = CARTESIAN_POINT ( 'NONE',  ( 814.9108240113580450, -160.2709662947836762, 337.5031285880265273 ) ) ;
#40343 = CARTESIAN_POINT ( 'NONE',  ( 745.4481719005789273, -387.7255117493283478, -347.5162901302853129 ) ) ;
#40344 = CARTESIAN_POINT ( 'NONE',  ( 799.9999999999993179, -512.9681489794448908, 329.9999999999999432 ) ) ;
#40345 = CARTESIAN_POINT ( 'NONE',  ( 181.1634899080285948, 260.0000000000000000, -199.9999999999953957 ) ) ;
#40346 = CARTESIAN_POINT ( 'NONE',  ( 771.2633955100217236, -239.9073299311470748, 363.4237431249939618 ) ) ;
#40347 = CARTESIAN_POINT ( 'NONE',  ( 757.0176451133909268, -13.09997266333522248, 349.9200121543848354 ) ) ;
#40348 = CARTESIAN_POINT ( 'NONE',  ( 803.4237431249931660, -399.1800572038738437, -331.2633955100225194 ) ) ;
#40349 = LINE ( 'NONE', #33620, #9950 ) ;
#40350 = CARTESIAN_POINT ( 'NONE',  ( 782.4968714119720516, -442.8164208402372992, -305.0891759886411023 ) ) ;
#40351 = DIRECTION ( 'NONE',  ( -0.000000000000000000, -0.000000000000000000, -1.000000000000000000 ) ) ;
#40352 = CARTESIAN_POINT ( 'NONE',  ( 772.3691319403857278, -71.26014174441469606, 315.8894580844506663 ) ) ;
#40353 = ORIENTED_EDGE ( 'NONE', *, *, #8889, .F. ) ;
#40354 = CARTESIAN_POINT ( 'NONE',  ( 799.4546378042377910, -225.0783235625959833, -356.1575198192848006 ) ) ;
#40355 = CARTESIAN_POINT ( 'NONE',  ( 800.0135310231082713, -62.08914811296580183, 325.0180583372163028 ) ) ;
#40356 = CARTESIAN_POINT ( 'NONE',  ( 759.8311093483677041, -214.1692326535052189, -310.9282345327691814 ) ) ;
#40357 =( LENGTH_UNIT ( ) NAMED_UNIT ( * ) SI_UNIT ( .MILLI., .METRE. ) );
#40358 = CARTESIAN_POINT ( 'NONE',  ( 756.1443688327750579, -333.6237781080502600, 314.3581564841659315 ) ) ;
#40359 = ORIENTED_EDGE ( 'NONE', *, *, #40263, .T. ) ;
#40360 = CIRCLE ( 'NONE', #20415, 10.00000000000000888 ) ;
#40361 = CARTESIAN_POINT ( 'NONE',  ( 802.7791456095903868, -28.71468719896028077, -329.0155153010375102 ) ) ;
#40362 = CARTESIAN_POINT ( 'NONE',  ( 756.3353852180819104, -341.9073299311465917, 331.1735550268788302 ) ) ;
#40363 = AXIS2_PLACEMENT_3D ( 'NONE', #2704, #33657, #37574 ) ;
#40364 = CARTESIAN_POINT ( 'NONE',  ( 782.5225473063381969, -70.27096629478397460, -375.2698199232970637 ) ) ;
#40365 = CARTESIAN_POINT ( 'NONE',  ( 802.1676090361155502, -86.63460265842024910, -327.8955696845344505 ) ) ;
#40366 = ORIENTED_EDGE ( 'NONE', *, *, #14121, .F. ) ;
#40367 = CARTESIAN_POINT ( 'NONE',  ( 790.9844846989617508, -22.37269993606246743, -317.2208543904092721 ) ) ;
#40368 = VECTOR ( 'NONE', #11163, 1000.000000000000114 ) ;
#40369 = EDGE_LOOP ( 'NONE', ( #35168, #17393, #32176, #18927, #21960, #12341 ) ) ;
#40370 = CARTESIAN_POINT ( 'NONE',  ( 759.0159684113467620, -304.9181544815161828, -325.8855110935213020 ) ) ;
#40372 = CARTESIAN_POINT ( 'NONE',  ( 802.5472867521000353, -364.3726999360614514, 350.8726784830461156 ) ) ;
#40371 = CARTESIAN_POINT ( 'NONE',  ( 794.9819416627830151, -60.99823902205671544, 319.9864689768909898 ) ) ;
#40373 = VECTOR ( 'NONE', #32476, 1000.000000000000000 ) ;
#40376 = CARTESIAN_POINT ( 'NONE',  ( 773.7943932421234194, -311.8055962898685038, 305.5313806188329409 ) ) ;
#40375 = CARTESIAN_POINT ( 'NONE',  ( 939.9999999999992042, 56.73212367640090292, -362.5753187112032947 ) ) ;
#40374 = CARTESIAN_POINT ( 'NONE',  ( 796.7737145352015204, -428.6346026584192259, 370.7187646348536987 ) ) ;
#40377 = CARTESIAN_POINT ( 'NONE',  ( 795.6651683502461765, -106.7146871989600498, 371.3240766477733814 ) ) ;
#40378 = CARTESIAN_POINT ( 'NONE',  ( 804.6971507214547046, -339.2817908451524431, -344.0799538623459739 ) ) ;
#40379 = CARTESIAN_POINT ( 'NONE',  ( 804.9363028652555840, -328.2709662947831362, -338.2165204200192079 ) ) ;
#40380 = CARTESIAN_POINT ( 'NONE',  ( 778.2165204200184689, -142.8164208402382656, -364.9363028652563230 ) ) ;
#40381 = CARTESIAN_POINT ( 'NONE',  ( 754.9967657858570647, -409.5436935675101040, 365.0032342141425374 ) ) ;
#40383 = DIRECTION ( 'NONE',  ( 0.000000000000000000, 0.000000000000000000, -1.000000000000000000 ) ) ;
#40382 = CARTESIAN_POINT ( 'NONE',  ( 998.9999999999992042, -600.0000000000001137, 360.0000000000000000 ) ) ;
#40384 = CARTESIAN_POINT ( 'NONE',  ( 799.9636004259356241, -118.9181544815167229, -311.2241431872006956 ) ) ;
#40385 = DIRECTION ( 'NONE',  ( -1.000000000000000000, 1.892425610156518354E-16, 0.000000000000000000 ) ) ;
#40386 = DIRECTION ( 'NONE',  ( -1.000000000000000000, -0.000000000000000000, 0.000000000000000000 ) ) ;
#40387 = CARTESIAN_POINT ( 'NONE',  ( 801.5560724626406000, -312.5545181178797520, 326.7756240680316182 ) ) ;
#40388 = CARTESIAN_POINT ( 'NONE',  ( 755.5713283507202505, -173.3618753856927128, 334.6858677611754729 ) ) ;
#40389 = ORIENTED_EDGE ( 'NONE', *, *, #35177, .T. ) ;
#40390 = CARTESIAN_POINT ( 'NONE',  ( 808.0189434323515343, -134.0891481129655745, -319.0252816721025511 ) ) ;
#40391 = CARTESIAN_POINT ( 'NONE',  ( 775.4999999999993179, -512.9681489794448908, -339.9999999999999432 ) ) ;
#40392 = CARTESIAN_POINT ( 'NONE',  ( 812.3518521366052028, -73.09997266333502353, 326.5853460496235243 ) ) ;
#40393 = CARTESIAN_POINT ( 'NONE',  ( 772.5602148656447525, -273.7255117493288026, -305.7998596910095443 ) ) ;
#40394 = CARTESIAN_POINT ( 'NONE',  ( 787.5162901302840055, -443.3618753856917465, -305.4481719005793252 ) ) ;
#40395 = CARTESIAN_POINT ( 'NONE',  ( 805.1927285166397041, -136.8164208402382371, 341.8018195045277707 ) ) ;
#40396 = ORIENTED_EDGE ( 'NONE', *, *, #37597, .F. ) ;
#40397 = CARTESIAN_POINT ( 'NONE',  ( 783.7566961878529810, -336.8965053807774552, -305.1792804349288417 ) ) ;
#40398 = AXIS2_PLACEMENT_3D ( 'NONE', #29216, #1024, #29437 ) ;
#40399 = CARTESIAN_POINT ( 'NONE',  ( 748.9653473494363425, -74.63460265842032015, -356.9462024416521331 ) ) ;
#40400 = CARTESIAN_POINT ( 'NONE',  ( 800.9840315886518738, -4.918154481517067467, 354.1144889064786412 ) ) ;
#40401 = CARTESIAN_POINT ( 'NONE',  ( 792.2312462859673587, -347.9073299311467053, -307.2067596250082602 ) ) ;
#40402 = CARTESIAN_POINT ( 'NONE',  ( 759.9999999999992042, 205.0000000000000568, -329.9999999999999432 ) ) ;
#40403 = CARTESIAN_POINT ( 'NONE',  ( 789.9200121543843807, -409.9874144716863498, 317.0176451133914384 ) ) ;
#40404 = EDGE_LOOP ( 'NONE', ( #21449, #37386, #29041, #2265 ) ) ;
#40405 = CARTESIAN_POINT ( 'NONE',  ( 779.4709603349208464, -72.35105083532378956, 314.7162404726379918 ) ) ;
#40406 = CARTESIAN_POINT ( 'NONE',  ( 756.1443688327750579, -117.6237781080509279, -314.3581564841659315 ) ) ;
#40407 = FACE_OUTER_BOUND ( 'NONE', #33015, .T. ) ;
#40408 = CARTESIAN_POINT ( 'NONE',  ( 773.7943932421234194, -239.8055962898687028, 305.5313806188329409 ) ) ;
#40409 = CARTESIAN_POINT ( 'NONE',  ( 800.2193346964446619, -66.99823902205670834, 355.1360043628816925 ) ) ;
#40410 = ORIENTED_EDGE ( 'NONE', *, *, #4111, .F. ) ;
#40411 = CARTESIAN_POINT ( 'NONE',  ( 754.8072714833581358, -244.8164208402378961, 338.1981804954720587 ) ) ;
#40412 = CARTESIAN_POINT ( 'NONE',  ( 788.7631598425961101, -433.4419599262316183, -305.7194118038759143 ) ) ;
#40413 = CARTESIAN_POINT ( 'NONE',  ( 747.3154664389472828, -67.98741447168742980, -326.4474001241230781 ) ) ;
#40414 = LINE ( 'NONE', #15684, #23175 ) ;
#40415 = ORIENTED_EDGE ( 'NONE', *, *, #28049, .F. ) ;
#40416 = ORIENTED_EDGE ( 'NONE', *, *, #35917, .F. ) ;
#40417 = CARTESIAN_POINT ( 'NONE',  ( 777.5031285880264704, -334.8164208402376403, 374.9108240113588408 ) ) ;
#40418 = CARTESIAN_POINT ( 'NONE',  ( 791.1614460488616487, -35.26014174441480264, 373.5763878283158874 ) ) ;
#40419 = CARTESIAN_POINT ( 'NONE',  ( 758.4439275373578084, -204.5545181178800931, -353.2243759319684386 ) ) ;
#40420 = CARTESIAN_POINT ( 'NONE',  ( 792.1044303154645831, -228.4527844766015789, -317.8323909638837677 ) ) ;
#40421 = CARTESIAN_POINT ( 'NONE',  ( 794.9819416627830151, -372.9982390220557704, -319.9864689768909898 ) ) ;
#40422 = ORIENTED_EDGE ( 'NONE', *, *, #4401, .F. ) ;
#40423 = CARTESIAN_POINT ( 'NONE',  ( 785.3687786644884454, -107.3618753856928976, -315.3201227861279676 ) ) ;
#40424 = ORIENTED_EDGE ( 'NONE', *, *, #39851, .T. ) ;
#40425 = CIRCLE ( 'NONE', #30087, 2.749999999999863665 ) ;
#40426 = CARTESIAN_POINT ( 'NONE',  ( 745.4481719005789273, -339.7255117493285184, 347.5162901302853129 ) ) ;
#40427 = FACE_OUTER_BOUND ( 'NONE', #31471, .T. ) ;
#40428 = DIRECTION ( 'NONE',  ( -1.236450975029139710E-16, 0.7517448203044212462, -0.6594541114781782287 ) ) ;
#40429 = DIRECTION ( 'NONE',  ( -1.000000000000000000, -0.000000000000000000, -0.000000000000000000 ) ) ;
#40430 = CARTESIAN_POINT ( 'NONE',  ( 766.9102291470427417, -186.5545181178801215, 318.6633372737382501 ) ) ;
#40431 = CARTESIAN_POINT ( 'NONE',  ( 778.2165204200184689, -94.81642084023843609, 364.9363028652563230 ) ) ;
#40432 = ORIENTED_EDGE ( 'NONE', *, *, #42547, .F. ) ;
#40433 = CARTESIAN_POINT ( 'NONE',  ( 766.9102291470427417, 5.445481882119263872, -318.6633372737382501 ) ) ;
#40434 = CARTESIAN_POINT ( 'NONE',  ( 751.9810565676468741, -50.08914811296584446, -360.9747183278973921 ) ) ;
#40435 = CARTESIAN_POINT ( 'NONE',  ( 755.8398074228967971, -259.4419599262322436, 333.4516893846970333 ) ) ;
#40436 = CARTESIAN_POINT ( 'NONE',  ( 768.0187753319979720, -392.6346026584193396, -318.0580252608186242 ) ) ;
#40437 = CARTESIAN_POINT ( 'NONE',  ( 771.2633955100217236, 0.09267006885218045942, -363.4237431249939618 ) ) ;
#40438 = CARTESIAN_POINT ( 'NONE',  ( 800.9747183278959710, -420.9982390220555999, 311.9810565676471583 ) ) ;
#40439 = CARTESIAN_POINT ( 'NONE',  ( -728.8365100919714905, 260.0000000000001705, -202.7499999999889440 ) ) ;
#40440 = CARTESIAN_POINT ( 'NONE',  ( 798.5707757039680246, -269.4636090269708006, -356.7845633553585003 ) ) ;
#40441 = CARTESIAN_POINT ( 'NONE',  ( 759.0252816721024374, -168.9982390220563673, -368.0189434323527280 ) ) ;
#40442 = CARTESIAN_POINT ( 'NONE',  ( 745.0891759886404770, -52.27096629478401724, 342.4968714119734159 ) ) ;
#40443 = CARTESIAN_POINT ( 'NONE',  ( 805.0032342141412300, -157.5436935675108998, 314.9967657858571783 ) ) ;
#40444 = CARTESIAN_POINT ( 'NONE',  ( 774.9293440288117836, 16.45630643248849623, -314.9535949064562601 ) ) ;
#40445 = CARTESIAN_POINT ( 'NONE',  ( 989.9999999999992042, -590.0000000000001137, 350.0000000000000000 ) ) ;
#40446 = CARTESIAN_POINT ( 'NONE',  ( 815.2698199232961542, -352.8164208402374129, 342.5225473063383106 ) ) ;
#40447 = CARTESIAN_POINT ( 'NONE',  ( 800.0135310231082713, -326.0891481129649492, -325.0180583372163028 ) ) ;
#40448 = ADVANCED_FACE ( 'NONE', ( #42522 ), #7889, .F. ) ;
#40449 = CARTESIAN_POINT ( 'NONE',  ( 802.7791456095903868, 19.28531280103956647, 329.0155153010375102 ) ) ;
#40450 = CARTESIAN_POINT ( 'NONE',  ( 814.4686193811664907, -99.28179084515313946, -346.2056067578752732 ) ) ;
#40451 = CARTESIAN_POINT ( 'NONE',  ( 780.5290396650775619, -132.3510508353235764, -365.2837595273619513 ) ) ;
#40452 = CARTESIAN_POINT ( 'NONE',  ( 776.2433038121456548, -132.8965053807781374, 374.8207195650711014 ) ) ;
#40453 = CARTESIAN_POINT ( 'NONE',  ( 790.0183182880230106, -452.9681489794449476, 362.9048749981275250 ) ) ;
#40454 = VECTOR ( 'NONE', #4177, 1000.000000000000114 ) ;
#40455 = CARTESIAN_POINT ( 'NONE',  ( 781.8018195045266339, -22.27096629478410250, -365.1927285166406705 ) ) ;
#40456 = CARTESIAN_POINT ( 'NONE',  ( 765.8855110935204493, -142.1692326535054178, -319.0159684113471599 ) ) ;
#40457 = CARTESIAN_POINT ( 'NONE',  ( 791.9812246680005501, -116.6346026584201780, -361.9419747391813189 ) ) ;
#40458 = CARTESIAN_POINT ( 'NONE',  ( 800.2193346964447755, -138.9982390220563957, 355.1360043628815788 ) ) ;
#40459 = EDGE_CURVE ( 'NONE', #2036, #22721, #38888, .T. ) ;
#40460 = CARTESIAN_POINT ( 'NONE',  ( 756.1348686366196716, -425.2601417444136018, -347.5531968255698416 ) ) ;
#40462 = CARTESIAN_POINT ( 'NONE',  ( 774.6858677611749044, -249.7255117493288594, 315.5713283507209894 ) ) ;
#40461 = CARTESIAN_POINT ( 'NONE',  ( 804.4286716492782716, -257.3618753856924286, 345.3141322388244703 ) ) ;
#40463 = DIRECTION ( 'NONE',  ( 0.000000000000000000, 0.000000000000000000, -1.000000000000000000 ) ) ;
#40464 = ORIENTED_EDGE ( 'NONE', *, *, #36589, .F. ) ;
#40465 = CARTESIAN_POINT ( 'NONE',  ( 755.8398074228967971, 4.558040073766884248, 333.4516893846970333 ) ) ;
#40466 = CARTESIAN_POINT ( 'NONE',  ( 781.2370466360911223, -284.7363362996979390, -304.9990715423533629 ) ) ;
#40467 = EDGE_LOOP ( 'NONE', ( #44305, #40728, #760, #28241 ) ) ;
#40468 = DIRECTION ( 'NONE',  ( 1.000000000000000000, 0.000000000000000000, 0.000000000000000000 ) ) ;
#40469 = CARTESIAN_POINT ( 'NONE',  ( 763.0537975583476964, -216.4527844766016926, 371.0346526505628617 ) ) ;
#40470 = CARTESIAN_POINT ( 'NONE',  ( 779.4763451958990572, -296.7363362996979390, 365.0264073115438919 ) ) ;
#40471 = CARTESIAN_POINT ( 'NONE',  ( 787.6308680596127942, -395.2601417444136587, 364.1105419155492768 ) ) ;
#40472 = ORIENTED_EDGE ( 'NONE', *, *, #29510, .F. ) ;
#40473 = CARTESIAN_POINT ( 'NONE',  ( 766.0291762391763086, -106.9181544815167371, -360.7704444035551319 ) ) ;
#40474 = CARTESIAN_POINT ( 'NONE',  ( 758.0580252608178853, -270.4527844766014937, -328.0187753319985404 ) ) ;
#40475 = ORIENTED_EDGE ( 'NONE', *, *, #17049, .F. ) ;
#40476 = CARTESIAN_POINT ( 'NONE',  ( 805.1927285166397041, -424.8164208402372992, -341.8018195045277707 ) ) ;
#40477 = CARTESIAN_POINT ( 'NONE',  ( 755.5713283507202505, -101.3618753856929544, -334.6858677611754729 ) ) ;
#40478 = EDGE_CURVE ( 'NONE', #22607, #10815, #24848, .T. ) ;
#40479 = CARTESIAN_POINT ( 'NONE',  ( 780.5290396650775619, -276.3510508353231785, 365.2837595273619513 ) ) ;
#40480 = DIRECTION ( 'NONE',  ( 1.000000000000000000, 0.000000000000000000, 0.000000000000000000 ) ) ;
#40481 = CARTESIAN_POINT ( 'NONE',  ( 754.3581564841646241, -17.46360902697157513, -316.1443688327762516 ) ) ;
#40482 = CARTESIAN_POINT ( 'NONE',  ( -911.9749999999993406, 154.9999999999998863, 339.9999999999999432 ) ) ;
#40483 = VERTEX_POINT ( 'NONE', #21268 ) ;
#40484 = CARTESIAN_POINT ( 'NONE',  ( 748.6759233522253680, -352.3726999360614514, -324.3348316497537098 ) ) ;
#40485 = CARTESIAN_POINT ( 'NONE',  ( 747.6481478633932056, -205.0999726633346256, 353.4146539503763620 ) ) ;
#40486 = VECTOR ( 'NONE', #1513, 1000.000000000000114 ) ;
#40488 = CARTESIAN_POINT ( 'NONE',  ( 757.8323909638827445, -290.6346026584195101, -352.1044303154654358 ) ) ;
#40487 = PLANE ( 'NONE',  #5450 ) ;
#40489 = CARTESIAN_POINT ( 'NONE',  ( 919.9999999999993179, 154.9999999999998863, -350.0000000000000000 ) ) ;
#40490 = CARTESIAN_POINT ( 'NONE',  ( 766.0291762391763086, -154.9181544815165523, -360.7704444035551319 ) ) ;
#40491 = CARTESIAN_POINT ( 'NONE',  ( 751.9810565676468741, -50.08914811296584446, 360.9747183278973921 ) ) ;
#40492 = DIRECTION ( 'NONE',  ( -1.000000000000000000, 0.000000000000000000, 0.000000000000000000 ) ) ;
#40493 = CARTESIAN_POINT ( 'NONE',  ( 777.5031285880264704, -334.8164208402376403, -374.9108240113588408 ) ) ;
#40494 = FACE_OUTER_BOUND ( 'NONE', #36360, .T. ) ;
#40495 = CARTESIAN_POINT ( 'NONE',  ( 803.4237431249931660, -39.18005720387496638, 331.2633955100225194 ) ) ;
#40496 = EDGE_CURVE ( 'NONE', #5848, #15202, #10887, .T. ) ;
#40497 = CARTESIAN_POINT ( 'NONE',  ( 757.7880784355613741, -282.0090635724253048, 312.4576283171834916 ) ) ;
#40498 = CARTESIAN_POINT ( 'NONE',  ( 777.5031285880264704, -262.8164208402379245, 374.9108240113588408 ) ) ;
#40499 = CARTESIAN_POINT ( 'NONE',  ( 810.7187646348534145, 5.547215523397618142, -356.7737145352016341 ) ) ;
#40500 = FACE_BOUND ( 'NONE', #42856, .T. ) ;
#40501 = ADVANCED_FACE ( 'NONE', ( #25175 ), #21033, .T. ) ;
#40502 = LINE ( 'NONE', #12539, #31358 ) ;
#40503 = CARTESIAN_POINT ( 'NONE',  ( 785.3687786644884454, -347.3618753856922012, 315.3201227861279676 ) ) ;
#40504 = CARTESIAN_POINT ( 'NONE',  ( 802.9823548866075953, -121.0999726633348956, 330.0799878456151077 ) ) ;
#40505 = CARTESIAN_POINT ( 'NONE',  ( 802.7791456095903868, -28.71468719896028077, -329.0155153010375102 ) ) ;
#40506 = DIRECTION ( 'NONE',  ( -0.000000000000000000, 1.000000000000000000, -0.000000000000000000 ) ) ;
#40507 = DIRECTION ( 'NONE',  ( 0.000000000000000000, 0.7651688349527167032, -0.6438296778008156807 ) ) ;
#40508 = CARTESIAN_POINT ( 'NONE',  ( 797.6776695296629214, -403.5436935675101608, 357.6776695296636603 ) ) ;
#40509 = ORIENTED_EDGE ( 'NONE', *, *, #35022, .F. ) ;
#40510 = EDGE_CURVE ( 'NONE', #29224, #2171, #21719, .T. ) ;
#40511 = CARTESIAN_POINT ( 'NONE',  ( 790.8726784830453198, -346.7146871989592682, -362.5472867521010585 ) ) ;
#40513 = CARTESIAN_POINT ( 'NONE',  ( 757.8323909638828582, -170.6346026584199933, 352.1044303154654358 ) ) ;
#40512 = CARTESIAN_POINT ( 'NONE',  ( 771.2633955100217236, -167.9073299311473022, 363.4237431249939618 ) ) ;
#40514 = CARTESIAN_POINT ( 'NONE',  ( 764.3348316497523456, -334.7146871989593251, -308.6759233522265617 ) ) ;
#40515 = CARTESIAN_POINT ( 'NONE',  ( 799.9999999999993179, -365.3551492539851893, 18.13243251470705886 ) ) ;
#40516 = VERTEX_POINT ( 'NONE', #24954 ) ;
#40517 = CARTESIAN_POINT ( 'NONE',  ( 781.7834795799800531, -370.8164208402375834, 315.0636971347436202 ) ) ;
#40518 = AXIS2_PLACEMENT_3D ( 'NONE', #4646, #4874, #18522 ) ;
#40519 = VERTEX_POINT ( 'NONE', #4192 ) ;
#40520 =( NAMED_UNIT ( * ) PLANE_ANGLE_UNIT ( ) SI_UNIT ( $, .RADIAN. ) );
#40521 = CARTESIAN_POINT ( 'NONE',  ( 800.9747183278959710, -180.9982390220563389, -311.9810565676471583 ) ) ;
#40522 = CARTESIAN_POINT ( 'NONE',  ( 796.9462024416508257, -108.4527844766020053, 308.9653473494370246 ) ) ;
#40523 = ORIENTED_EDGE ( 'NONE', *, *, #184, .F. ) ;
#40524 = CARTESIAN_POINT ( 'NONE',  ( 804.6798772138710092, -183.7255117493290300, -334.6312213355106451 ) ) ;
#40525 = ORIENTED_EDGE ( 'NONE', *, *, #15904, .T. ) ;
#40526 = EDGE_CURVE ( 'NONE', #10930, #20722, #35121, .T. ) ;
#40527 = CARTESIAN_POINT ( 'NONE',  ( 790.9844846989617508, -454.3726999360611103, -317.2208543904092721 ) ) ;
#40528 = EDGE_CURVE ( 'NONE', #37281, #7806, #1705, .T. ) ;
#40529 = CARTESIAN_POINT ( 'NONE',  ( 805.0032342141412300, -253.5436935675104735, 314.9967657858571783 ) ) ;
#40530 = CARTESIAN_POINT ( 'NONE',  ( 804.9511171171677688, -173.8055962898689302, 335.8780910478229202 ) ) ;
#40532 = DIRECTION ( 'NONE',  ( -0.000000000000000000, -0.000000000000000000, -1.000000000000000000 ) ) ;
#40531 = DIRECTION ( 'NONE',  ( -0.000000000000000000, 1.000000000000000000, -0.000000000000000000 ) ) ;
#40533 = EDGE_LOOP ( 'NONE', ( #29898, #30908, #41646, #26908 ) ) ;
#40534 = CARTESIAN_POINT ( 'NONE',  ( 755.5913626894240451, -445.6454272087883055, -346.6156483768012890 ) ) ;
#40535 = DIRECTION ( 'NONE',  ( -0.000000000000000000, 1.000000000000000000, -0.000000000000000000 ) ) ;
#40536 = CARTESIAN_POINT ( 'NONE',  ( 760.0363995740630116, -202.9181544815164386, -368.7758568127991907 ) ) ;
#40537 = CARTESIAN_POINT ( 'NONE',  ( 783.7953271457878373, -104.1908817542440175, 375.1787889125761239 ) ) ;
#40539 = CARTESIAN_POINT ( 'NONE',  ( 756.3353852180819104, -197.9073299311472169, -331.1735550268788302 ) ) ;
#40538 = CARTESIAN_POINT ( 'NONE',  ( 914.9999999999992042, 99.99999999999984368, 360.0000000000000000 ) ) ;
#40540 = CARTESIAN_POINT ( 'NONE',  ( 770.0799878456142551, -349.9874144716865771, -362.9823548866085616 ) ) ;
#40541 = FACE_OUTER_BOUND ( 'NONE', #12164, .T. ) ;
#40542 = CARTESIAN_POINT ( 'NONE',  ( 762.1177392798416577, -210.5545181178800647, -309.8865473780659272 ) ) ;
#40543 = CARTESIAN_POINT ( 'NONE',  ( 791.8656671112827325, -456.3250812000245560, 367.5545208264068719 ) ) ;
#40544 = CARTESIAN_POINT ( 'NONE',  ( -468.8365100919714337, 258.0940000000001646, -199.9999999999908766 ) ) ;
#40545 = CARTESIAN_POINT ( 'NONE',  ( 776.9254006560222479, -44.19088175424421649, -314.8983024940802125 ) ) ;
#40546 = CARTESIAN_POINT ( 'NONE',  ( 796.1575198192839480, -390.0090635724249069, 359.4546378042384163 ) ) ;
#40547 = CARTESIAN_POINT ( 'NONE',  ( 814.2001403089898304, -233.3618753856925423, -347.4397851343538264 ) ) ;
#40548 = LINE ( 'NONE', #16282, #22414 ) ;
#40549 = DIRECTION ( 'NONE',  ( -0.000000000000000000, -0.6438296778008192334, -0.7651688349527135946 ) ) ;
#40550 = CARTESIAN_POINT ( 'NONE',  ( 754.8072714833581358, -52.81642084023856398, -338.1981804954720587 ) ) ;
#40551 = CIRCLE ( 'NONE', #7352, 2.749999999999919176 ) ;
#40552 = EDGE_CURVE ( 'NONE', #7841, #35164, #16497, .T. ) ;
#40553 = EDGE_CURVE ( 'NONE', #7179, #13769, #40831, .T. ) ;
#40554 = CARTESIAN_POINT ( 'NONE',  ( 797.8822607201568644, -174.5545181178801784, 370.1134526219340160 ) ) ;
#40555 = CARTESIAN_POINT ( 'NONE',  ( 768.8385539511368734, -143.2601417444144829, -306.4236121716840557 ) ) ;
#40556 = CARTESIAN_POINT ( 'NONE',  ( 787.4397851343537695, -141.7255117493291721, 374.2001403089903988 ) ) ;
#40557 = CARTESIAN_POINT ( 'NONE',  ( 810.7187646348534145, -378.4527844766011526, -356.7737145352016341 ) ) ;
#40558 = DIRECTION ( 'NONE',  ( 0.000000000000000000, -0.000000000000000000, 1.000000000000000000 ) ) ;
#40559 = EDGE_CURVE ( 'NONE', #27855, #14164, #8396, .T. ) ;
#40560 = CARTESIAN_POINT ( 'NONE',  ( 794.9819416627830151, -252.9982390220560831, 319.9864689768909898 ) ) ;
#40561 = CARTESIAN_POINT ( 'NONE',  ( 772.4468031744293057, -9.827245390607961539, 363.8651313633793620 ) ) ;
#40562 = CARTESIAN_POINT ( 'NONE',  ( 797.6776695296629214, -403.5436935675101608, -357.6776695296636603 ) ) ;
#40563 = CARTESIAN_POINT ( 'NONE',  ( 454.7528517110262101, 229.9999999999999432, -2132.806278688367456 ) ) ;
#40564 = CARTESIAN_POINT ( 'NONE',  ( 814.5518280994195948, -447.7255117493280636, -332.4837098697145734 ) ) ;
#40565 = CARTESIAN_POINT ( 'NONE',  ( 919.9999999999993179, 154.9999999999998863, -360.0000000000000000 ) ) ;
#40566 = CARTESIAN_POINT ( 'NONE',  ( 755.0488828828309806, -89.80559628986918597, 344.1219089521771934 ) ) ;
#40567 = EDGE_LOOP ( 'NONE', ( #6723, #33151, #41088, #27969 ) ) ;
#40568 = EDGE_CURVE ( 'NONE', #32683, #7811, #36267, .T. ) ;
#40569 = CARTESIAN_POINT ( 'NONE',  ( 795.9930595647434757, -219.0783235625960401, -320.7433823573372820 ) ) ;
#40570 = CARTESIAN_POINT ( 'NONE',  ( 759.9864689768902508, -74.08914811296577341, 354.9819416627836404 ) ) ;
#40571 = CARTESIAN_POINT ( 'NONE',  ( 807.5423716828161105, -225.0783235625959833, -362.2119215644372048 ) ) ;
#40572 = SURFACE_STYLE_USAGE ( .BOTH. , #44476 ) ;
#40573 = CARTESIAN_POINT ( 'NONE',  ( 815.1787889125755555, -342.8965053807773984, 343.7953271457877804 ) ) ;
#40574 = ORIENTED_EDGE ( 'NONE', *, *, #2646, .F. ) ;
#40575 = CARTESIAN_POINT ( 'NONE',  ( 808.7758568127978833, -436.1692326535044231, 320.0363995740631822 ) ) ;
#40576 = CARTESIAN_POINT ( 'NONE',  ( 791.9812246680005501, -140.6346026584201070, -361.9419747391813189 ) ) ;
#40577 = CARTESIAN_POINT ( 'NONE',  ( 792.1044303154645831, -372.4527844766010958, 317.8323909638837677 ) ) ;
#40578 = CARTESIAN_POINT ( 'NONE',  ( 814.2001403089898304, -65.36187538569306810, -347.4397851343538264 ) ) ;
#40579 = CARTESIAN_POINT ( 'NONE',  ( 762.1405469898973024, -73.54369356751121245, -357.8594530101016176 ) ) ;
#40580 = ORIENTED_EDGE ( 'NONE', *, *, #17924, .F. ) ;
#40581 = CARTESIAN_POINT ( 'NONE',  ( 800.9840315886518738, -4.918154481517067467, -354.1144889064786412 ) ) ;
#40582 = ORIENTED_EDGE ( 'NONE', *, *, #2366, .F. ) ;
#40583 = CARTESIAN_POINT ( 'NONE',  ( 776.9254006560222479, -332.1908817542433781, -314.8983024940802125 ) ) ;
#40585 = CARTESIAN_POINT ( 'NONE',  ( 763.0428371773158460, -419.4636090269702891, 358.7617431975195359 ) ) ;
#40584 = CARTESIAN_POINT ( 'NONE',  ( 785.3141322388236176, -93.72551174932934259, 364.4286716492789537 ) ) ;
#40588 = CARTESIAN_POINT ( 'NONE',  ( 752.4576283171824116, -333.0783235625956991, 317.7880784355627952 ) ) ;
#40587 = DIRECTION ( 'NONE',  ( -0.000000000000000000, -1.110223024625155554E-15, 1.000000000000000000 ) ) ;
#40586 = CARTESIAN_POINT ( 'NONE',  ( 808.0189434323515343, -446.0891481129646081, 319.0252816721025511 ) ) ;
#40589 = CARTESIAN_POINT ( 'NONE',  ( 758.0141637701419768, -111.0783235625964096, 367.2620300519063790 ) ) ;
#40590 = CARTESIAN_POINT ( 'NONE',  ( 759.0159684113467620, -328.9181544815160692, -325.8855110935213020 ) ) ;
#40591 = CARTESIAN_POINT ( 'NONE',  ( 774.6312213355099630, -335.3618753856920307, -364.6798772138717482 ) ) ;
#40592 = CARTESIAN_POINT ( 'NONE',  ( 801.9419747391806368, -162.4527844766018632, -351.9812246680014027 ) ) ;
#40593 = CARTESIAN_POINT ( 'NONE',  ( 755.2512626584698410, -439.5436935675101040, 315.2512626584710915 ) ) ;
#40595 = CARTESIAN_POINT ( 'NONE',  ( 939.9999999999993179, 50.81038600091411439, -193.6948738798775764 ) ) ;
#40594 = CYLINDRICAL_SURFACE ( 'NONE', #18969, 2.749999999999835687 ) ;
#40596 = CARTESIAN_POINT ( 'NONE',  ( 814.8207195650702488, -122.1908817542439749, -336.2433038121456548 ) ) ;
#40597 = CARTESIAN_POINT ( 'NONE',  ( -775.4999999999993179, -501.1515549466498669, -368.0974687824633520 ) ) ;
#40598 = DIRECTION ( 'NONE',  ( 0.000000000000000000, 0.000000000000000000, 1.000000000000000000 ) ) ;
#40599 = CARTESIAN_POINT ( 'NONE',  ( 784.1219089521767955, -285.2817908451526137, 315.0488828828318333 ) ) ;
#40600 = EDGE_LOOP ( 'NONE', ( #6770, #10506, #31376, #19888 ) ) ;
#40601 = CARTESIAN_POINT ( 'NONE',  ( 799.9636004259356241, -262.9181544815162965, 311.2241431872006956 ) ) ;
#40602 = CARTESIAN_POINT ( 'NONE',  ( 751.6929314249750860, -150.9982390220564241, -318.8095938919659034 ) ) ;
#40603 = DIRECTION ( 'NONE',  ( -1.000000000000000000, 0.000000000000000000, 0.000000000000000000 ) ) ;
#40604 = CARTESIAN_POINT ( 'NONE',  ( 771.3260364891663130, -91.64542720878951343, 306.0683387631859773 ) ) ;
#40605 = CARTESIAN_POINT ( 'NONE',  ( 759.0252816721024374, -264.9982390220561115, -368.0189434323527280 ) ) ;
#40606 = LINE ( 'NONE', #32379, #9232 ) ;
#40607 = CARTESIAN_POINT ( 'NONE',  ( 804.6798772138708955, -159.7255117493291436, 334.6312213355107019 ) ) ;
#40608 = ORIENTED_EDGE ( 'NONE', *, *, #1581, .F. ) ;
#40609 = CARTESIAN_POINT ( 'NONE',  ( 815.0009284576459549, -342.3510508353228943, -338.7629533639073429 ) ) ;
#40610 = CARTESIAN_POINT ( 'NONE',  ( 815.2698199232961542, -88.81642084023842187, -342.5225473063383106 ) ) ;
#40611 = CARTESIAN_POINT ( 'NONE',  ( 802.9823548866075953, -25.09997266333519050, 330.0799878456151077 ) ) ;
#40612 = CARTESIAN_POINT ( 'NONE',  ( 805.0032342141412300, -349.5436935675102745, -314.9967657858571783 ) ) ;
#40613 = CARTESIAN_POINT ( 'NONE',  ( 799.9999999999993179, 205.0000000000000568, 255.0000000000000000 ) ) ;
#40614 = CARTESIAN_POINT ( 'NONE',  ( 773.3843516231979720, -421.4419599262317888, 364.4086373105754433 ) ) ;
#40615 = ORIENTED_EDGE ( 'NONE', *, *, #30034, .F. ) ;
#40616 = CARTESIAN_POINT ( 'NONE',  ( 786.6156483768007774, -73.44195992623286884, 315.5913626894246136 ) ) ;
#40617 = CARTESIAN_POINT ( 'NONE',  ( 748.3538107759620743, -136.7146871989600072, -355.8262568251490165 ) ) ;
#40618 = DIRECTION ( 'NONE',  ( -0.000000000000000000, 0.000000000000000000, 1.000000000000000000 ) ) ;
#40619 = CARTESIAN_POINT ( 'NONE',  ( 751.2241431872005251, -256.1692326535049915, 359.9636004259367610 ) ) ;
#40620 = CARTESIAN_POINT ( 'NONE',  ( 759.7806653035535192, -78.99823902205665149, 324.8639956371181370 ) ) ;
#40621 = VERTEX_POINT ( 'NONE', #33711 ) ;
#40622 = EDGE_LOOP ( 'NONE', ( #35879, #40863, #16995, #10572 ) ) ;
#40623 = CARTESIAN_POINT ( 'NONE',  ( 765.0180583372156207, -240.9982390220561683, 360.0135310231089534 ) ) ;
#40624 = CARTESIAN_POINT ( 'NONE',  ( 803.8556311672234642, -417.6237781080499190, -365.6418435158340117 ) ) ;
#40625 = CARTESIAN_POINT ( 'NONE',  ( 911.9749999999993406, 154.9999999999998863, -360.0000000000000000 ) ) ;
#40626 = VERTEX_POINT ( 'NONE', #33476 ) ;
#40627 = ORIENTED_EDGE ( 'NONE', *, *, #29559, .T. ) ;
#40628 = CARTESIAN_POINT ( 'NONE',  ( 809.0717654672305343, -388.9181544815158986, -360.1688906516309885 ) ) ;
#40629 = CARTESIAN_POINT ( 'NONE',  ( 792.2312462859673587, -323.9073299311468190, 307.2067596250082602 ) ) ;
#40630 = CARTESIAN_POINT ( 'NONE',  ( 788.7631598425961101, -49.44195992623295410, 305.7194118038759143 ) ) ;
#40631 = CARTESIAN_POINT ( 'NONE',  ( 780.5236548040995785, -212.7363362996982232, -314.9735926884559944 ) ) ;
#40632 = CARTESIAN_POINT ( 'NONE',  ( 768.0187753319979720, -224.6346026584198228, -318.0580252608186242 ) ) ;
#40633 = CARTESIAN_POINT ( 'NONE',  ( 797.8594530101009923, -397.5436935675101040, -322.1405469898982119 ) ) ;
#40634 = ORIENTED_EDGE ( 'NONE', *, *, #22448, .F. ) ;
#40635 = CARTESIAN_POINT ( 'NONE',  ( 754.8072714833581358, -196.8164208402380950, 338.1981804954720587 ) ) ;
#40636 = CARTESIAN_POINT ( 'NONE',  ( 800.2193346964447755, -90.99823902205663728, -355.1360043628815788 ) ) ;
#40637 = ORIENTED_EDGE ( 'NONE', *, *, #22659, .F. ) ;
#40638 = CARTESIAN_POINT ( 'NONE',  ( 745.0891759886404770, -340.2709662947831362, 342.4968714119734159 ) ) ;
#40639 = DIRECTION ( 'NONE',  ( -1.000000000000000000, -0.000000000000000000, 0.000000000000000000 ) ) ;
#40640 = CARTESIAN_POINT ( 'NONE',  ( 794.9298647675502707, 16.45630643248849978, 314.4833286358118016 ) ) ;
#40641 = DIRECTION ( 'NONE',  ( 0.000000000000000000, 0.000000000000000000, 1.000000000000000000 ) ) ;
#40642 = CARTESIAN_POINT ( 'NONE',  ( 755.3028492785439312, -207.2817908451527842, 335.9200461376539693 ) ) ;
#40643 = CARTESIAN_POINT ( 'NONE',  ( 778.2165204200184689, -70.81642084023850714, 364.9363028652563230 ) ) ;
#40644 = ORIENTED_EDGE ( 'NONE', *, *, #4374, .T. ) ;
#40645 = CARTESIAN_POINT ( 'NONE',  ( 810.4231160770870019, -456.5545181178792404, -321.9338519418446936 ) ) ;
#40646 = CARTESIAN_POINT ( 'NONE',  ( 810.7187646348534145, -18.45278447660230725, -356.7737145352016341 ) ) ;
#40647 = CARTESIAN_POINT ( 'NONE',  ( 800.7704444035546203, -244.1692326535050768, 326.0291762391768771 ) ) ;
#40648 = CARTESIAN_POINT ( 'NONE',  ( 762.3223304703356007, -391.5436935675101608, -322.3223304703362828 ) ) ;
#40649 = CARTESIAN_POINT ( 'NONE',  ( 804.9363028652555840, -16.27096629478413092, -338.2165204200192079 ) ) ;
#40650 = CARTESIAN_POINT ( 'NONE',  ( 763.2262854647970016, -416.6346026584192259, 309.2812353651462445 ) ) ;
#40651 = CARTESIAN_POINT ( 'NONE',  ( 799.9999999999993179, -462.9681489794448339, -317.6393202250019954 ) ) ;
#40652 = CARTESIAN_POINT ( 'NONE',  ( 793.9708237608222134, -286.9181544815161828, -319.2295555964448681 ) ) ;
#40653 = CARTESIAN_POINT ( 'NONE',  ( 814.5518280994195948, -159.7255117493291436, -332.4837098697145734 ) ) ;
#40654 = CARTESIAN_POINT ( 'NONE',  ( 782.5225473063381969, -70.27096629478397460, 375.2698199232970637 ) ) ;
#40655 = CARTESIAN_POINT ( 'NONE',  ( 804.7487373415286811, -139.5436935675110135, 364.7487373415288516 ) ) ;
#40656 = CARTESIAN_POINT ( 'NONE',  ( 789.5497161195852414, 16.45630643248838609, -314.2297168413928148 ) ) ;
#40657 = LINE ( 'NONE', #33274, #28393 ) ;
#40658 = CARTESIAN_POINT ( 'NONE',  ( 911.9999999999993179, 154.9999999999998863, -350.0000000000000000 ) ) ;
#40659 = CARTESIAN_POINT ( 'NONE',  ( 759.0252816721024374, -360.9982390220557704, 368.0189434323527280 ) ) ;
#40660 = CARTESIAN_POINT ( 'NONE',  ( 758.0580252608178853, -342.4527844766013231, -328.0187753319985404 ) ) ;
#40661 = CARTESIAN_POINT ( 'NONE',  ( 804.1601925771018387, 16.55804007376685050, 346.5483106153029098 ) ) ;
#40662 = CARTESIAN_POINT ( 'NONE',  ( 744.6391490659812007, -86.73633629969862113, -338.7502325331110455 ) ) ;
#40663 = CARTESIAN_POINT ( 'NONE',  ( 770.0799878456142551, -133.9874144716872024, -362.9823548866085616 ) ) ;
#40664 = CARTESIAN_POINT ( 'NONE',  ( 744.8212110874229666, -138.8965053807781374, 336.2046728542121627 ) ) ;
#40665 = LINE ( 'NONE', #37189, #19555 ) ;
#40666 = CARTESIAN_POINT ( 'NONE',  ( 764.8639956371174549, -32.08914811296588709, -319.7806653035542013 ) ) ;
#40667 = CARTESIAN_POINT ( 'NONE',  ( 779.4709603349208464, -168.3510508353234911, -314.7162404726379918 ) ) ;
#40668 = CARTESIAN_POINT ( 'NONE',  ( 767.8955696845333705, -144.4527844766018632, 362.1676090361162323 ) ) ;
#40669 = CARTESIAN_POINT ( 'NONE',  ( 773.3843516231979720, -421.4419599262317888, -364.4086373105754433 ) ) ;
#40670 = EDGE_CURVE ( 'NONE', #24400, #14175, #27533, .T. ) ;
#40672 = CARTESIAN_POINT ( 'NONE',  ( 764.8639956371174549, -248.0891481129651766, 319.7806653035542581 ) ) ;
#40671 = CARTESIAN_POINT ( 'NONE',  ( 785.3141322388236176, -285.7255117493286889, 364.4286716492789537 ) ) ;
#40673 = CARTESIAN_POINT ( 'NONE',  ( -598.8365100919716042, 260.0000000000001705, -202.7499999999898250 ) ) ;
#40674 = ORIENTED_EDGE ( 'NONE', *, *, #45098, .T. ) ;
#40675 = CARTESIAN_POINT ( 'NONE',  ( 799.4546378042377910, 14.92167643740321381, 356.1575198192848006 ) ) ;
#40676 = CARTESIAN_POINT ( 'NONE',  ( 805.6418435158337843, -269.4636090269708006, -363.8556311672236916 ) ) ;
#40677 = ORIENTED_EDGE ( 'NONE', *, *, #44984, .F. ) ;
#40678 = APPLICATION_PROTOCOL_DEFINITION ( 'draft international standard', 'automotive_design', 1998, #127 ) ;
#40679 = CARTESIAN_POINT ( 'NONE',  ( 814.9108240113580450, -208.2709662947835341, 337.5031285880265273 ) ) ;
#40680 = CARTESIAN_POINT ( 'NONE',  ( 804.8461984189677878, -314.1908817542433781, 336.9566956441385628 ) ) ;
#40681 = CARTESIAN_POINT ( 'NONE',  ( 757.2208543904082489, -400.7146871989590977, 350.9844846989624330 ) ) ;
#40682 = ORIENTED_EDGE ( 'NONE', *, *, #17337, .T. ) ;
#40683 = CARTESIAN_POINT ( 'NONE',  ( 755.3028492785439312, -111.2817908451530968, -335.9200461376539693 ) ) ;
#40684 = CARTESIAN_POINT ( 'NONE',  ( 755.3201227861273992, -123.7255117493292147, -345.3687786644892981 ) ) ;
#40685 = CARTESIAN_POINT ( 'NONE',  ( 778.1981804954715471, -274.2709662947832499, -314.8072714833591021 ) ) ;
#40686 = ORIENTED_EDGE ( 'NONE', *, *, #16475, .F. ) ;
#40687 = CARTESIAN_POINT ( 'NONE',  ( 781.8018195045266339, -430.2709662947827383, -365.1927285166406705 ) ) ;
#40688 = CARTESIAN_POINT ( 'NONE',  ( 797.8594530101008786, -85.54369356751118403, -322.1405469898980982 ) ) ;
#40689 = CARTESIAN_POINT ( 'NONE',  ( 803.8651313633788504, -293.2601417444139429, 332.4468031744301015 ) ) ;
#40690 = CARTESIAN_POINT ( 'NONE',  ( 799.9999999999993179, 205.0000000000000568, 255.0000000000000000 ) ) ;
#40691 = LINE ( 'NONE', #44380, #20433 ) ;
#40692 = CARTESIAN_POINT ( 'NONE',  ( -468.8365100919714337, 230.0000000000001421, -199.9999999999908766 ) ) ;
#40693 = ORIENTED_EDGE ( 'NONE', *, *, #8906, .F. ) ;
#40694 = CARTESIAN_POINT ( 'NONE',  ( 771.3260364891663130, -355.6454272087887603, -306.0683387631859773 ) ) ;
#40695 = EDGE_CURVE ( 'NONE', #34711, #12298, #40196, .T. ) ;
#40696 = CARTESIAN_POINT ( 'NONE',  ( 812.3518521366052028, -217.0999726633345972, 326.5853460496235243 ) ) ;
#40698 = CARTESIAN_POINT ( 'NONE',  ( 788.7366044899766848, -275.9073299311469896, -316.5762568750059813 ) ) ;
#40697 = DIRECTION ( 'NONE',  ( 1.000000000000000000, 0.000000000000000000, 0.000000000000000000 ) ) ;
#40699 = CARTESIAN_POINT ( 'NONE',  ( 775.4999999999993179, -359.5698779088871788, -26.28906389436296109 ) ) ;
#40700 = CARTESIAN_POINT ( 'NONE',  ( 779.4763451958990572, -176.7363362996983369, -365.0264073115438919 ) ) ;
#40701 = ADVANCED_FACE ( 'NONE', ( #16153 ), #19616, .F. ) ;
#40702 = CARTESIAN_POINT ( 'NONE',  ( 808.3070685750230950, -42.99823902205675807, 361.1904061080339261 ) ) ;
#40703 = VECTOR ( 'NONE', #5143, 1000.000000000000000 ) ;
#40704 = LINE ( 'NONE', #15767, #28397 ) ;
#40705 = CARTESIAN_POINT ( 'NONE',  ( 746.8695393053151292, -389.9073299311465917, -327.6429770376306578 ) ) ;
#40706 = CARTESIAN_POINT ( 'NONE',  ( 521.6730038022808458, 229.9999999999999432, -122.7905160835442615 ) ) ;
#40707 = CARTESIAN_POINT ( 'NONE',  ( 771.2633955100217236, -47.90732993114767169, 363.4237431249939618 ) ) ;
#40708 = CARTESIAN_POINT ( 'NONE',  ( 813.5763878283155464, -315.8272453906070609, 351.1614460488615350 ) ) ;
#40709 = CARTESIAN_POINT ( 'NONE',  ( 808.0189434323515343, -254.0891481129652334, 319.0252816721025511 ) ) ;
#40710 = CARTESIAN_POINT ( 'NONE',  ( 801.1904061080336987, -20.08914811296592973, -368.3070685750235498 ) ) ;
#40711 = CARTESIAN_POINT ( 'NONE',  ( 781.8018195045266339, -262.2709662947831930, -365.1927285166406705 ) ) ;
#40712 = CARTESIAN_POINT ( 'NONE',  ( 441.1634899080286232, 229.9999999999999716, -197.2499999999973852 ) ) ;
#40713 = CARTESIAN_POINT ( 'NONE',  ( 797.8594530101008786, -373.5436935675101040, 322.1405469898980982 ) ) ;
#40714 = CARTESIAN_POINT ( 'NONE',  ( 784.1219089521767955, -117.2817908451530684, 315.0488828828318333 ) ) ;
#40715 = CARTESIAN_POINT ( 'NONE',  ( 789.9200121543843807, -1.987414471687640294, -317.0176451133914384 ) ) ;
#40716 = CARTESIAN_POINT ( 'NONE',  ( -208.8365100919714052, 260.0000000000001137, -199.9999999999926956 ) ) ;
#40717 = DIRECTION ( 'NONE',  ( -1.000000000000000000, 0.000000000000000000, 0.000000000000000000 ) ) ;
#40718 = CARTESIAN_POINT ( 'NONE',  ( 788.7366044899766848, -395.9073299311465348, 316.5762568750059813 ) ) ;
#40719 = ORIENTED_EDGE ( 'NONE', *, *, #22865, .T. ) ;
#40720 = CARTESIAN_POINT ( 'NONE',  ( 793.2243759319678702, -314.5328690171411949, -318.4439275373583200 ) ) ;
#40721 = EDGE_CURVE ( 'NONE', #32644, #28582, #7637, .T. ) ;
#40723 = CARTESIAN_POINT ( 'NONE',  ( 800.2193346964446619, -162.9982390220563673, 355.1360043628816925 ) ) ;
#40722 = CARTESIAN_POINT ( 'NONE',  ( 774.6858677611749044, -177.7255117493290868, 315.5713283507209894 ) ) ;
#40724 = CARTESIAN_POINT ( 'NONE',  ( 781.2497674668890113, -348.3510508353228943, -375.3608509340180603 ) ) ;
#40725 = CARTESIAN_POINT ( 'NONE',  ( 181.1634899080285948, 260.0000000000000000, -197.2499999999955662 ) ) ;
#40726 = EDGE_LOOP ( 'NONE', ( #21192, #17749, #45008, #33912 ) ) ;
#40727 = CARTESIAN_POINT ( 'NONE',  ( 756.5762568750052424, -363.1800572038739006, 348.7366044899774238 ) ) ;
#40728 = ORIENTED_EDGE ( 'NONE', *, *, #151, .T. ) ;
#40729 =( LENGTH_UNIT ( ) NAMED_UNIT ( * ) SI_UNIT ( .MILLI., .METRE. ) );
#40730 = CARTESIAN_POINT ( 'NONE',  ( 745.0891759886404770, -196.2709662947835909, -342.4968714119734159 ) ) ;
#40731 = CARTESIAN_POINT ( 'NONE',  ( 777.4774526936600978, -106.2709662947838467, 304.7301800767028226 ) ) ;
#40732 = ORIENTED_EDGE ( 'NONE', *, *, #33345, .T. ) ;
#40733 = AXIS2_PLACEMENT_3D ( 'NONE', #43756, #22748, #36843 ) ;
#40734 = CARTESIAN_POINT ( 'NONE',  ( 794.9819416627830151, -180.9982390220563389, -319.9864689768909898 ) ) ;
#40735 = ORIENTED_EDGE ( 'NONE', *, *, #31205, .T. ) ;
#40736 = CARTESIAN_POINT ( 'NONE',  ( 793.9708237608222134, -454.9181544815156713, -319.2295555964448681 ) ) ;
#40737 = CARTESIAN_POINT ( 'NONE',  ( 792.2312462859673587, -251.9073299311470748, 307.2067596250082602 ) ) ;
#40738 = CARTESIAN_POINT ( 'NONE',  ( 756.7813123517142913, -211.9874144716869750, 329.9779781133712504 ) ) ;
#40740 = FACE_OUTER_BOUND ( 'NONE', #19707, .T. ) ;
#40739 = PLANE ( 'NONE',  #14457 ) ;
#40741 = ADVANCED_FACE ( 'NONE', ( #8559 ), #8994, .F. ) ;
#40742 = ORIENTED_EDGE ( 'NONE', *, *, #2102, .T. ) ;
#40743 = CARTESIAN_POINT ( 'NONE',  ( 805.2837595273609850, -434.7363362996975980, -340.5290396650784714 ) ) ;
#40744 = DIRECTION ( 'NONE',  ( 1.000000000000000000, 0.000000000000000000, 0.000000000000000000 ) ) ;
#40745 = ORIENTED_EDGE ( 'NONE', *, *, #19126, .T. ) ;
#40746 = CARTESIAN_POINT ( 'NONE',  ( 778.7629533639073998, -224.7363362996982232, -375.0009284576466371 ) ) ;
#40747 = CARTESIAN_POINT ( 'NONE',  ( 809.0717654672305343, -100.9181544815167513, 360.1688906516309885 ) ) ;
#40749 = CARTESIAN_POINT ( 'NONE',  ( 781.8018195045266339, -190.2709662947835909, -365.1927285166406705 ) ) ;
#40748 = DIRECTION ( 'NONE',  ( 0.000000000000000000, 0.000000000000000000, 1.000000000000000000 ) ) ;
#40750 = CARTESIAN_POINT ( 'NONE',  ( 759.2295555964440155, -352.1692326535046504, -353.9708237608231229 ) ) ;
#40751 = DIRECTION ( 'NONE',  ( 0.000000000000000000, 0.000000000000000000, 1.000000000000000000 ) ) ;
#40752 = CARTESIAN_POINT ( 'NONE',  ( 799.9636004259356241, -238.9181544815163534, -311.2241431872006956 ) ) ;
#40753 = LINE ( 'NONE', #37054, #10472 ) ;
#40754 = CARTESIAN_POINT ( 'NONE',  ( 571.1634899080285095, 259.9999999999999432, -208.0249999999981014 ) ) ;
#40755 = CARTESIAN_POINT ( 'NONE',  ( 769.0155153010367712, -34.37269993606243901, -362.7791456095907279 ) ) ;
#40756 = EDGE_CURVE ( 'NONE', #34100, #30229, #39974, .T. ) ;
#40757 = CARTESIAN_POINT ( 'NONE',  ( 773.4516893846965786, -451.6454272087884192, 315.8398074228977066 ) ) ;
#40758 = AXIS2_PLACEMENT_3D ( 'NONE', #8737, #18454, #43809 ) ;
#40759 = CARTESIAN_POINT ( 'NONE',  ( 939.9999999999994316, -434.4637272565419153, -347.3621835540871530 ) ) ;
#40760 = CARTESIAN_POINT ( 'NONE',  ( 776.9566956441375396, -420.8965053807772279, -364.8461984189686405 ) ) ;
#40761 = CARTESIAN_POINT ( 'NONE',  ( 754.9967657858570647, -289.5436935675105019, -365.0032342141425943 ) ) ;
#40762 = CARTESIAN_POINT ( 'NONE',  ( 800.9840315886518738, -244.9181544815162681, 354.1144889064786412 ) ) ;
#40763 = DIRECTION ( 'NONE',  ( -0.000000000000000000, 1.000000000000000000, -0.000000000000000000 ) ) ;
#40764 = LINE ( 'NONE', #41000, #45283 ) ;
#40765 = CARTESIAN_POINT ( 'NONE',  ( 778.2165204200184689, -46.81642084023858530, -364.9363028652563230 ) ) ;
#40766 = CARTESIAN_POINT ( 'NONE',  ( 744.6391490659812007, -206.7363362996982801, 338.7502325331110455 ) ) ;
#40767 = CARTESIAN_POINT ( 'NONE',  ( 814.8230680027162407, -125.8055962898690581, -333.7305795820267917 ) ) ;
#40768 = CARTESIAN_POINT ( 'NONE',  ( 777.4774526936600978, -154.2709662947836478, 304.7301800767027657 ) ) ;
#40769 = CARTESIAN_POINT ( 'NONE',  ( 746.8695393053150156, -413.9073299311465348, -327.6429770376306010 ) ) ;
#40770 = LINE ( 'NONE', #29922, #15820 ) ;
#40771 = CARTESIAN_POINT ( 'NONE',  ( 792.1044303154645831, -252.4527844766015789, 317.8323909638837677 ) ) ;
#40772 = CARTESIAN_POINT ( 'NONE',  ( 769.0155153010367712, -10.37269993606250473, 362.7791456095907279 ) ) ;
#40773 = EDGE_CURVE ( 'NONE', #37557, #17589, #1604, .T. ) ;
#40774 = CARTESIAN_POINT ( 'NONE',  ( 805.1927285166397041, -400.8164208402373561, -341.8018195045277707 ) ) ;
#40775 = PLANE ( 'NONE',  #1822 ) ;
#40776 = CARTESIAN_POINT ( 'NONE',  ( 771.3260364891663130, -43.64542720878966975, -306.0683387631859773 ) ) ;
#40778 = EDGE_CURVE ( 'NONE', #34351, #26697, #31987, .T. ) ;
#40777 = CARTESIAN_POINT ( 'NONE',  ( -775.4999999999993179, -857.0166862835568509, -63.94525337997358605 ) ) ;
#40779 = CARTESIAN_POINT ( 'NONE',  ( 805.1016975059191054, -102.8965053807782368, 343.0745993439771837 ) ) ;
#40780 = ORIENTED_EDGE ( 'NONE', *, *, #44081, .T. ) ;
#40781 = CARTESIAN_POINT ( 'NONE',  ( 754.9735926884551418, -234.3510508353232638, -340.5236548041000333 ) ) ;
#40782 = ADVANCED_FACE ( 'NONE', ( #8113 ), #26083, .F. ) ;
#40783 = CARTESIAN_POINT ( 'NONE',  ( 781.7834795799800531, -58.81642084023854267, 315.0636971347436202 ) ) ;
#40784 = CARTESIAN_POINT ( 'NONE',  ( 745.1769319972822814, -209.8055962898687881, -346.2694204179732083 ) ) ;
#40785 = LINE ( 'NONE', #22776, #34160 ) ;
#40786 = CARTESIAN_POINT ( 'NONE',  ( 813.9316612368132837, -391.4419599262317888, 348.6739635108323228 ) ) ;
#40787 = ORIENTED_EDGE ( 'NONE', *, *, #22360, .T. ) ;
#40788 = CARTESIAN_POINT ( 'NONE',  ( 745.7998596910086917, -5.361875385693257279, 332.5602148656461168 ) ) ;
#40789 = CARTESIAN_POINT ( 'NONE',  ( 801.9419747391806368, -186.4527844766017779, -351.9812246680014027 ) ) ;
#40790 = CARTESIAN_POINT ( 'NONE',  ( 771.2633955100217236, -383.9073299311466485, 363.4237431249939618 ) ) ;
#40791 = CARTESIAN_POINT ( 'NONE',  ( 800.9747183278959710, -84.99823902205663728, -311.9810565676471583 ) ) ;
#40792 = AXIS2_PLACEMENT_3D ( 'NONE', #17243, #28789, #10778 ) ;
#40793 = CARTESIAN_POINT ( 'NONE',  ( 804.4286716492782716, -89.36187538569299704, -345.3141322388244703 ) ) ;
#40794 = ORIENTED_EDGE ( 'NONE', *, *, #26985, .T. ) ;
#40795 = CARTESIAN_POINT ( 'NONE',  ( 799.2566176426618085, -24.00906357242609346, -324.0069404352559559 ) ) ;
#40796 = ORIENTED_EDGE ( 'NONE', *, *, #17027, .T. ) ;
#40797 = CARTESIAN_POINT ( 'NONE',  ( 755.5913626894240451, -349.6454272087887603, -346.6156483768012890 ) ) ;
#40798 = EDGE_CURVE ( 'NONE', #6536, #6383, #22173, .T. ) ;
#40800 = CARTESIAN_POINT ( 'NONE',  ( 760.7433823573367135, -396.0090635724249637, 355.9930595647440441 ) ) ;
#40799 = CARTESIAN_POINT ( 'NONE',  ( 792.1044303154645831, -84.45278447660206211, 317.8323909638837677 ) ) ;
#40803 = CARTESIAN_POINT ( 'NONE',  ( 813.2346286133761168, -317.2601417444139429, 328.9521613784389160 ) ) ;
#40802 = CARTESIAN_POINT ( 'NONE',  ( 311.1634899080286232, 260.0000000000000000, -193.8809999999963338 ) ) ;
#40801 = CARTESIAN_POINT ( 'NONE',  ( 746.8695393053151292, -437.9073299311464211, 327.6429770376306578 ) ) ;
#40804 = EDGE_CURVE ( 'NONE', #16495, #34761, #43427, .T. ) ;
#40805 = CARTESIAN_POINT ( 'NONE',  ( 780.5236548040995785, -332.7363362996979390, -314.9735926884559944 ) ) ;
#40806 = CARTESIAN_POINT ( 'NONE',  ( 800.0135310231082713, -326.0891481129649492, -325.0180583372163028 ) ) ;
#40807 = CARTESIAN_POINT ( 'NONE',  ( 814.2805881961230625, -145.6454272087893287, -331.2368401574024119 ) ) ;
#40808 = CARTESIAN_POINT ( 'NONE',  ( 768.9521613784389729, -9.827245390607961539, 373.2346286133773106 ) ) ;
#40809=STYLED_ITEM('',(#45765),#33039);
#40811 = DIRECTION ( 'NONE',  ( 0.000000000000000000, 1.000000000000000000, -0.000000000000000000 ) ) ;
#40810 = FACE_OUTER_BOUND ( 'NONE', #20382, .T. ) ;
#40812 = CARTESIAN_POINT ( 'NONE',  ( 776.9566956441375396, -252.8965053807777394, -364.8461984189686405 ) ) ;
#40813 = CARTESIAN_POINT ( 'NONE',  ( 802.2119215644370342, -126.0090635724257737, -367.5423716828165084 ) ) ;
#40814 = DIRECTION ( 'NONE',  ( 0.000000000000000000, 0.000000000000000000, -1.000000000000000000 ) ) ;
#40816 = EDGE_CURVE ( 'NONE', #6488, #1032, #32807, .T. ) ;
#40815 = LINE ( 'NONE', #5468, #40018 ) ;
#40817 = ADVANCED_FACE ( 'NONE', ( #8322 ), #36724, .F. ) ;
#40818 = CARTESIAN_POINT ( 'NONE',  ( 757.4527132478984868, -328.3726999360615650, 329.1273215169538844 ) ) ;
#40819 = CARTESIAN_POINT ( 'NONE',  ( 788.7366044899766848, -179.9073299311472454, 316.5762568750059813 ) ) ;
#40820 = VERTEX_POINT ( 'NONE', #8781 ) ;
#40821 = CARTESIAN_POINT ( 'NONE',  ( 764.1737431748507561, -298.3726999360616787, 371.6461892240376415 ) ) ;
#40822 = CARTESIAN_POINT ( 'NONE',  ( 744.7301800767020268, -148.8164208402382656, -337.4774526936615189 ) ) ;
#40823 = DIRECTION ( 'NONE',  ( -1.880165489482579047E-16, -1.000000000000000000, -0.000000000000000000 ) ) ;
#40824 = CARTESIAN_POINT ( 'NONE',  ( 788.6739635108323228, -79.64542720878957027, 373.9316612368139090 ) ) ;
#40825 = CARTESIAN_POINT ( 'NONE',  ( 813.1304606946830518, -281.9073299311468759, -352.3570229623690580 ) ) ;
#40826 = CARTESIAN_POINT ( 'NONE',  ( 808.3070685750232087, -450.9982390220554294, -361.1904061080339829 ) ) ;
#40827 = CARTESIAN_POINT ( 'NONE',  ( 800.0135310231082713, -158.0891481129655176, 325.0180583372163028 ) ) ;
#40828 = VECTOR ( 'NONE', #654, 1000.000000000000000 ) ;
#40829 = VERTEX_POINT ( 'NONE', #33258 ) ;
#40830 = CARTESIAN_POINT ( 'NONE',  ( 756.1443688327750579, -357.6237781080501463, -314.3581564841659315 ) ) ;
#40831 = CIRCLE ( 'NONE', #34925, 2.749999999999919176 ) ;
#40832 = CARTESIAN_POINT ( 'NONE',  ( 801.1904061080336987, -92.08914811296568814, -368.3070685750235498 ) ) ;
#40833 = CARTESIAN_POINT ( 'NONE',  ( 759.0159684113467620, -40.91815448151695023, 325.8855110935213020 ) ) ;
#40834 = CARTESIAN_POINT ( 'NONE',  ( 763.2262854647970016, -344.6346026584195101, -309.2812353651462445 ) ) ;
#40835 = DIRECTION ( 'NONE',  ( 0.000000000000000000, 0.000000000000000000, -1.000000000000000000 ) ) ;
#40836 = CARTESIAN_POINT ( 'NONE',  ( 754.9735926884551418, -426.3510508353226669, 340.5236548041000333 ) ) ;
#40837 = ORIENTED_EDGE ( 'NONE', *, *, #33769, .F. ) ;
#40838 = CARTESIAN_POINT ( 'NONE',  ( 783.7566961878529810, -120.8965053807781800, -305.1792804349288417 ) ) ;
#40839 = DIRECTION ( 'NONE',  ( -0.000000000000000000, 1.000000000000000000, -0.000000000000000000 ) ) ;
#40840 = CARTESIAN_POINT ( 'NONE',  ( 781.2497674668890113, -276.3510508353231785, 375.3608509340180603 ) ) ;
#40841 = CARTESIAN_POINT ( 'NONE',  ( 774.6312213355098493, -71.36187538569303968, 364.6798772138717482 ) ) ;
#40842 = ORIENTED_EDGE ( 'NONE', *, *, #29773, .F. ) ;
#40843 = VECTOR ( 'NONE', #2870, 1000.000000000000000 ) ;
#40844 = CARTESIAN_POINT ( 'NONE',  ( 788.8264449731200330, -285.1800572038740711, 363.6646147819171233 ) ) ;
#40845 = CARTESIAN_POINT ( 'NONE',  ( 811.6461892240364477, -436.7146871989589272, -324.1737431748509835 ) ) ;
#40846 = DIRECTION ( 'NONE',  ( 1.000000000000000000, 0.000000000000000000, 0.000000000000000000 ) ) ;
#40847 = EDGE_LOOP ( 'NONE', ( #39120, #10978, #27010, #40366 ) ) ;
#40848 = VERTEX_POINT ( 'NONE', #12016 ) ;
#40849 = CARTESIAN_POINT ( 'NONE',  ( 814.2805881961230625, -385.6454272087888171, -331.2368401574024119 ) ) ;
#40850 = EDGE_CURVE ( 'NONE', #30459, #9099, #13540, .T. ) ;
#40851 = CARTESIAN_POINT ( 'NONE',  ( 794.9819416627830151, -300.9982390220559409, 319.9864689768909898 ) ) ;
#40853 = CARTESIAN_POINT ( 'NONE',  ( 786.2056067578752163, -203.8055962898688449, 374.4686193811670023 ) ) ;
#40852 = CARTESIAN_POINT ( 'NONE',  ( 763.2262854647970016, -320.6346026584195670, 309.2812353651462445 ) ) ;
#40854 = CARTESIAN_POINT ( 'NONE',  ( 810.1134526219336749, -32.53286901714208312, 357.8822607201570349 ) ) ;
#40855 = CARTESIAN_POINT ( 'NONE',  ( 766.9102291470427417, -210.5545181178800647, -318.6633372737382501 ) ) ;
#40856 = CARTESIAN_POINT ( 'NONE',  ( 804.4286716492782716, -233.3618753856925423, -345.3141322388244703 ) ) ;
#40857 = CIRCLE ( 'NONE', #4728, 10.00000000000000888 ) ;
#40858 = CARTESIAN_POINT ( 'NONE',  ( 800.2193346964446619, -426.9982390220555430, -355.1360043628816925 ) ) ;
#40859 = AXIS2_PLACEMENT_3D ( 'NONE', #784, #39604, #43711 ) ;
#40860 = EDGE_LOOP ( 'NONE', ( #37607, #21538, #27220, #5732 ) ) ;
#40861 = CARTESIAN_POINT ( 'NONE',  ( 801.9419747391806368, -210.4527844766016926, 351.9812246680014027 ) ) ;
#40862 = CARTESIAN_POINT ( 'NONE',  ( 805.1927285166397041, -112.8164208402383508, -341.8018195045277707 ) ) ;
#40863 = ORIENTED_EDGE ( 'NONE', *, *, #25594, .F. ) ;
#40864 = CARTESIAN_POINT ( 'NONE',  ( 805.0032342141412300, -373.5436935675101040, 314.9967657858571783 ) ) ;
#40865 = PLANE ( 'NONE',  #41050 ) ;
#40866 = PLANE ( 'NONE',  #1274 ) ;
#40867 = DIRECTION ( 'NONE',  ( -0.000000000000000000, 1.000000000000000000, -0.000000000000000000 ) ) ;
#40868 = CARTESIAN_POINT ( 'NONE',  ( 780.5236548040995785, -188.7363362996983085, 314.9735926884559944 ) ) ;
#40869 = CARTESIAN_POINT ( 'NONE',  ( 781.8018195045266339, -70.27096629478397460, 365.1927285166406705 ) ) ;
#40870 = ORIENTED_EDGE ( 'NONE', *, *, #40510, .F. ) ;
#40871 = CARTESIAN_POINT ( 'NONE',  ( 799.9636004259356241, -430.9181544815157849, -311.2241431872006956 ) ) ;
#40872 = CARTESIAN_POINT ( 'NONE',  ( 796.7737145352015204, -44.63460265842040542, -370.7187646348536987 ) ) ;
#40873 = CARTESIAN_POINT ( 'NONE',  ( 803.2186876482843445, -271.9874144716868045, 350.0220218866286928 ) ) ;
#40874 = CARTESIAN_POINT ( 'NONE',  ( 788.8264449731200330, -405.1800572038737300, -363.6646147819171233 ) ) ;
#40875 = CARTESIAN_POINT ( 'NONE',  ( 759.9864689768902508, -26.08914811296592262, -354.9819416627836404 ) ) ;
#40876 = VECTOR ( 'NONE', #19156, 1000.000000000000000 ) ;
#40877 = CARTESIAN_POINT ( 'NONE',  ( 808.0189434323515343, -446.0891481129646081, 319.0252816721025511 ) ) ;
#40878 = CARTESIAN_POINT ( 'NONE',  ( 791.7608162188021197, 205.0000000000000568, -360.0000000000000000 ) ) ;
#40879 = CARTESIAN_POINT ( 'NONE',  ( 805.2837595273609850, -290.7363362996980527, -340.5290396650784714 ) ) ;
#40880 = CARTESIAN_POINT ( 'NONE',  ( 767.6429770376289525, -153.1800572038746395, -306.8695393053162093 ) ) ;
#40881 = CARTESIAN_POINT ( 'NONE',  ( 792.3570229623688874, -93.18005720387481006, 373.1304606946836202 ) ) ;
#40882 = CARTESIAN_POINT ( 'NONE',  ( 787.5162901302840055, -155.3618753856927128, 305.4481719005792684 ) ) ;
#40883 = CARTESIAN_POINT ( 'NONE',  ( 792.8389451398237497, 16.45630643248849978, -314.6345231965543121 ) ) ;
#40884 = LINE ( 'NONE', #37422, #22482 ) ;
#40885 = CARTESIAN_POINT ( 'NONE',  ( 786.2056067578752163, -227.8055962898687596, -374.4686193811670023 ) ) ;
#40886 = DIRECTION ( 'NONE',  ( 1.000000000000000000, 0.000000000000000000, 0.000000000000000000 ) ) ;
#40887 = CARTESIAN_POINT ( 'NONE',  ( 772.5602148656447525, -393.7255117493283478, 305.7998596910095443 ) ) ;
#40888 = CARTESIAN_POINT ( 'NONE',  ( 745.4481719005789273, -27.72551174932954510, 347.5162901302853697 ) ) ;
#40889 = CARTESIAN_POINT ( 'NONE',  ( 762.3223304703356007, -367.5436935675102745, -322.3223304703362828 ) ) ;
#40890 = CARTESIAN_POINT ( 'NONE',  ( 758.6633372737375112, 3.467130982857797417, 326.9102291470432533 ) ) ;
#40891 = CARTESIAN_POINT ( 'NONE',  ( 776.2046728542105711, -116.1908817542440033, -304.8212110874238761 ) ) ;
#40892 = CARTESIAN_POINT ( 'NONE',  ( 765.8855110935204493, -142.1692326535054178, -319.0159684113471599 ) ) ;
#40893 = CARTESIAN_POINT ( 'NONE',  ( 807.5423716828161105, -153.0783235625962675, 362.2119215644372048 ) ) ;
#40894 = FACE_OUTER_BOUND ( 'NONE', #31579, .T. ) ;
#40895 = CARTESIAN_POINT ( 'NONE',  ( 785.3141322388236176, -69.72551174932942786, -364.4286716492789537 ) ) ;
#40896 = CARTESIAN_POINT ( 'NONE',  ( 784.0799538623451781, -155.8055962898689586, -364.6971507214555572 ) ) ;
#40897 = CARTESIAN_POINT ( 'NONE',  ( 797.6776695296629214, -115.5436935675110988, -357.6776695296636603 ) ) ;
#40898 = CARTESIAN_POINT ( 'NONE',  ( 755.3201227861273992, -171.7255117493291152, 345.3687786644892981 ) ) ;
#40899 = CARTESIAN_POINT ( 'NONE',  ( 803.8556311672234642, -9.623778108051251223, -365.6418435158340117 ) ) ;
#40900 = CARTESIAN_POINT ( 'NONE',  ( 795.1360043628808398, -308.0891481129650629, 360.2193346964456282 ) ) ;
#40901 = CARTESIAN_POINT ( 'NONE',  ( 789.9999999999992042, 205.0000000000000568, -339.9999999999999432 ) ) ;
#40902 = ORIENTED_EDGE ( 'NONE', *, *, #35641, .F. ) ;
#40903 = CARTESIAN_POINT ( 'NONE',  ( 796.7845633553578182, -33.62377810805116951, 358.5707757039688204 ) ) ;
#40904 = CARTESIAN_POINT ( 'NONE',  ( 814.2805881961230625, -265.6454272087889876, -331.2368401574024119 ) ) ;
#40905 = AXIS2_PLACEMENT_3D ( 'NONE', #45454, #34357, #6641 ) ;
#40906 = EDGE_LOOP ( 'NONE', ( #6861, #42849 ) ) ;
#40907 = PRODUCT_CONTEXT ( 'NONE', #10433, 'mechanical' ) ;
#40908 = CIRCLE ( 'NONE', #2526, 19.99999999999990763 ) ;
#40909 = CARTESIAN_POINT ( 'NONE',  ( 804.7487373415286811, -211.5436935675107861, 364.7487373415288516 ) ) ;
#40910 = CARTESIAN_POINT ( 'NONE',  ( 804.1105419155481968, -291.8272453906071746, 347.6308680596136469 ) ) ;
#40911 = CARTESIAN_POINT ( 'NONE',  ( 800.7704444035546203, -412.1692326535045936, 326.0291762391768771 ) ) ;
#40912 = EDGE_LOOP ( 'NONE', ( #40353, #39913 ) ) ;
#40913 = CARTESIAN_POINT ( 'NONE',  ( 783.0745993439762742, -128.1908817542439465, -365.1016975059196739 ) ) ;
#40914 = CARTESIAN_POINT ( 'NONE',  ( 781.7834795799800531, -106.8164208402383935, -315.0636971347436202 ) ) ;
#40916 = ADVANCED_FACE ( 'NONE', ( #19389 ), #22849, .T. ) ;
#40915 = CARTESIAN_POINT ( 'NONE',  ( 778.1981804954715471, -322.2709662947830793, -314.8072714833591021 ) ) ;
#40917 = ORIENTED_EDGE ( 'NONE', *, *, #41837, .T. ) ;
#40918 = CARTESIAN_POINT ( 'NONE',  ( 803.4237431249931660, -423.1800572038737300, -331.2633955100225194 ) ) ;
#40919 = CARTESIAN_POINT ( 'NONE',  ( 765.8855110935204493, -286.1692326535048778, 319.0159684113471599 ) ) ;
#40920 = CARTESIAN_POINT ( 'NONE',  ( 792.5472707286114655, -457.8762024727506628, 368.6839859091244307 ) ) ;
#40921 = DIRECTION ( 'NONE',  ( 1.000000000000000000, 0.000000000000000000, -0.000000000000000000 ) ) ;
#40922 = CARTESIAN_POINT ( 'NONE',  ( 311.1634899080286232, 260.0000000000000000, -191.9749999999963279 ) ) ;
#40923 = ORIENTED_EDGE ( 'NONE', *, *, #19257, .F. ) ;
#40924 = CARTESIAN_POINT ( 'NONE',  ( 804.1009440267234822, -359.4636090269705164, -314.0944755984392600 ) ) ;
#40925 = AXIS2_PLACEMENT_3D ( 'NONE', #34640, #28157, #2997 ) ;
#40926 = CARTESIAN_POINT ( 'NONE',  ( 773.7305795820266212, -201.2817908451528126, 374.8230680027170365 ) ) ;
#40927 = VECTOR ( 'NONE', #31396, 1000.000000000000000 ) ;
#40928 = CARTESIAN_POINT ( 'NONE',  ( 805.1927285166397041, -304.8164208402376403, -341.8018195045277707 ) ) ;
#40929 = DIRECTION ( 'NONE',  ( 0.000000000000000000, 0.000000000000000000, 1.000000000000000000 ) ) ;
#40930 = CARTESIAN_POINT ( 'NONE',  ( 804.8461984189677878, -194.1908817542437475, -336.9566956441385628 ) ) ;
#40931 = CARTESIAN_POINT ( 'NONE',  ( 747.2067596250078623, -51.18005720387493085, 352.2312462859687230 ) ) ;
#40932 = CARTESIAN_POINT ( 'NONE',  ( -338.8365100919713200, 256.5000000000001137, -199.9999999999917861 ) ) ;
#40933 = CARTESIAN_POINT ( 'NONE',  ( 772.5602148656447525, -393.7255117493283478, -305.7998596910095443 ) ) ;
#40934 = DIRECTION ( 'NONE',  ( -0.000000000000000000, 1.000000000000000000, -0.000000000000000000 ) ) ;
#40935 = CARTESIAN_POINT ( 'NONE',  ( 797.8594530101008786, -61.54369356751124087, 322.1405469898980982 ) ) ;
#40936 = CIRCLE ( 'NONE', #11442, 10.00000000000000888 ) ;
#40937 = CARTESIAN_POINT ( 'NONE',  ( 748.6759233522253680, -328.3726999360615650, 324.3348316497537098 ) ) ;
#40938 = CARTESIAN_POINT ( 'NONE',  ( 800.9747183278959710, -276.9982390220559978, 311.9810565676471583 ) ) ;
#40939 = CARTESIAN_POINT ( 'NONE',  ( 777.4774526936600978, -34.27096629478407408, -304.7301800767027657 ) ) ;
#40940 = CARTESIAN_POINT ( 'NONE',  ( 785.3141322388236176, -261.7255117493288026, -364.4286716492789537 ) ) ;
#40941 = VECTOR ( 'NONE', #27153, 1000.000000000000000 ) ;
#40942 = DIRECTION ( 'NONE',  ( -0.000000000000000000, 1.000000000000000000, -0.000000000000000000 ) ) ;
#40943 = AXIS2_PLACEMENT_3D ( 'NONE', #36623, #11904, #11460 ) ;
#40944 = CARTESIAN_POINT ( 'NONE',  ( 800.0135310231082713, -374.0891481129647786, 325.0180583372163028 ) ) ;
#40945 = CARTESIAN_POINT ( 'NONE',  ( 786.5483106153019435, -103.6454272087894850, 364.1601925771022366 ) ) ;
#40946 = CARTESIAN_POINT ( 'NONE',  ( 763.2154366446407039, -45.62377810805114109, -321.4292242960311228 ) ) ;
#40947 = CARTESIAN_POINT ( 'NONE',  ( 795.6651683502461765, -34.71468719896025590, 371.3240766477733814 ) ) ;
#40948 = CARTESIAN_POINT ( 'NONE',  ( 778.1981804954715471, -370.2709662947830793, 314.8072714833591021 ) ) ;
#40949 = CARTESIAN_POINT ( 'NONE',  ( -786.4999999999993179, -110.5936016518798652, 750.6326042729449455 ) ) ;
#40950 = CARTESIAN_POINT ( 'NONE',  ( 879.9999999999992042, 239.9999999999998010, 360.0000000000000000 ) ) ;
#40951 = CARTESIAN_POINT ( 'NONE',  ( 793.4146539503750546, -145.9874144716871740, 307.6481478633938877 ) ) ;
#40952 = CARTESIAN_POINT ( 'NONE',  ( 785.3141322388236176, -381.7255117493284615, 364.4286716492789537 ) ) ;
#40953 = ORIENTED_EDGE ( 'NONE', *, *, #11738, .F. ) ;
#40954 = AXIS2_PLACEMENT_3D ( 'NONE', #27764, #34694, #10210 ) ;
#40955 = CARTESIAN_POINT ( 'NONE',  ( 803.8651313633788504, -341.2601417444138292, -332.4468031744301015 ) ) ;
#40957 = CARTESIAN_POINT ( 'NONE',  ( 756.5762568750052424, -195.1800572038744974, 348.7366044899774238 ) ) ;
#40956 = CARTESIAN_POINT ( 'NONE',  ( 762.3223304703356007, -199.5436935675108430, 322.3223304703362828 ) ) ;
#40958 = CARTESIAN_POINT ( 'NONE',  ( 764.3348316497523456, -358.7146871989592114, -308.6759233522265617 ) ) ;
#40959 = LINE ( 'NONE', #1470, #37410 ) ;
#40960 = VERTEX_POINT ( 'NONE', #23743 ) ;
#40961 = CARTESIAN_POINT ( 'NONE',  ( 800.0135310231082713, -374.0891481129647786, 325.0180583372163028 ) ) ;
#40962 = AXIS2_PLACEMENT_3D ( 'NONE', #7075, #10300, #17705 ) ;
#40963 = VERTEX_POINT ( 'NONE', #16853 ) ;
#40964 = DIRECTION ( 'NONE',  ( 1.000000000000000000, 0.000000000000000000, 0.000000000000000000 ) ) ;
#40965 = CARTESIAN_POINT ( 'NONE',  ( 810.7187646348534145, -234.4527844766016358, -356.7737145352016341 ) ) ;
#40966 = CARTESIAN_POINT ( 'NONE',  ( 782.4968714119720516, -130.8164208402383224, 305.0891759886411023 ) ) ;
#40967 = ORIENTED_EDGE ( 'NONE', *, *, #32345, .F. ) ;
#40968 = CARTESIAN_POINT ( 'NONE',  ( 803.4237431249931660, -183.1800572038744974, -331.2633955100225194 ) ) ;
#40969 = VERTEX_POINT ( 'NONE', #20066 ) ;
#40970 = CARTESIAN_POINT ( 'NONE',  ( 754.8072714833581358, -316.8164208402377540, -338.1981804954720587 ) ) ;
#40971 = CARTESIAN_POINT ( 'NONE',  ( 784.1219089521767955, -453.2817908451519315, -315.0488828828318333 ) ) ;
#40972 = AXIS2_PLACEMENT_3D ( 'NONE', #21359, #35435, #32448 ) ;
#40973 = CARTESIAN_POINT ( 'NONE',  ( 759.0252816721024374, -240.9982390220561683, 368.0189434323527280 ) ) ;
#40974 = CARTESIAN_POINT ( 'NONE',  ( 789.9200121543843807, -193.9874144716870319, 317.0176451133914384 ) ) ;
#40976 = CARTESIAN_POINT ( 'NONE',  ( 759.9999999999992042, 205.0000000000000568, -339.9999999999999432 ) ) ;
#40975 = DIRECTION ( 'NONE',  ( 0.9164815115825537539, 0.1263042864341373805, -0.3796167358741193709 ) ) ;
#40977 = DIRECTION ( 'NONE',  ( 0.000000000000000000, -0.9238795325112892920, 0.3826834323650836756 ) ) ;
#40978 = CIRCLE ( 'NONE', #3373, 8.025000000000003908 ) ;
#40979 = PRODUCT_DEFINITION_SHAPE ( 'NONE', 'NONE',  #45726 ) ;
#40980 = ORIENTED_EDGE ( 'NONE', *, *, #26084, .F. ) ;
#40981 = CARTESIAN_POINT ( 'NONE',  ( 800.9840315886518738, -412.9181544815157281, -354.1144889064786412 ) ) ;
#40982 = DIRECTION ( 'NONE',  ( -0.000000000000000000, -0.000000000000000000, 1.000000000000000000 ) ) ;
#40983 = LINE ( 'NONE', #27125, #7119 ) ;
#40984 = VERTEX_POINT ( 'NONE', #37623 ) ;
#40985 = CARTESIAN_POINT ( 'NONE',  ( 762.1177392798416577, -234.5545181178799794, -309.8865473780659272 ) ) ;
#40986 = CARTESIAN_POINT ( 'NONE',  ( 745.5313806188320314, -87.28179084515316788, 333.7943932421247268 ) ) ;
#40988 = CARTESIAN_POINT ( 'NONE',  ( 757.8323909638827445, -194.6346026584198796, -352.1044303154654358 ) ) ;
#40987 = FACE_OUTER_BOUND ( 'NONE', #4961, .T. ) ;
#40989 = CARTESIAN_POINT ( 'NONE',  ( 770.0799878456142551, -373.9874144716864066, -362.9823548866085616 ) ) ;
#40990 = CARTESIAN_POINT ( 'NONE',  ( 750.9282345327678740, -208.9181544815164102, -319.8311093483690115 ) ) ;
#40991 = DIRECTION ( 'NONE',  ( -0.000000000000000000, 1.000000000000000000, -0.000000000000000000 ) ) ;
#40992 = FACE_OUTER_BOUND ( 'NONE', #34538, .T. ) ;
#40993 = CARTESIAN_POINT ( 'NONE',  ( 804.6971507214547046, -75.28179084515321051, -344.0799538623459739 ) ) ;
#40994 = CARTESIAN_POINT ( 'NONE',  ( 763.0428371773158460, -419.4636090269702891, 358.7617431975195359 ) ) ;
#40995 = EDGE_CURVE ( 'NONE', #15857, #3171, #12682, .T. ) ;
#40996 = DIRECTION ( 'NONE',  ( -0.000000000000000000, 1.000000000000000000, -0.000000000000000000 ) ) ;
#40997 = VECTOR ( 'NONE', #21330, 1000.000000000000000 ) ;
#40998 = CARTESIAN_POINT ( 'NONE',  ( 747.2067596250078623, -267.1800572038742985, -352.2312462859687230 ) ) ;
#40999 = DIRECTION ( 'NONE',  ( 1.000000000000000000, 0.000000000000000000, 0.000000000000000000 ) ) ;
#41000 = CARTESIAN_POINT ( 'NONE',  ( -26.63011601220122060, -513.1383975375929367, -369.9999999999999432 ) ) ;
#41001 = CARTESIAN_POINT ( 'NONE',  ( 771.1735550268778070, -57.18005720387489532, -316.3353852180827630 ) ) ;
#41002 = CIRCLE ( 'NONE', #31431, 20.00000000000001776 ) ;
#41003 = CARTESIAN_POINT ( 'NONE',  ( 745.7194118038753459, -205.6454272087891297, 348.7631598425976449 ) ) ;
#41004 = CARTESIAN_POINT ( 'NONE',  ( 800.1688906516307043, -154.1692326535053894, -369.0717654672308186 ) ) ;
#41005 = CARTESIAN_POINT ( 'NONE',  ( 792.2312462859673587, -155.9073299311473306, 307.2067596250082602 ) ) ;
#41006 = CARTESIAN_POINT ( 'NONE',  ( 787.4397851343537695, -405.7255117493283478, -374.2001403089903988 ) ) ;
#41007 = DIRECTION ( 'NONE',  ( 0.000000000000000000, 0.000000000000000000, 1.000000000000000000 ) ) ;
#41008 = CARTESIAN_POINT ( 'NONE',  ( 762.1405469898971887, -265.5436935675106156, 357.8594530101015607 ) ) ;
#41009 = CARTESIAN_POINT ( 'NONE',  ( 804.8461984189677878, -50.19088175424420939, 336.9566956441385628 ) ) ;
#41010 = CARTESIAN_POINT ( 'NONE',  ( 754.8072714833581358, -436.8164208402372992, -338.1981804954720587 ) ) ;
#41011 = AXIS2_PLACEMENT_3D ( 'NONE', #15350, #30098, #43503 ) ;
#41012 = CARTESIAN_POINT ( 'NONE',  ( 790.0183182880230106, -452.9681489794449476, 362.9048749981275250 ) ) ;
#41013 = CARTESIAN_POINT ( 'NONE',  ( 919.9999999999993179, 154.9999999999998863, 350.0000000000000000 ) ) ;
#41014 = CARTESIAN_POINT ( 'NONE',  ( 783.0433043558608688, -96.89650538077825104, 315.1538015810313027 ) ) ;
#41015 = VERTEX_POINT ( 'NONE', #17292 ) ;
#41016 = CIRCLE ( 'NONE', #36566, 2.749999999999842792 ) ;
#41017 = EDGE_CURVE ( 'NONE', #8247, #16583, #15023, .T. ) ;
#41018 = CARTESIAN_POINT ( 'NONE',  ( 759.2295555964440155, -208.1692326535051905, -353.9708237608231229 ) ) ;
#41019 = CARTESIAN_POINT ( 'NONE',  ( 778.1981804954714335, -58.27096629478398171, 314.8072714833589885 ) ) ;
#41020 = CARTESIAN_POINT ( 'NONE',  ( 747.3154664389472828, -259.9874144716869182, -326.4474001241230781 ) ) ;
#41021 = DIRECTION ( 'NONE',  ( 0.000000000000000000, 1.110223024625155554E-15, 1.000000000000000000 ) ) ;
#41022 = CARTESIAN_POINT ( 'NONE',  ( 746.0683387631852383, -379.4419599262318457, 331.3260364891676204 ) ) ;
#41023 = ORIENTED_EDGE ( 'NONE', *, *, #17520, .T. ) ;
#41024 = CARTESIAN_POINT ( 'NONE',  ( 764.8639956371174549, -176.0891481129653755, -319.7806653035542013 ) ) ;
#41025 = CARTESIAN_POINT ( 'NONE',  ( 785.3687786644884454, -371.3618753856919739, 315.3201227861279676 ) ) ;
#41026 = EDGE_CURVE ( 'NONE', #40960, #7806, #37855, .T. ) ;
#41027 = CARTESIAN_POINT ( 'NONE',  ( 811.0346526505616112, -110.6346026584201638, -323.0537975583477532 ) ) ;
#41028 = CARTESIAN_POINT ( 'NONE',  ( 774.6858677611749044, -57.72551174932945628, -315.5713283507209894 ) ) ;
#41029 = ORIENTED_EDGE ( 'NONE', *, *, #36014, .T. ) ;
#41030 = CARTESIAN_POINT ( 'NONE',  ( 779.4763451958990572, -56.73633629969872771, -365.0264073115438919 ) ) ;
#41031 = CARTESIAN_POINT ( 'NONE',  ( 757.0176451133909268, -349.0999726633342561, -349.9200121543848354 ) ) ;
#41033 = CARTESIAN_POINT ( 'NONE',  ( 798.5707757039680246, -413.4636090269704027, 356.7845633553585003 ) ) ;
#41032 = CARTESIAN_POINT ( 'NONE',  ( 755.5713283507202505, -101.3618753856929544, 334.6858677611754729 ) ) ;
#41034 = CARTESIAN_POINT ( 'NONE',  ( 763.2154366446407039, -93.62377810805098477, 321.4292242960311228 ) ) ;
#41037 = CARTESIAN_POINT ( 'NONE',  ( 768.8385539511368734, -359.2601417444137724, 306.4236121716840557 ) ) ;
#41036 = CARTESIAN_POINT ( 'NONE',  ( 772.4999999999993179, -462.9681489794447202, 270.0000000000000568 ) ) ;
#41035 = CARTESIAN_POINT ( 'NONE',  ( 796.9462024416508257, -444.4527844766009821, 308.9653473494370246 ) ) ;
#41038 = CARTESIAN_POINT ( 'NONE',  ( 769.9779781133707957, -307.0999726633343130, -316.7813123517150871 ) ) ;
#41039 = CARTESIAN_POINT ( 'NONE',  ( 755.5713283507202505, -317.3618753856922581, -334.6858677611754729 ) ) ;
#41040 = CARTESIAN_POINT ( 'NONE',  ( 768.9521613784389729, -129.8272453906075725, -373.2346286133773106 ) ) ;
#41041 = ADVANCED_FACE ( 'NONE', ( #9229 ), #13158, .F. ) ;
#41042 = CARTESIAN_POINT ( 'NONE',  ( 808.0189434323515343, -446.0891481129646081, 319.0252816721025511 ) ) ;
#41044 = LINE ( 'NONE', #20017, #38112 ) ;
#41043 = CARTESIAN_POINT ( 'NONE',  ( -78.83651009197140525, 256.5000000000000568, -199.9999999999936051 ) ) ;
#41045 = CARTESIAN_POINT ( 'NONE',  ( 755.0488828828309806, -257.8055962898686744, -344.1219089521771934 ) ) ;
#41046 = ADVANCED_FACE ( 'NONE', ( #38325 ), #2280, .T. ) ;
#41047 = CARTESIAN_POINT ( 'NONE',  ( 762.1177392798416577, -114.5545181178803631, -309.8865473780659272 ) ) ;
#41048 = CARTESIAN_POINT ( 'NONE',  ( 789.8657795001898876, -452.9681489794449476, 362.9715936389367812 ) ) ;
#41049 = DIRECTION ( 'NONE',  ( -1.000000000000000000, -0.000000000000000000, -0.000000000000000000 ) ) ;
#41050 = AXIS2_PLACEMENT_3D ( 'NONE', #2755, #43861, #27919 ) ;
#41051 = CARTESIAN_POINT ( 'NONE',  ( 763.0428371773158460, -323.4636090269706301, 358.7617431975195359 ) ) ;
#41052 = CARTESIAN_POINT ( 'NONE',  ( 765.0180583372156207, -192.9982390220562820, 360.0135310231089534 ) ) ;
#41053 = EDGE_LOOP ( 'NONE', ( #34662, #38894, #36368, #34237 ) ) ;
#41054 = CARTESIAN_POINT ( 'NONE',  ( 786.2694204179717872, -309.2817908451525568, 305.1769319972829067 ) ) ;
#41055 = CARTESIAN_POINT ( 'NONE',  ( 744.7301800767020268, -172.8164208402381519, -337.4774526936615189 ) ) ;
#41056 = CARTESIAN_POINT ( 'NONE',  ( -858.8365100919713768, 260.0000000000002274, -191.9749999999881993 ) ) ;
#41057 = CARTESIAN_POINT ( 'NONE',  ( 766.4474001241216001, -115.0999726633348956, 307.3154664389482491 ) ) ;
#41058 = CARTESIAN_POINT ( 'NONE',  ( 763.2262854647970016, -296.6346026584195670, -309.2812353651462445 ) ) ;
#41059 = FACE_OUTER_BOUND ( 'NONE', #31743, .T. ) ;
#41060 = CARTESIAN_POINT ( 'NONE',  ( 794.9819416627830151, -156.9982390220564241, 319.9864689768909898 ) ) ;
#41061 = ORIENTED_EDGE ( 'NONE', *, *, #21315, .T. ) ;
#41062 = CARTESIAN_POINT ( 'NONE',  ( 752.7379699480933368, -420.0090635724249069, 361.9858362298580232 ) ) ;
#41063 = CARTESIAN_POINT ( 'NONE',  ( 786.2056067578752163, -347.8055962898683333, -374.4686193811670023 ) ) ;
#41064 = CARTESIAN_POINT ( 'NONE',  ( 815.2698199232961542, -112.8164208402383508, -342.5225473063383106 ) ) ;
#41065 = ADVANCED_FACE ( 'NONE', ( #30456, #2983, #34141 ), #27007, .T. ) ;
#41066 = CARTESIAN_POINT ( 'NONE',  ( 757.0176451133909268, -37.09997266333514432, 349.9200121543848354 ) ) ;
#41067 = CARTESIAN_POINT ( 'NONE',  ( 747.2067596250078623, -387.1800572038738437, -352.2312462859687230 ) ) ;
#41068 = DIRECTION ( 'NONE',  ( 0.000000000000000000, 0.000000000000000000, 1.000000000000000000 ) ) ;
#41069 = CARTESIAN_POINT ( 'NONE',  ( 756.1443688327750579, 26.37622189194863509, 314.3581564841659315 ) ) ;
#41070 = VECTOR ( 'NONE', #42421, 1000.000000000000000 ) ;
#41071 = ORIENTED_EDGE ( 'NONE', *, *, #44198, .F. ) ;
#41072 = VECTOR ( 'NONE', #13035, 1000.000000000000000 ) ;
#41073 = EDGE_CURVE ( 'NONE', #1769, #44135, #5760, .T. ) ;
#41074 = CARTESIAN_POINT ( 'NONE',  ( 800.0135310231082713, -230.0891481129652618, -325.0180583372163028 ) ) ;
#41075 = AXIS2_PLACEMENT_3D ( 'NONE', #23693, #26270, #12862 ) ;
#41076 = CARTESIAN_POINT ( 'NONE',  ( 751.2241431872005251, -160.1692326535053326, -359.9636004259367610 ) ) ;
#41077 = LINE ( 'NONE', #41305, #45471 ) ;
#41078 = CARTESIAN_POINT ( 'NONE',  ( 746.7653713866222915, -281.2601417444139997, 351.0478386215610271 ) ) ;
#41079 = CARTESIAN_POINT ( 'NONE',  ( 768.0187753319979720, -80.63460265842029173, 318.0580252608186242 ) ) ;
#41080 = ORIENTED_EDGE ( 'NONE', *, *, #28951, .F. ) ;
#41081 = VECTOR ( 'NONE', #2334, 1000.000000000000000 ) ;
#41082 = CARTESIAN_POINT ( 'NONE',  ( 805.1016975059191054, -6.896505380778533478, -343.0745993439771837 ) ) ;
#41083 = CARTESIAN_POINT ( 'NONE',  ( 804.6798772138708955, -255.7255117493287742, 334.6312213355107019 ) ) ;
#41084 = AXIS2_PLACEMENT_3D ( 'NONE', #11958, #36436, #26026 ) ;
#41085 = ADVANCED_FACE ( 'NONE', ( #12920 ), #41106, .F. ) ;
#41086 = CARTESIAN_POINT ( 'NONE',  ( 813.9316612368132837, -439.4419599262316751, -348.6739635108323228 ) ) ;
#41087 = DIRECTION ( 'NONE',  ( -0.000000000000000000, -0.000000000000000000, 1.000000000000000000 ) ) ;
#41088 = ORIENTED_EDGE ( 'NONE', *, *, #35748, .T. ) ;
#41089 = ORIENTED_EDGE ( 'NONE', *, *, #29222, .F. ) ;
#41090 = CARTESIAN_POINT ( 'NONE',  ( 783.7953271457878373, -368.1908817542433212, -375.1787889125761239 ) ) ;
#41092 = CARTESIAN_POINT ( 'NONE',  ( 815.0009284576459549, -222.3510508353233206, 338.7629533639073429 ) ) ;
#41091 = CARTESIAN_POINT ( 'NONE',  ( 804.7487373415286811, -331.5436935675104451, 364.7487373415288516 ) ) ;
#41093 = CARTESIAN_POINT ( 'NONE',  ( 759.0159684113467620, -232.9181544815163249, -325.8855110935213020 ) ) ;
#41094 = CARTESIAN_POINT ( 'NONE',  ( 774.6858677611749044, -201.7255117493290015, -315.5713283507209894 ) ) ;
#41095 = CARTESIAN_POINT ( 'NONE',  ( 797.8594530101009923, -421.5436935675101040, -322.1405469898982119 ) ) ;
#41096 = VERTEX_POINT ( 'NONE', #20532 ) ;
#41097 = CARTESIAN_POINT ( 'NONE',  ( 755.5713283507202505, -221.3618753856925707, 334.6858677611754729 ) ) ;
#41098 = CARTESIAN_POINT ( 'NONE',  ( 771.1735550268778070, -105.1800572038747248, -316.3353852180827630 ) ) ;
#41099 = VERTEX_POINT ( 'NONE', #6204 ) ;
#41100 = VECTOR ( 'NONE', #6904, 1000.000000000000000 ) ;
#41101 = CARTESIAN_POINT ( 'NONE',  ( 796.7737145352015204, -356.6346026584193964, 370.7187646348536987 ) ) ;
#41102 = DIRECTION ( 'NONE',  ( 0.000000000000000000, 0.000000000000000000, -1.000000000000000000 ) ) ;
#41103 = EDGE_CURVE ( 'NONE', #10523, #13769, #30705, .T. ) ;
#41104 = CARTESIAN_POINT ( 'NONE',  ( -769.9999999999992042, 205.0000000000000568, -319.9999999999999432 ) ) ;
#41105 = AXIS2_PLACEMENT_3D ( 'NONE', #34625, #15928, #30011 ) ;
#41106 = PLANE ( 'NONE',  #22381 ) ;
#41107 = CARTESIAN_POINT ( 'NONE',  ( 793.9708237608222134, -214.9181544815164386, 319.2295555964448681 ) ) ;
#41108 = CARTESIAN_POINT ( 'NONE',  ( 803.4237431249931660, -87.18005720387481006, 331.2633955100225194 ) ) ;
#41109 = VERTEX_POINT ( 'NONE', #3201 ) ;
#41110 = CARTESIAN_POINT ( 'NONE',  ( 768.9521613784389729, -441.8272453906066630, -373.2346286133773106 ) ) ;
#41111 = CARTESIAN_POINT ( 'NONE',  ( 777.5031285880264704, -70.81642084023850714, -374.9108240113588408 ) ) ;
#41112 = CARTESIAN_POINT ( 'NONE',  ( 798.7617431975189675, -243.6237781080504590, 323.0428371773161871 ) ) ;
#41113 = AXIS2_PLACEMENT_3D ( 'NONE', #5853, #23392, #37493 ) ;
#41114 = CARTESIAN_POINT ( 'NONE',  ( 788.7366044899766848, -419.9073299311465348, -316.5762568750059813 ) ) ;
#41115 = CARTESIAN_POINT ( 'NONE',  ( 804.6798772138710092, -39.72551174932951312, -334.6312213355106451 ) ) ;
#41116 = CARTESIAN_POINT ( 'NONE',  ( 815.3608509340175488, -2.736336299698892027, 341.2497674668889545 ) ) ;
#41117 = CARTESIAN_POINT ( 'NONE',  ( 795.1360043628807261, 3.910851887033985896, -360.2193346964456282 ) ) ;
#41118 = CARTESIAN_POINT ( 'NONE',  ( 763.0428371773158460, -275.4636090269708575, -358.7617431975195359 ) ) ;
#41119 = CARTESIAN_POINT ( 'NONE',  ( 751.6929314249748586, -198.9982390220562252, -318.8095938919659034 ) ) ;
#41120 = VECTOR ( 'NONE', #40326, 1000.000000000000000 ) ;
#41121 = CARTESIAN_POINT ( 'NONE',  ( 777.5031285880264704, -94.81642084023843609, 374.9108240113588408 ) ) ;
#41122 = CARTESIAN_POINT ( 'NONE',  ( 763.0537975583475827, -144.4527844766018632, 371.0346526505627480 ) ) ;
#41123 = CARTESIAN_POINT ( 'NONE',  ( 879.9999999999992042, 429.9999999999999432, -244.9999999999999716 ) ) ;
#41124 = CARTESIAN_POINT ( 'NONE',  ( 776.2433038121456548, -228.8965053807778816, -374.8207195650711014 ) ) ;
#41125 = EDGE_CURVE ( 'NONE', #5691, #6488, #17223, .T. ) ;
#41126 = CARTESIAN_POINT ( 'NONE',  ( 771.3260364891663130, -427.6454272087885897, 306.0683387631859773 ) ) ;
#41127 = CARTESIAN_POINT ( 'NONE',  ( 772.5602148656447525, -297.7255117493286889, -305.7998596910095443 ) ) ;
#41128 = LINE ( 'NONE', #15952, #3636 ) ;
#41129 = CARTESIAN_POINT ( 'NONE',  ( 747.2067596250078623, -387.1800572038738437, 352.2312462859687230 ) ) ;
#41130 = CARTESIAN_POINT ( 'NONE',  ( 745.4481719005789273, -3.725511749329622813, 347.5162901302853697 ) ) ;
#41131 = CARTESIAN_POINT ( 'NONE',  ( 800.2193346964447755, -354.9982390220557704, -355.1360043628815788 ) ) ;
#41132 = EDGE_CURVE ( 'NONE', #18880, #25919, #43749, .T. ) ;
#41133 = CARTESIAN_POINT ( 'NONE',  ( 779.4709603349208464, -24.35105083532392811, 314.7162404726379918 ) ) ;
#41134 = CARTESIAN_POINT ( 'NONE',  ( 752.7379699480933368, -84.00906357242590161, -361.9858362298580232 ) ) ;
#41135 = CARTESIAN_POINT ( 'NONE',  ( 789.9200121543843807, -169.9874144716871172, -317.0176451133914384 ) ) ;
#41136 = CARTESIAN_POINT ( 'NONE',  ( 754.0944755984390895, -159.6237781080508285, 364.1009440267246760 ) ) ;
#41137 = CARTESIAN_POINT ( 'NONE',  ( 788.7366044899766848, 12.09267006885214180, 316.5762568750059813 ) ) ;
#41138 = VERTEX_POINT ( 'NONE', #27688 ) ;
#41139 = CARTESIAN_POINT ( 'NONE',  ( 778.2165204200184689, -70.81642084023850714, -364.9363028652563230 ) ) ;
#41140 = CARTESIAN_POINT ( 'NONE',  ( 794.1144889064781864, -154.1692326535053894, -360.9840315886528401 ) ) ;
#41141 = CARTESIAN_POINT ( 'NONE',  ( 803.6646147819161570, -161.9073299311472454, 348.8264449731210561 ) ) ;
#41142 = CARTESIAN_POINT ( 'NONE',  ( 771.2368401574024119, 10.55804007376686826, -374.2805881961240857 ) ) ;
#41144 = CARTESIAN_POINT ( 'NONE',  ( 800.2193346964446619, -282.9982390220559409, 355.1360043628816925 ) ) ;
#41143 = CARTESIAN_POINT ( 'NONE',  ( 755.0636971347428243, -292.2709662947831930, 341.7834795799807353 ) ) ;
#41145 = FACE_OUTER_BOUND ( 'NONE', #9136, .T. ) ;
#41146 = ORIENTED_EDGE ( 'NONE', *, *, #21098, .T. ) ;
#41147 = CARTESIAN_POINT ( 'NONE',  ( 765.8855110935204493, -22.16923265350575889, 319.0159684113471599 ) ) ;
#41148 = CARTESIAN_POINT ( 'NONE',  ( 807.2620300519052989, -288.0090635724252479, -318.0141637701419768 ) ) ;
#41149 = CIRCLE ( 'NONE', #16080, 6.119000000000013095 ) ;
#41150 = ORIENTED_EDGE ( 'NONE', *, *, #1475, .T. ) ;
#41151 = CARTESIAN_POINT ( 'NONE',  ( 0.000000000000000000, 0.000000000000000000, 0.000000000000000000 ) ) ;
#41152 = CARTESIAN_POINT ( 'NONE',  ( 810.7187646348534145, -210.4527844766016926, 356.7737145352016341 ) ) ;
#41153 = CARTESIAN_POINT ( 'NONE',  ( 790.0220218866281812, -295.0999726633343698, 363.2186876482849129 ) ) ;
#41154 = CARTESIAN_POINT ( 'NONE',  ( 764.3348316497523456, 25.28531280103955226, 308.6759233522265617 ) ) ;
#41155 = ORIENTED_EDGE ( 'NONE', *, *, #15105, .F. ) ;
#41156 = CARTESIAN_POINT ( 'NONE',  ( 802.5472867521000353, -100.3726999360622187, -350.8726784830461156 ) ) ;
#41157 = CARTESIAN_POINT ( 'NONE',  ( 768.0187753319979720, -104.6346026584202207, -318.0580252608186242 ) ) ;
#41158 = CARTESIAN_POINT ( 'NONE',  ( 755.3201227861273992, -315.7255117493286320, -345.3687786644892981 ) ) ;
#41159 = ORIENTED_EDGE ( 'NONE', *, *, #42189, .F. ) ;
#41160 = CARTESIAN_POINT ( 'NONE',  ( 756.5762568750052424, -435.1800572038737869, -348.7366044899774238 ) ) ;
#41161 = CARTESIAN_POINT ( 'NONE',  ( 789.9200121543843807, -313.9874144716866908, 317.0176451133914384 ) ) ;
#41162 = DIRECTION ( 'NONE',  ( 0.000000000000000000, 0.000000000000000000, -1.000000000000000000 ) ) ;
#41163 = DIRECTION ( 'NONE',  ( -1.000000000000000000, -0.000000000000000000, -0.000000000000000000 ) ) ;
#41164 = CARTESIAN_POINT ( 'NONE',  ( 800.9840315886518738, -124.9181544815167086, 354.1144889064786412 ) ) ;
#41165 = CARTESIAN_POINT ( 'NONE',  ( 989.9999999999992042, -190.2822455671962416, -69.00746428064729798 ) ) ;
#41166 = VERTEX_POINT ( 'NONE', #6671 ) ;
#41167 = CARTESIAN_POINT ( 'NONE',  ( 811.3240766477731540, -340.3726999360615082, -355.6651683502462902 ) ) ;
#41168 = CARTESIAN_POINT ( 'NONE',  ( 764.1737431748507561, -202.3726999360618777, 371.6461892240376415 ) ) ;
#41169 = CARTESIAN_POINT ( 'NONE',  ( 768.0187753319979720, -320.6346026584195670, -318.0580252608186242 ) ) ;
#41170 = CARTESIAN_POINT ( 'NONE',  ( 799.2566176426618085, -192.0090635724255606, -324.0069404352559559 ) ) ;
#41171 = CARTESIAN_POINT ( 'NONE',  ( 777.4774526936600978, -34.27096629478407408, 304.7301800767027657 ) ) ;
#41172 = FACE_OUTER_BOUND ( 'NONE', #26727, .T. ) ;
#41173 = CARTESIAN_POINT ( 'NONE',  ( 751.9810565676468741, -386.0891481129647786, -360.9747183278973921 ) ) ;
#41174 = VECTOR ( 'NONE', #32344, 1000.000000000000000 ) ;
#41175 = CARTESIAN_POINT ( 'NONE',  ( 799.9636004259356241, -334.9181544815160692, 311.2241431872006956 ) ) ;
#41176 = DIRECTION ( 'NONE',  ( 0.000000000000000000, 0.000000000000000000, 1.000000000000000000 ) ) ;
#41177 = CARTESIAN_POINT ( 'NONE',  ( 758.8095938919642549, -296.0891481129650629, 311.6929314249763365 ) ) ;
#41178 = CARTESIAN_POINT ( 'NONE',  ( 754.9967657858570647, -25.54369356751136877, -365.0032342141425374 ) ) ;
#41179 = CARTESIAN_POINT ( 'NONE',  ( 774.6312213355099630, -263.3618753856924855, -364.6798772138717482 ) ) ;
#41180 = LINE ( 'NONE', #9755, #29873 ) ;
#41181 = CARTESIAN_POINT ( 'NONE',  ( 756.3353852180819104, -389.9073299311465348, 331.1735550268788302 ) ) ;
#41182 = CARTESIAN_POINT ( 'NONE',  ( 769.9779781133707957, -115.0999726633348956, 316.7813123517150871 ) ) ;
#41183 = CARTESIAN_POINT ( 'NONE',  ( 805.1016975059191054, -54.89650538077837183, -343.0745993439771837 ) ) ;
#41184 = CARTESIAN_POINT ( 'NONE',  ( 766.5853460496234675, -61.98741447168745822, 372.3518521366060554 ) ) ;
#41185 = CARTESIAN_POINT ( 'NONE',  ( 762.1405469898973024, -361.5436935675103882, 357.8594530101016176 ) ) ;
#41186 = CARTESIAN_POINT ( 'NONE',  ( 814.9108240113580450, 7.729033705215793582, 337.5031285880265273 ) ) ;
#41187 = FACE_OUTER_BOUND ( 'NONE', #22314, .T. ) ;
#41188 = CARTESIAN_POINT ( 'NONE',  ( 764.3348316497523456, -142.7146871989599219, 308.6759233522265617 ) ) ;
#41189 = CARTESIAN_POINT ( 'NONE',  ( 794.9819416627830151, -444.9982390220554862, 319.9864689768909898 ) ) ;
#41190 = VERTEX_POINT ( 'NONE', #20746 ) ;
#41191 = CARTESIAN_POINT ( 'NONE',  ( 771.1735550268778070, -57.18005720387489532, -316.3353852180827630 ) ) ;
#41192 = CARTESIAN_POINT ( 'NONE',  ( 754.9735926884551418, -354.3510508353228943, -340.5236548041000333 ) ) ;
#41194 = CARTESIAN_POINT ( 'NONE',  ( 781.7834795799800531, -202.8164208402380950, 315.0636971347436202 ) ) ;
#41193 = CARTESIAN_POINT ( 'NONE',  ( 795.1360043628807261, -188.0891481129653187, 360.2193346964456282 ) ) ;
#41195 = CARTESIAN_POINT ( 'NONE',  ( 748.3538107759620743, -376.7146871989592682, -355.8262568251490165 ) ) ;
#41196 = LINE ( 'NONE', #9770, #11644 ) ;
#41197 = VERTEX_POINT ( 'NONE', #2758 ) ;
#41198 = CARTESIAN_POINT ( 'NONE',  ( 785.3141322388236176, -381.7255117493284615, 364.4286716492789537 ) ) ;
#41199 = EDGE_LOOP ( 'NONE', ( #43784, #33243, #36344, #13483 ) ) ;
#41200 = CARTESIAN_POINT ( 'NONE',  ( 751.9810565676468741, -218.0891481129653187, -360.9747183278973921 ) ) ;
#41201 = CARTESIAN_POINT ( 'NONE',  ( 787.4397851343537695, -117.7255117493292715, 374.2001403089903988 ) ) ;
#41202 = VERTEX_POINT ( 'NONE', #34626 ) ;
#41203 = CARTESIAN_POINT ( 'NONE',  ( 756.3353852180820240, -221.9073299311471033, -331.1735550268787733 ) ) ;
#41204 = ORIENTED_EDGE ( 'NONE', *, *, #28363, .T. ) ;
#41205 = VECTOR ( 'NONE', #44632, 1000.000000000000114 ) ;
#41206 = CARTESIAN_POINT ( 'NONE',  ( 774.6858677611749044, -321.7255117493286320, -315.5713283507209894 ) ) ;
#41207 = CARTESIAN_POINT ( 'NONE',  ( 796.1575198192839480, -462.0090635724247932, -359.4546378042384163 ) ) ;
#41208 = CARTESIAN_POINT ( 'NONE',  ( 745.7998596910086917, -269.3618753856924286, 332.5602148656461168 ) ) ;
#41209 = CARTESIAN_POINT ( 'NONE',  ( 794.1144889064781864, -178.1692326535052473, 360.9840315886528401 ) ) ;
#41211 = CARTESIAN_POINT ( 'NONE',  ( -338.8365100919713200, 260.0000000000001137, -197.2499999999919282 ) ) ;
#41210 = FACE_BOUND ( 'NONE', #43196, .T. ) ;
#41212 = CARTESIAN_POINT ( 'NONE',  ( 746.4999999999993179, -359.5698779088871788, -26.28906389436294688 ) ) ;
#41213 = EDGE_LOOP ( 'NONE', ( #10638, #41591, #3711, #28833 ) ) ;
#41214 = CARTESIAN_POINT ( 'NONE',  ( 805.2837595273609850, -458.7363362996973706, -340.5290396650784714 ) ) ;
#41215 = CARTESIAN_POINT ( 'NONE',  ( -919.9999999999993179, 154.9999999999998863, 339.9999999999999432 ) ) ;
#41216 = CARTESIAN_POINT ( 'NONE',  ( -879.9999999999992042, 240.0000000000002274, -219.9999999999999716 ) ) ;
#41217 = CARTESIAN_POINT ( 'NONE',  ( 805.6418435158337843, -245.4636090269709143, -363.8556311672236916 ) ) ;
#41218 = CARTESIAN_POINT ( 'NONE',  ( 768.9521613784389729, -105.8272453906076578, 373.2346286133773106 ) ) ;
#41220 = CARTESIAN_POINT ( 'NONE',  ( 764.8639956371174549, -224.0891481129653187, -319.7806653035542013 ) ) ;
#41219 = FACE_OUTER_BOUND ( 'NONE', #13344, .T. ) ;
#41221 = CARTESIAN_POINT ( 'NONE',  ( 755.0488828828309806, -353.8055962898683333, -344.1219089521771934 ) ) ;
#41222 = CARTESIAN_POINT ( 'NONE',  ( 773.7305795820266212, -249.2817908451526421, -374.8230680027170365 ) ) ;
#41223 = DIRECTION ( 'NONE',  ( 0.000000000000000000, 0.000000000000000000, 1.000000000000000000 ) ) ;
#41224 = LINE ( 'NONE', #13276, #27501 ) ;
#41225 = CARTESIAN_POINT ( 'NONE',  ( 769.9779781133707957, -67.09997266333506616, -316.7813123517150871 ) ) ;
#41226 = CARTESIAN_POINT ( 'NONE',  ( 763.8424801807145741, -426.0090635724247932, 320.5453621957614700 ) ) ;
#41227 = DIRECTION ( 'NONE',  ( -1.000000000000000000, -0.000000000000000000, -0.000000000000000000 ) ) ;
#41228 = CARTESIAN_POINT ( 'NONE',  ( 815.2698199232962679, -280.8164208402378108, -342.5225473063383674 ) ) ;
#41229 = DIRECTION ( 'NONE',  ( 0.000000000000000000, 0.000000000000000000, 1.000000000000000000 ) ) ;
#41230 = CARTESIAN_POINT ( 'NONE',  ( -786.4999999999993179, -563.3203001761230553, -342.3463313526983143 ) ) ;
#41231 = CARTESIAN_POINT ( 'NONE',  ( 781.8018195045266339, -46.27096629478404566, -365.1927285166406705 ) ) ;
#41232 = CARTESIAN_POINT ( 'NONE',  ( 766.4474001241216001, -211.0999726633346540, 307.3154664389482491 ) ) ;
#41233 = CARTESIAN_POINT ( 'NONE',  ( 756.1443688327750579, -165.6237781080507716, -314.3581564841659315 ) ) ;
#41234 = CARTESIAN_POINT ( 'NONE',  ( 804.7487373415286811, -187.5436935675108430, 364.7487373415288516 ) ) ;
#41235 = CARTESIAN_POINT ( 'NONE',  ( 808.0189434323515343, -398.0891481129647218, -319.0252816721025511 ) ) ;
#41236 = CARTESIAN_POINT ( 'NONE',  ( 939.9999999999993179, -590.0000000000001137, 360.0000000000000000 ) ) ;
#41237 = CARTESIAN_POINT ( 'NONE',  ( 785.3141322388236176, -261.7255117493288026, 364.4286716492789537 ) ) ;
#41238 = ADVANCED_FACE ( 'NONE', ( #27453 ), #23976, .F. ) ;
#41239 = CARTESIAN_POINT ( 'NONE',  ( 801.5560724626406000, -48.55451811788057626, 326.7756240680316182 ) ) ;
#41240 = CARTESIAN_POINT ( 'NONE',  ( 804.6798772138708955, -423.7255117493281205, -334.6312213355107019 ) ) ;
#41241 = AXIS2_PLACEMENT_3D ( 'NONE', #15509, #42988, #945 ) ;
#41242 = LINE ( 'NONE', #3112, #10680 ) ;
#41243 = CARTESIAN_POINT ( 'NONE',  ( -468.8365100919714337, 260.0000000000001705, -191.9749999999908709 ) ) ;
#41245 = CARTESIAN_POINT ( 'NONE',  ( 754.8072714833581358, -340.8164208402376971, 338.1981804954720587 ) ) ;
#41244 = CARTESIAN_POINT ( 'NONE',  ( 759.2295555964440155, -88.16923265350555994, 353.9708237608231229 ) ) ;
#41246 = VERTEX_POINT ( 'NONE', #45244 ) ;
#41247 = CARTESIAN_POINT ( 'NONE',  ( 773.3843516231979720, -253.4419599262323572, -364.4086373105754433 ) ) ;
#41248 = CARTESIAN_POINT ( 'NONE',  ( 757.8323909638827445, -74.63460265842032015, 352.1044303154654358 ) ) ;
#41249 = CARTESIAN_POINT ( 'NONE',  ( 752.4576283171824116, -261.0783235625959264, -317.7880784355627952 ) ) ;
#41250 = FACE_OUTER_BOUND ( 'NONE', #32286, .T. ) ;
#41251 = CARTESIAN_POINT ( 'NONE',  ( 793.4146539503750546, -385.9874144716864066, 307.6481478633938877 ) ) ;
#41252 = ORIENTED_EDGE ( 'NONE', *, *, #20953, .T. ) ;
#41253 = CARTESIAN_POINT ( 'NONE',  ( 805.1927285166397041, -304.8164208402376403, 341.8018195045277707 ) ) ;
#41254 = CARTESIAN_POINT ( 'NONE',  ( 787.5162901302840055, 12.63812461430668321, 305.4481719005792684 ) ) ;
#41255 = CARTESIAN_POINT ( 'NONE',  ( 775.9200461376533440, -23.80559628986938847, -315.3028492785443291 ) ) ;
#41256 = CARTESIAN_POINT ( 'NONE',  ( 802.1676090361156639, -158.6346026584199933, -327.8955696845344505 ) ) ;
#41257 = CARTESIAN_POINT ( 'NONE',  ( 785.3141322388236176, -381.7255117493284615, 364.4286716492789537 ) ) ;
#41258 = CARTESIAN_POINT ( 'NONE',  ( 746.8695393053150156, -101.9073299311474727, -327.6429770376306010 ) ) ;
#41259 = CARTESIAN_POINT ( 'NONE',  ( 801.9419747391806368, -90.45278447660209054, -351.9812246680014027 ) ) ;
#41260 = VERTEX_POINT ( 'NONE', #34838 ) ;
#41261 = CARTESIAN_POINT ( 'NONE',  ( 763.0428371773158460, -35.46360902697151829, -358.7617431975195359 ) ) ;
#41262 = CARTESIAN_POINT ( 'NONE',  ( 763.8424801807145741, -354.0090635724250774, -320.5453621957614700 ) ) ;
#41264 = CARTESIAN_POINT ( 'NONE',  ( 755.5913626894240451, -421.6454272087885329, 346.6156483768012890 ) ) ;
#41263 = CARTESIAN_POINT ( 'NONE',  ( 756.3353852180819104, -101.9073299311474727, 331.1735550268788302 ) ) ;
#41265 = CARTESIAN_POINT ( 'NONE',  ( 804.1601925771018387, -103.4419599262327836, 346.5483106153029098 ) ) ;
#41268 = CARTESIAN_POINT ( 'NONE',  ( 808.7758568127978833, -340.1692326535047641, 320.0363995740631822 ) ) ;
#41267 = FACE_OUTER_BOUND ( 'NONE', #11965, .T. ) ;
#41266 = CARTESIAN_POINT ( 'NONE',  ( 914.9999999999992042, 99.99999999999984368, -360.0000000000000000 ) ) ;
#41269 = VECTOR ( 'NONE', #10544, 1000.000000000000000 ) ;
#41270 = CARTESIAN_POINT ( 'NONE',  ( 766.0291762391763086, -370.9181544815159555, -360.7704444035551319 ) ) ;
#41271 = CARTESIAN_POINT ( 'NONE',  ( 795.1360043628807261, -308.0891481129650629, -360.2193346964456282 ) ) ;
#41272 = CARTESIAN_POINT ( 'NONE',  ( 812.3518521366052028, -121.0999726633348956, -326.5853460496235243 ) ) ;
#41273 = CONICAL_SURFACE ( 'NONE', #16942, 8.025000000000003908, 0.7853981633974482790 ) ;
#41274 = CARTESIAN_POINT ( 'NONE',  ( 813.1304606946830518, -449.9073299311463643, 352.3570229623690580 ) ) ;
#41276 = DIRECTION ( 'NONE',  ( -0.000000000000000000, 1.000000000000000000, -0.000000000000000000 ) ) ;
#41275 = FACE_OUTER_BOUND ( 'NONE', #3682, .T. ) ;
#41277 = CARTESIAN_POINT ( 'NONE',  ( 765.8855110935204493, -262.1692326535049347, -319.0159684113471599 ) ) ;
#41278 = CARTESIAN_POINT ( 'NONE',  ( 788.6739635108323228, -127.6454272087894140, -373.9316612368139090 ) ) ;
#41279 = CARTESIAN_POINT ( 'NONE',  ( 939.9999999999993179, 50.81038600091411439, 193.6948738798775764 ) ) ;
#41280 = LINE ( 'NONE', #37809, #6069 ) ;
#41281 = CARTESIAN_POINT ( 'NONE',  ( 793.0897708529556667, -342.5545181178796952, 361.3366627262616362 ) ) ;
#41282 = VERTEX_POINT ( 'NONE', #44327 ) ;
#41283 = CARTESIAN_POINT ( 'NONE',  ( 760.0363995740630116, -298.9181544815161828, 368.7758568127991907 ) ) ;
#41284 = CARTESIAN_POINT ( 'NONE',  ( 812.7932403749906598, -159.1800572038746111, -327.7687537140311633 ) ) ;
#41285 = FACE_OUTER_BOUND ( 'NONE', #920, .T. ) ;
#41286 =( BOUNDED_CURVE ( )  B_SPLINE_CURVE ( 2, ( #31222, #6973, #20813, #21058, #17829, #10206, #31897, #38389, #269, #6517, #13680, #39087, #35142 ),
 .UNSPECIFIED., .F., .T. ) 
 B_SPLINE_CURVE_WITH_KNOTS ( ( 3, 2, 2, 2, 2, 2, 3 ),
 ( 0.000000000000000000, 0.0008527428137030668154, 0.003125470086430381933, 0.005398197359157586028, 0.007670924631884902013, 0.009943651904612216264, 0.01049328897333767253 ),
 .UNSPECIFIED. ) 
 CURVE ( )  GEOMETRIC_REPRESENTATION_ITEM ( )  RATIONAL_B_SPLINE_CURVE ( ( 0.4976140944542620792, 0.4980906878130254567, 0.5000002209606652093, 0.4949109396520706139, 0.5000002209606652093, 0.4949109396520706139, 0.5000002209606652093, 0.4949109396520706139, 0.5000002209606652093, 0.4949109396520706139, 0.5000002209606652093, 0.4987694275901001228, 0.4981339451206906466 ) ) 
 REPRESENTATION_ITEM ( '' )  );
#41287 = CARTESIAN_POINT ( 'NONE',  ( 744.6391490659812007, -110.7363362996985501, 338.7502325331110455 ) ) ;
#41288 = CARTESIAN_POINT ( 'NONE',  ( 787.4397851343537695, -309.7255117493287457, -374.2001403089903988 ) ) ;
#41289 = ADVANCED_FACE ( 'NONE', ( #7594 ), #434, .F. ) ;
#41290 = CARTESIAN_POINT ( 'NONE',  ( 911.9749999999993406, 219.9999999999998863, 360.0000000000000000 ) ) ;
#41291 = CARTESIAN_POINT ( 'NONE',  ( 799.9999999999993179, 197.3292319334027241, 273.4704985657796783 ) ) ;
#41292 = CARTESIAN_POINT ( 'NONE',  ( 803.4237431249931660, -135.1800572038746679, 331.2633955100225194 ) ) ;
#41293 = EDGE_LOOP ( 'NONE', ( #42221, #13656, #14064, #16824 ) ) ;
#41294 = EDGE_CURVE ( 'NONE', #15262, #11223, #18234, .T. ) ;
#41295 = CARTESIAN_POINT ( 'NONE',  ( 807.2620300519052989, -432.0090635724247932, 318.0141637701419768 ) ) ;
#41296 = CARTESIAN_POINT ( 'NONE',  ( 805.9055244015594326, -387.6237781080499758, -315.8990559732753240 ) ) ;
#41297 = CARTESIAN_POINT ( 'NONE',  ( 747.2067596250078623, -123.1800572038747106, -352.2312462859687230 ) ) ;
#41298 = CARTESIAN_POINT ( 'NONE',  ( 760.7433823573367135, -36.00906357242605793, 355.9930595647440441 ) ) ;
#41299 = CARTESIAN_POINT ( 'NONE',  ( 796.7737145352015204, -380.6346026584192828, -370.7187646348536987 ) ) ;
#41300 = CARTESIAN_POINT ( 'NONE',  ( -521.6730038022808458, 240.0000000000001705, -122.7905160835438068 ) ) ;
#41301 = CARTESIAN_POINT ( 'NONE',  ( 796.7845633553578182, -417.6237781080499190, 358.5707757039688204 ) ) ;
#41302 = ORIENTED_EDGE ( 'NONE', *, *, #15175, .F. ) ;
#41303 = CARTESIAN_POINT ( 'NONE',  ( 774.6312213355099630, -263.3618753856924855, 364.6798772138717482 ) ) ;
#41304 = CARTESIAN_POINT ( 'NONE',  ( 801.9858362298568863, -147.0783235625962959, -312.7379699480935642 ) ) ;
#41305 = CARTESIAN_POINT ( 'NONE',  ( 799.9999999999993179, 205.0000000000000568, -245.0000000000000284 ) ) ;
#41306 = CARTESIAN_POINT ( 'NONE',  ( 798.0661480581538854, -266.5328690171413655, 309.5768839229118043 ) ) ;
#41307 = CARTESIAN_POINT ( 'NONE',  ( 759.9864689768902508, -98.08914811296568814, 354.9819416627836404 ) ) ;
#41308 = ORIENTED_EDGE ( 'NONE', *, *, #39488, .F. ) ;
#41309 = CARTESIAN_POINT ( 'NONE',  ( 798.7617431975189675, -3.623778108051270319, -323.0428371773161871 ) ) ;
#41310 = CARTESIAN_POINT ( 'NONE',  ( 781.8018195045266339, -262.2709662947831930, 365.1927285166406705 ) ) ;
#41311 = CARTESIAN_POINT ( 'NONE',  ( 759.0252816721024374, -0.9982390220569063999, -368.0189434323527280 ) ) ;
#41312 = CARTESIAN_POINT ( 'NONE',  ( 571.1634899080285095, 259.9999999999999432, -199.9999999999981526 ) ) ;
#41313 = ORIENTED_EDGE ( 'NONE', *, *, #25587, .T. ) ;
#41314 = ORIENTED_EDGE ( 'NONE', *, *, #7816, .F. ) ;
#41315 = CARTESIAN_POINT ( 'NONE',  ( 803.4237431249931660, -183.1800572038744974, -331.2633955100225194 ) ) ;
#41316 = CARTESIAN_POINT ( 'NONE',  ( 749.5768839229115201, -396.5545181178794678, -358.0661480581553064 ) ) ;
#41317 = CARTESIAN_POINT ( 'NONE',  ( 792.1044303154645831, -276.4527844766013800, -317.8323909638837677 ) ) ;
#41319 = CARTESIAN_POINT ( 'NONE',  ( 749.8865473780648472, -260.5328690171413086, 322.1177392798429082 ) ) ;
#41318 = CARTESIAN_POINT ( 'NONE',  ( 758.8095938919644823, -344.0891481129648355, 311.6929314249762797 ) ) ;
#41320 = CARTESIAN_POINT ( 'NONE',  ( 790.9844846989617508, -238.3726999360617640, -317.2208543904092721 ) ) ;
#41321 = CARTESIAN_POINT ( 'NONE',  ( 762.3223304703356007, -223.5436935675107577, -322.3223304703362828 ) ) ;
#41322 = CARTESIAN_POINT ( 'NONE',  ( 759.7806653035535192, -414.9982390220555430, -324.8639956371181370 ) ) ;
#41323 = CARTESIAN_POINT ( 'NONE',  ( 788.8264449731200330, -261.1800572038741848, 363.6646147819171233 ) ) ;
#41324 = VERTEX_POINT ( 'NONE', #25361 ) ;
#41325 = CARTESIAN_POINT ( 'NONE',  ( 755.2512626584698410, -367.5436935675102745, 315.2512626584710915 ) ) ;
#41326 = CARTESIAN_POINT ( 'NONE',  ( -208.8365100919714052, 258.0940000000001078, -206.1189999999926954 ) ) ;
#41327 = CARTESIAN_POINT ( 'NONE',  ( 795.8262568251477660, -22.37269993606246743, -308.3538107759623585 ) ) ;
#41328 = LINE ( 'NONE', #2279, #45498 ) ;
#41329 = DIRECTION ( 'NONE',  ( 0.000000000000000000, 0.000000000000000000, 1.000000000000000000 ) ) ;
#41330 = EDGE_CURVE ( 'NONE', #44890, #15534, #4697, .T. ) ;
#41331 = CARTESIAN_POINT ( 'NONE',  ( 784.1219089521767955, -213.2817908451527842, 315.0488828828318333 ) ) ;
#41332 = CARTESIAN_POINT ( 'NONE',  ( 801.9419747391806368, -90.45278447660209054, 351.9812246680014027 ) ) ;
#41333 = CARTESIAN_POINT ( 'NONE',  ( 788.6739635108323228, -439.6454272087884760, -373.9316612368139090 ) ) ;
#41334 = CARTESIAN_POINT ( 'NONE',  ( 782.5225473063383106, -70.27096629478397460, -375.2698199232970637 ) ) ;
#41335 = CARTESIAN_POINT ( 'NONE',  ( 765.8855110935204493, -262.1692326535049347, 319.0159684113471599 ) ) ;
#41336 = CARTESIAN_POINT ( 'NONE',  ( 795.1360043628807261, -428.0891481129644944, -360.2193346964456282 ) ) ;
#41337 = CARTESIAN_POINT ( 'NONE',  ( 804.4286716492782716, -41.36187538569314626, -345.3141322388244703 ) ) ;
#41338 = CARTESIAN_POINT ( 'NONE',  ( 748.6759233522253680, -16.37269993606248519, 324.3348316497537098 ) ) ;
#41339 = CARTESIAN_POINT ( 'NONE',  ( 181.1634899080285948, 260.0000000000000000, -208.0249999999954014 ) ) ;
#41340 = CARTESIAN_POINT ( 'NONE',  ( 755.8894580844503253, -279.8272453906071746, -332.3691319403863531 ) ) ;
#41341 = CARTESIAN_POINT ( 'NONE',  ( 772.4837098697144029, -191.3618753856925991, -374.5518280994205611 ) ) ;
#41342 = EDGE_CURVE ( 'NONE', #38409, #29779, #17540, .T. ) ;
#41343 = CARTESIAN_POINT ( 'NONE',  ( 745.0891759886404770, -100.2709662947838609, 342.4968714119734159 ) ) ;
#41344 = CARTESIAN_POINT ( 'NONE',  ( 812.7932403749906598, -135.1800572038746679, 327.7687537140311633 ) ) ;
#41345 = CARTESIAN_POINT ( 'NONE',  ( -468.8365100919714337, 258.0940000000001646, -193.8809999999909053 ) ) ;
#41346 = DIRECTION ( 'NONE',  ( 0.000000000000000000, 1.000000000000000000, 0.000000000000000000 ) ) ;
#41347 = CARTESIAN_POINT ( 'NONE',  ( 759.8311093483677041, -286.1692326535048778, -310.9282345327691814 ) ) ;
#41348 = CARTESIAN_POINT ( 'NONE',  ( 766.4474001241216001, -427.0999726633338582, 307.3154664389482491 ) ) ;
#41349 = CARTESIAN_POINT ( 'NONE',  ( 804.7487373415286811, -283.5436935675105019, -364.7487373415288516 ) ) ;
#41350 = CARTESIAN_POINT ( 'NONE',  ( -78.83651009197140525, 230.0000000000000568, -199.9999999999936051 ) ) ;
#41351 = CARTESIAN_POINT ( 'NONE',  ( 777.5031285880264704, -382.8164208402374697, 374.9108240113588408 ) ) ;
#41352 = CARTESIAN_POINT ( 'NONE',  ( 805.0032342141413437, -13.54369356751140963, 314.9967657858572352 ) ) ;
#41353 = CARTESIAN_POINT ( 'NONE',  ( 785.3687786644884454, -347.3618753856922012, -315.3201227861279676 ) ) ;
#41354 = CARTESIAN_POINT ( 'NONE',  ( 789.9200121543843807, -1.987414471687640294, 317.0176451133914384 ) ) ;
#41355 = CARTESIAN_POINT ( 'NONE',  ( 746.0683387631852383, -43.44195992623296831, -331.3260364891676204 ) ) ;
#41356 = CARTESIAN_POINT ( 'NONE',  ( 784.0799538623451781, -155.8055962898689586, -364.6971507214555572 ) ) ;
#41357 = EDGE_CURVE ( 'NONE', #38523, #27925, #35762, .T. ) ;
#41358 = CARTESIAN_POINT ( 'NONE',  ( 781.2497674668890113, -180.3510508353234343, 375.3608509340180603 ) ) ;
#41359 = DIRECTION ( 'NONE',  ( 0.000000000000000000, 0.000000000000000000, 1.000000000000000000 ) ) ;
#41360 = ADVANCED_FACE ( 'NONE', ( #45487 ), #21221, .T. ) ;
#41361 = CARTESIAN_POINT ( 'NONE',  ( 781.2497674668890113, -180.3510508353234343, 375.3608509340180603 ) ) ;
#41362 = ORIENTED_EDGE ( 'NONE', *, *, #13125, .T. ) ;
#41363 = CARTESIAN_POINT ( 'NONE',  ( 781.8018195045266339, -70.27096629478397460, -365.1927285166406705 ) ) ;
#41364 = CARTESIAN_POINT ( 'NONE',  ( 770.0799878456142551, -157.9874144716871456, -362.9823548866085616 ) ) ;
#41365 = PRODUCT_DEFINITION_CONTEXT ( 'detailed design', #11927, 'design' ) ;
#41366 = CARTESIAN_POINT ( 'NONE',  ( 788.7366044899766848, -155.9073299311473306, 316.5762568750059813 ) ) ;
#41367 = CARTESIAN_POINT ( 'NONE',  ( 786.2056067578752163, 12.19440371013049784, -374.4686193811670023 ) ) ;
#41369 = CARTESIAN_POINT ( 'NONE',  ( 804.9363028652555840, -304.2709662947832499, 338.2165204200192079 ) ) ;
#41368 = CARTESIAN_POINT ( 'NONE',  ( 767.8955696845333705, -288.4527844766014937, 362.1676090361162323 ) ) ;
#41370 = CARTESIAN_POINT ( 'NONE',  ( 779.9999999999990905, 18.49609980828599376, -309.9999999999999432 ) ) ;
#41371 = ORIENTED_EDGE ( 'NONE', *, *, #31758, .T. ) ;
#41372 = CARTESIAN_POINT ( 'NONE',  ( 795.9930595647434757, -27.07832356259665474, 320.7433823573372820 ) ) ;
#41373 = CARTESIAN_POINT ( 'NONE',  ( 768.9521613784389729, -321.8272453906070609, -373.2346286133773106 ) ) ;
#41374 = APPLICATION_PROTOCOL_DEFINITION ( 'draft international standard', 'automotive_design', 1998, #30200 ) ;
#41375 = CARTESIAN_POINT ( 'NONE',  ( 758.8095938919644823, -224.0891481129652902, 311.6929314249762797 ) ) ;
#41376 = CARTESIAN_POINT ( 'NONE',  ( 784.1219089521767955, -333.2817908451523863, 315.0488828828318333 ) ) ;
#41377 = CARTESIAN_POINT ( 'NONE',  ( 776.9566956441375396, -420.8965053807772279, 364.8461984189686405 ) ) ;
#41378 = CARTESIAN_POINT ( 'NONE',  ( 804.1105419155481968, -99.82724539060768620, -347.6308680596136469 ) ) ;
#41379 = CARTESIAN_POINT ( 'NONE',  ( 759.7806653035534055, -126.9982390220565094, -324.8639956371180801 ) ) ;
#41380 = CARTESIAN_POINT ( 'NONE',  ( 804.9363028652555840, -304.2709662947832499, -338.2165204200192079 ) ) ;
#41381 = ORIENTED_EDGE ( 'NONE', *, *, #6043, .F. ) ;
#41382 = CARTESIAN_POINT ( 'NONE',  ( 804.4286716492782716, -425.3618753856919170, -345.3141322388244703 ) ) ;
#41383 = EDGE_CURVE ( 'NONE', #15632, #39395, #45717, .T. ) ;
#41384 = CARTESIAN_POINT ( 'NONE',  ( 766.7756240680305382, -302.5328690171411949, 361.5560724626415663 ) ) ;
#41385 = LINE ( 'NONE', #9732, #45501 ) ;
#41386 = ADVANCED_FACE ( 'NONE', ( #27922, #32309, #7370 ), #32063, .F. ) ;
#41387 = CARTESIAN_POINT ( 'NONE',  ( 780.5236548040995785, -116.7363362996985217, 314.9735926884559944 ) ) ;
#41388 = FACE_OUTER_BOUND ( 'NONE', #5183, .T. ) ;
#41389 = EDGE_LOOP ( 'NONE', ( #42670, #16419, #33562, #41029 ) ) ;
#41390 = CARTESIAN_POINT ( 'NONE',  ( 776.2046728542105711, -332.1908817542433781, -304.8212110874238761 ) ) ;
#41391 = CARTESIAN_POINT ( 'NONE',  ( 802.2119215644370342, -198.0090635724255606, 367.5423716828165084 ) ) ;
#41392 = CARTESIAN_POINT ( 'NONE',  ( 774.6312213355099630, -311.3618753856922581, -364.6798772138717482 ) ) ;
#41393 = CARTESIAN_POINT ( 'NONE',  ( 779.9999999999992042, 16.45630643248849267, 370.0000000000000568 ) ) ;
#41394 = CARTESIAN_POINT ( 'NONE',  ( 773.4516893846965786, -187.6454272087892434, -315.8398074228977066 ) ) ;
#41395 = ADVANCED_FACE ( 'NONE', ( #3898 ), #44451, .F. ) ;
#41396 = CARTESIAN_POINT ( 'NONE',  ( 749.2812353651451076, -54.45278447660219001, 323.2262854647983090 ) ) ;
#41397 = CARTESIAN_POINT ( 'NONE',  ( 808.7373736539768743, -452.9681489794446065, 336.0792598452978268 ) ) ;
#41398 = CARTESIAN_POINT ( 'NONE',  ( 811.0346526505617248, -374.6346026584193396, -323.0537975583478101 ) ) ;
#41399 = CARTESIAN_POINT ( 'NONE',  ( 919.9999999999993179, 219.9999999999998863, 360.0000000000000000 ) ) ;
#41400 = CARTESIAN_POINT ( 'NONE',  ( 771.3260364891663130, -307.6454272087888171, 306.0683387631859773 ) ) ;
#41401 = CARTESIAN_POINT ( 'NONE',  ( 879.9999999999992042, 239.9999999999998010, -360.0000000000000000 ) ) ;
#41402 = CARTESIAN_POINT ( 'NONE',  ( 813.1304606946830518, -305.9073299311467622, 352.3570229623690580 ) ) ;
#41403 = CARTESIAN_POINT ( 'NONE',  ( 782.4968714119720516, -10.81642084023869543, -305.0891759886411023 ) ) ;
#41404 = CARTESIAN_POINT ( 'NONE',  ( 756.3353852180819104, -245.9073299311469896, -331.1735550268788302 ) ) ;
#41405 = CARTESIAN_POINT ( 'NONE',  ( 265.7583438952258916, -600.0000000000000000, -320.0000000000000000 ) ) ;
#41406 = CARTESIAN_POINT ( 'NONE',  ( 803.6646147819161570, -401.9073299311463643, 348.8264449731210561 ) ) ;
#41407 = CARTESIAN_POINT ( 'NONE',  ( 800.9840315886518738, -172.9181544815165239, 354.1144889064786412 ) ) ;
#41408 = CARTESIAN_POINT ( 'NONE',  ( 804.1601925771018387, -55.44195992623293989, -346.5483106153029098 ) ) ;
#41409 = CARTESIAN_POINT ( 'NONE',  ( 808.7758568127978833, -52.16923265350567362, 320.0363995740631822 ) ) ;
#41410 = CARTESIAN_POINT ( 'NONE',  ( 801.9419747391806368, -378.4527844766011526, 351.9812246680014027 ) ) ;
#41411 = DIRECTION ( 'NONE',  ( 1.000000000000000000, 0.000000000000000000, -0.000000000000000000 ) ) ;
#41412 = CARTESIAN_POINT ( 'NONE',  ( 745.1769319972822814, -137.8055962898690154, 346.2694204179732083 ) ) ;
#41413 = CARTESIAN_POINT ( 'NONE',  ( 785.3687786644884454, -443.3618753856917465, 315.3201227861279676 ) ) ;
#41414 = ORIENTED_EDGE ( 'NONE', *, *, #33769, .T. ) ;
#41415 = CARTESIAN_POINT ( 'NONE',  ( 754.8072714833581358, -76.81642084023845030, -338.1981804954720587 ) ) ;
#41416 = CARTESIAN_POINT ( 'NONE',  ( 803.8651313633788504, -365.2601417444137155, -332.4468031744301015 ) ) ;
#41418 = CARTESIAN_POINT ( 'NONE',  ( 768.0187753319979720, -176.6346026584199933, 318.0580252608186242 ) ) ;
#41417 = CARTESIAN_POINT ( 'NONE',  ( 792.1044303154645831, -204.4527844766016926, 317.8323909638837677 ) ) ;
#41419 = CARTESIAN_POINT ( 'NONE',  ( 786.2056067578752163, -371.8055962898682765, -374.4686193811670023 ) ) ;
#41420 = DIRECTION ( 'NONE',  ( -1.000000000000000000, 0.000000000000000000, 0.000000000000000000 ) ) ;
#41421 = EDGE_LOOP ( 'NONE', ( #4667, #37742, #11992, #31249, #7686, #3312, #27003, #24353, #13932, #8555, #41089 ) ) ;
#41422 = CARTESIAN_POINT ( 'NONE',  ( 797.8594530101008786, -397.5436935675100472, 322.1405469898980982 ) ) ;
#41423 = EDGE_LOOP ( 'NONE', ( #6542, #44521, #26307, #23276 ) ) ;
#41424 = SHAPE_REPRESENTATION_RELATIONSHIP ( 'NONE' , 'NONE' ,  #10941, #27670 ) ;
#41425 = CARTESIAN_POINT ( 'NONE',  ( 792.2312462859673587, -227.9073299311471033, -307.2067596250082602 ) ) ;
#41426 = CARTESIAN_POINT ( 'NONE',  ( 744.7301800767020268, -100.8164208402383935, 337.4774526936615189 ) ) ;
#41427 = ORIENTED_EDGE ( 'NONE', *, *, #41642, .T. ) ;
#41428 = CARTESIAN_POINT ( 'NONE',  ( 764.8639956371174549, -200.0891481129653471, -319.7806653035542581 ) ) ;
#41429 = VERTEX_POINT ( 'NONE', #11061 ) ;
#41430 = CARTESIAN_POINT ( 'NONE',  ( 802.1676090361156639, -326.6346026584193396, -327.8955696845344505 ) ) ;
#41431 = CARTESIAN_POINT ( 'NONE',  ( 755.3028492785439312, -447.2817908451521021, -335.9200461376539693 ) ) ;
#41432 = CARTESIAN_POINT ( 'NONE',  ( 784.0799538623451781, -203.8055962898688449, 364.6971507214555572 ) ) ;
#41434 = DIRECTION ( 'NONE',  ( 0.000000000000000000, 0.000000000000000000, 1.000000000000000000 ) ) ;
#41433 = CARTESIAN_POINT ( 'NONE',  ( 779.9999999999992042, -452.9681489794448339, -339.9999999999999432 ) ) ;
#41435 = CARTESIAN_POINT ( 'NONE',  ( 779.9999999999992042, -452.9681489794448339, 339.9999999999999432 ) ) ;
#41436 = ORIENTED_EDGE ( 'NONE', *, *, #31148, .T. ) ;
#41437 = CARTESIAN_POINT ( 'NONE',  ( 792.1044303154645831, 11.54721552339760038, -317.8323909638837677 ) ) ;
#41438 = DIRECTION ( 'NONE',  ( 0.000000000000000000, 1.000000000000000000, -0.000000000000000000 ) ) ;
#41439 = LINE ( 'NONE', #43862, #3455 ) ;
#41440 = ORIENTED_EDGE ( 'NONE', *, *, #2909, .T. ) ;
#41441 = CARTESIAN_POINT ( 'NONE',  ( 744.6391490659812007, -254.7363362996981095, -338.7502325331110455 ) ) ;
#41442 = CARTESIAN_POINT ( 'NONE',  ( 778.7629533639073998, -104.7363362996985785, 375.0009284576466371 ) ) ;
#41444 = CARTESIAN_POINT ( 'NONE',  ( 755.0636971347428243, -220.2709662947834772, -341.7834795799807353 ) ) ;
#41443 = DIRECTION ( 'NONE',  ( 0.000000000000000000, 0.000000000000000000, -1.000000000000000000 ) ) ;
#41445 = CARTESIAN_POINT ( 'NONE',  ( 755.8398074228967971, -379.4419599262318457, -333.4516893846970333 ) ) ;
#41446 = CARTESIAN_POINT ( 'NONE',  ( 783.7953271457878373, -248.1908817542435202, -375.1787889125761239 ) ) ;
#41447 = LINE ( 'NONE', #25924, #21584 ) ;
#41448 = DIRECTION ( 'NONE',  ( 1.644774851296528363E-16, -1.000000000000000000, 0.000000000000000000 ) ) ;
#41449 = CARTESIAN_POINT ( 'NONE',  ( 755.1538015810308480, -86.19088175424408860, -343.0433043558613804 ) ) ;
#41450 = CARTESIAN_POINT ( 'NONE',  ( 757.4527132478984868, -448.3726999360611103, 329.1273215169538844 ) ) ;
#41451 = CARTESIAN_POINT ( 'NONE',  ( 802.2119215644370342, -366.0090635724250774, 367.5423716828165084 ) ) ;
#41452 = CARTESIAN_POINT ( 'NONE',  ( 755.8398074228967971, -427.4419599262317888, -333.4516893846970333 ) ) ;
#41453 = CARTESIAN_POINT ( 'NONE',  ( 767.7687537140311633, -287.9073299311468759, -372.7932403749916830 ) ) ;
#41454 = CARTESIAN_POINT ( 'NONE',  ( 911.9999999999993179, 219.9999999999998863, 350.0000000000000000 ) ) ;
#41455 = CARTESIAN_POINT ( 'NONE',  ( -208.8365100919714052, 260.0000000000001137, -199.9999999999926956 ) ) ;
#41456 = CARTESIAN_POINT ( 'NONE',  ( 797.8594530101008786, -61.54369356751124087, -322.1405469898980982 ) ) ;
#41457 = CARTESIAN_POINT ( 'NONE',  ( 760.0363995740630116, -226.9181544815163534, 368.7758568127991907 ) ) ;
#41458 = CARTESIAN_POINT ( 'NONE',  ( 749.8865473780648472, -164.5328690171416781, -322.1177392798429082 ) ) ;
#41459 = CARTESIAN_POINT ( 'NONE',  ( 813.1304606946830518, -185.9073299311472454, 352.3570229623690580 ) ) ;
#41460 = CARTESIAN_POINT ( 'NONE',  ( 751.6929314249748586, -414.9982390220555430, -318.8095938919659034 ) ) ;
#41461 = DIRECTION ( 'NONE',  ( 1.000000000000000000, -0.000000000000000000, -0.000000000000000000 ) ) ;
#41462 = CARTESIAN_POINT ( 'NONE',  ( 757.8323909638827445, -290.6346026584195101, 352.1044303154654358 ) ) ;
#41463 = CARTESIAN_POINT ( 'NONE',  ( 766.9102291470427417, -42.55451811788057626, 318.6633372737382501 ) ) ;
#41464 = CARTESIAN_POINT ( 'NONE',  ( 767.8955696845333705, -432.4527844766008684, -362.1676090361162323 ) ) ;
#41465 = FACE_BOUND ( 'NONE', #25048, .T. ) ;
#41466 = FACE_OUTER_BOUND ( 'NONE', #42721, .T. ) ;
#41468 = CARTESIAN_POINT ( 'NONE',  ( 767.8955696845333705, -336.4527844766012095, 362.1676090361162323 ) ) ;
#41467 = CARTESIAN_POINT ( 'NONE',  ( 764.0069404352550464, -111.0783235625964096, 359.2566176426627180 ) ) ;
#41469 = VERTEX_POINT ( 'NONE', #21446 ) ;
#41470 = CARTESIAN_POINT ( 'NONE',  ( 769.1273215169530886, -262.7146871989594956, -317.4527132478988847 ) ) ;
#41471 = CARTESIAN_POINT ( 'NONE',  ( 762.1405469898971887, -121.5436935675110419, -357.8594530101015607 ) ) ;
#41472 = CARTESIAN_POINT ( 'NONE',  ( 804.6798772138708955, -111.7255117493293000, 334.6312213355107019 ) ) ;
#41473 = AXIS2_PLACEMENT_3D ( 'NONE', #33830, #44222, #16052 ) ;
#41474 = CARTESIAN_POINT ( 'NONE',  ( 801.9858362298568863, -267.0783235625958696, -312.7379699480935642 ) ) ;
#41475 = CARTESIAN_POINT ( 'NONE',  ( 51.16348990802859475, 240.0000000000000568, -197.2499999999946851 ) ) ;
#41476 = CARTESIAN_POINT ( 'NONE',  ( 805.9055244015594326, -387.6237781080499758, 315.8990559732753240 ) ) ;
#41477 = ORIENTED_EDGE ( 'NONE', *, *, #693, .F. ) ;
#41478 = CARTESIAN_POINT ( 'NONE',  ( 768.0187753319979720, -272.6346026584196807, 318.0580252608186242 ) ) ;
#41479 = CARTESIAN_POINT ( 'NONE',  ( 789.9200121543843807, -49.98741447168749374, -317.0176451133914384 ) ) ;
#41480 = CARTESIAN_POINT ( 'NONE',  ( 797.8594530101008786, -157.5436935675108998, -322.1405469898980982 ) ) ;
#41481 = CARTESIAN_POINT ( 'NONE',  ( 755.3201227861273992, -363.7255117493284047, 345.3687786644892981 ) ) ;
#41482 = CARTESIAN_POINT ( 'NONE',  ( 805.0032342141412300, -109.5436935675110988, -314.9967657858571783 ) ) ;
#41483 = CARTESIAN_POINT ( 'NONE',  ( 800.0135310231082713, -110.0891481129656597, -325.0180583372163028 ) ) ;
#41484 = ORIENTED_EDGE ( 'NONE', *, *, #6577, .T. ) ;
#41485 = CARTESIAN_POINT ( 'NONE',  ( 761.4292242960306112, -41.46360902697149697, -323.2154366446414429 ) ) ;
#41486 = CARTESIAN_POINT ( 'NONE',  ( 805.2837595273609850, -338.7363362996978822, -340.5290396650784714 ) ) ;
#41488 = CARTESIAN_POINT ( 'NONE',  ( 755.1538015810308480, -422.1908817542430370, 343.0433043558613804 ) ) ;
#41487 = CARTESIAN_POINT ( 'NONE',  ( 788.8264449731200330, -117.1800572038746964, 363.6646147819171233 ) ) ;
#41491 = CARTESIAN_POINT ( 'NONE',  ( 807.5423716828161105, -345.0783235625956991, 362.2119215644372048 ) ) ;
#41490 = PLANE ( 'NONE',  #18859 ) ;
#41489 = DIRECTION ( 'NONE',  ( -1.000000000000000000, -0.000000000000000000, 0.000000000000000000 ) ) ;
#41492 = CARTESIAN_POINT ( 'NONE',  ( 793.4146539503750546, -121.9874144716872593, 307.6481478633938877 ) ) ;
#41493 = CARTESIAN_POINT ( 'NONE',  ( 763.0428371773158460, -347.4636090269705733, -358.7617431975195359 ) ) ;
#41494 = CARTESIAN_POINT ( 'NONE',  ( 768.0187753319979720, -344.6346026584195101, -318.0580252608186242 ) ) ;
#41495 = AXIS2_PLACEMENT_3D ( 'NONE', #2235, #41504, #6158 ) ;
#41496 = CARTESIAN_POINT ( 'NONE',  ( 793.5525998758768083, -127.0999726633348672, -372.6845335610516941 ) ) ;
#41497 = EDGE_CURVE ( 'NONE', #12114, #29177, #28366, .T. ) ;
#41498 = CARTESIAN_POINT ( 'NONE',  ( 762.1177392798416577, 5.445481882119263872, 309.8865473780659272 ) ) ;
#41500 = LINE ( 'NONE', #45192, #41741 ) ;
#41499 = FACE_OUTER_BOUND ( 'NONE', #21094, .T. ) ;
#41501 = CARTESIAN_POINT ( 'NONE',  ( 760.5453621957607311, -261.0783235625959264, -323.8424801807151425 ) ) ;
#41502 = CARTESIAN_POINT ( 'NONE',  ( 799.9636004259356241, -166.9181544815165523, -311.2241431872006956 ) ) ;
#41503 = DIRECTION ( 'NONE',  ( 1.892425610156518354E-16, 1.000000000000000000, -0.000000000000000000 ) ) ;
#41504 = DIRECTION ( 'NONE',  ( -1.880165489482579047E-16, -1.000000000000000000, -0.000000000000000000 ) ) ;
#41505 = CARTESIAN_POINT ( 'NONE',  ( 755.8894580844503253, -327.8272453906069472, 332.3691319403863531 ) ) ;
#41506 = ORIENTED_EDGE ( 'NONE', *, *, #15427, .T. ) ;
#41507 = CARTESIAN_POINT ( 'NONE',  ( 810.4231160770870019, -312.5545181178797520, 321.9338519418446936 ) ) ;
#41508 = PRESENTATION_LAYER_ASSIGNMENT (  '', '', ( #9778 ) ) ;
#41509 = CARTESIAN_POINT ( 'NONE',  ( 815.2698199232962679, -184.8164208402381234, -342.5225473063383674 ) ) ;
#41510 = LINE ( 'NONE', #23931, #3240 ) ;
#41511 = CARTESIAN_POINT ( 'NONE',  ( 776.2046728542105711, -116.1908817542440033, 304.8212110874238761 ) ) ;
#41512 = CARTESIAN_POINT ( 'NONE',  ( 747.2067596250078623, -315.1800572038740711, -352.2312462859687230 ) ) ;
#41513 = DIRECTION ( 'NONE',  ( 0.000000000000000000, 0.000000000000000000, 1.000000000000000000 ) ) ;
#41514 = LINE ( 'NONE', #38743, #13881 ) ;
#41515 = CARTESIAN_POINT ( 'NONE',  ( 765.0180583372156207, -168.9982390220563673, 360.0135310231089534 ) ) ;
#41516 = ORIENTED_EDGE ( 'NONE', *, *, #17132, .T. ) ;
#41517 = CARTESIAN_POINT ( 'NONE',  ( 809.0717654672305343, -436.9181544815157281, 360.1688906516309885 ) ) ;
#41518 = CARTESIAN_POINT ( 'NONE',  ( 815.1787889125755555, -366.8965053807773984, -343.7953271457877804 ) ) ;
#41519 = CARTESIAN_POINT ( 'NONE',  ( 805.0032342141412300, -133.5436935675110135, -314.9967657858571783 ) ) ;
#41520 = CARTESIAN_POINT ( 'NONE',  ( 755.5913626894240451, -37.64542720878968396, 346.6156483768012890 ) ) ;
#41521 = CARTESIAN_POINT ( 'NONE',  ( 792.2312462859673587, -395.9073299311465348, -307.2067596250082602 ) ) ;
#41522 = FACE_BOUND ( 'NONE', #45356, .T. ) ;
#41523 = CARTESIAN_POINT ( 'NONE',  ( 765.8855110935204493, -430.1692326535043094, 319.0159684113471599 ) ) ;
#41524 = ORIENTED_EDGE ( 'NONE', *, *, #39356, .T. ) ;
#41525 = CARTESIAN_POINT ( 'NONE',  ( 793.4146539503750546, -145.9874144716871740, -307.6481478633938877 ) ) ;
#41526 = CARTESIAN_POINT ( 'NONE',  ( 999.5857864376259840, 479.9999999999999432, 199.9999999999999432 ) ) ;
#41527 = CARTESIAN_POINT ( 'NONE',  ( 745.1769319972822814, -281.8055962898686175, 346.2694204179732083 ) ) ;
#41528 = CARTESIAN_POINT ( 'NONE',  ( 757.8323909638828582, -98.63460265842023489, 352.1044303154654358 ) ) ;
#41529 = AXIS2_PLACEMENT_3D ( 'NONE', #26131, #29608, #26580 ) ;
#41530 = EDGE_LOOP ( 'NONE', ( #19584, #42050, #26645, #23727, #9410, #28068, #14054, #25339, #17274, #19490, #20120 ) ) ;
#41531 = CARTESIAN_POINT ( 'NONE',  ( 801.9419747391806368, -282.4527844766014937, 351.9812246680014027 ) ) ;
#41532 = CARTESIAN_POINT ( 'NONE',  ( 782.5225473063381969, 1.729033705215812011, -375.2698199232970637 ) ) ;
#41533 = CARTESIAN_POINT ( 'NONE',  ( 799.9999999999993179, -512.9681489794448908, 339.9999999999999432 ) ) ;
#41534 = ADVANCED_FACE ( 'NONE', ( #42918, #14765 ), #28838, .F. ) ;
#41535 = ORIENTED_EDGE ( 'NONE', *, *, #18705, .T. ) ;
#41536 = ORIENTED_EDGE ( 'NONE', *, *, #7420, .F. ) ;
#41537 = CARTESIAN_POINT ( 'NONE',  ( 773.7305795820266212, -417.2817908451522158, -374.8230680027170365 ) ) ;
#41538 = EDGE_CURVE ( 'NONE', #2952, #40312, #11284, .T. ) ;
#41540 = CARTESIAN_POINT ( 'NONE',  ( 807.5423716828161105, -249.0783235625959549, 362.2119215644372048 ) ) ;
#41539 = CARTESIAN_POINT ( 'NONE',  ( 814.9108240113580450, -352.2709662947830225, 337.5031285880265273 ) ) ;
#41541 = CARTESIAN_POINT ( 'NONE',  ( 786.5483106153019435, -271.6454272087889876, -364.1601925771022366 ) ) ;
#41542 = CARTESIAN_POINT ( 'NONE',  ( 774.6312213355099630, -263.3618753856924855, -364.6798772138717482 ) ) ;
#41543 = CARTESIAN_POINT ( 'NONE',  ( 756.3353852180820240, -413.9073299311465348, -331.1735550268787733 ) ) ;
#41544 = CARTESIAN_POINT ( 'NONE',  ( 805.1927285166397041, -88.81642084023842187, -341.8018195045277707 ) ) ;
#41545 = CARTESIAN_POINT ( 'NONE',  ( 755.0636971347428243, -244.2709662947834204, 341.7834795799807353 ) ) ;
#41546 = ORIENTED_EDGE ( 'NONE', *, *, #29496, .F. ) ;
#41547 = CARTESIAN_POINT ( 'NONE',  ( 811.0346526505616112, -350.6346026584192828, 323.0537975583477532 ) ) ;
#41548 = DIRECTION ( 'NONE',  ( 0.000000000000000000, 0.000000000000000000, 1.000000000000000000 ) ) ;
#41549 = CARTESIAN_POINT ( 'NONE',  ( 773.7305795820266212, -33.28179084515333130, -374.8230680027170365 ) ) ;
#41550 = CARTESIAN_POINT ( 'NONE',  ( 791.7419236033215384, 16.45630643248850689, 314.5156751397937001 ) ) ;
#41551 = DIRECTION ( 'NONE',  ( -1.000000000000000000, 0.000000000000000000, 0.000000000000000000 ) ) ;
#41552 = CARTESIAN_POINT ( 'NONE',  ( 800.9840315886518738, -220.9181544815164102, 354.1144889064786412 ) ) ;
#41553 = CARTESIAN_POINT ( 'NONE',  ( 767.8955696845333705, -120.4527844766019484, 362.1676090361162323 ) ) ;
#41554 = VERTEX_POINT ( 'NONE', #10362 ) ;
#41555 = CARTESIAN_POINT ( 'NONE',  ( 802.9823548866075953, -25.09997266333519050, -330.0799878456151077 ) ) ;
#41556 = CARTESIAN_POINT ( 'NONE',  ( 744.7301800767020268, -52.81642084023856398, -337.4774526936615189 ) ) ;
#41557 = VECTOR ( 'NONE', #23302, 1000.000000000000000 ) ;
#41558 = CARTESIAN_POINT ( 'NONE',  ( 759.2295555964440155, -280.1692326535049347, 353.9708237608231229 ) ) ;
#41559 = CARTESIAN_POINT ( 'NONE',  ( 774.6858677611749044, -441.7255117493282910, -315.5713283507209894 ) ) ;
#41560 = CARTESIAN_POINT ( 'NONE',  ( 759.9864689768902508, -50.08914811296584446, -354.9819416627836404 ) ) ;
#41561 = CARTESIAN_POINT ( 'NONE',  ( 809.0717654672305343, -4.918154481517067467, 360.1688906516309885 ) ) ;
#41562 = CARTESIAN_POINT ( 'NONE',  ( 763.2262854647970016, -200.6346026584199365, -309.2812353651462445 ) ) ;
#41563 = CARTESIAN_POINT ( 'NONE',  ( 777.5031285880264704, -70.81642084023850714, 374.9108240113588408 ) ) ;
#41564 = EDGE_CURVE ( 'NONE', #861, #29887, #31831, .T. ) ;
#41565 = CARTESIAN_POINT ( 'NONE',  ( 772.4837098697144029, -167.3618753856927412, 374.5518280994205611 ) ) ;
#41566 = CARTESIAN_POINT ( 'NONE',  ( 831.1634899080286232, 259.9999999999998863, -197.2500000000000853 ) ) ;
#41567 = CARTESIAN_POINT ( 'NONE',  ( 919.9999999999993179, 219.9999999999998863, -360.0000000000000000 ) ) ;
#41568 = CARTESIAN_POINT ( 'NONE',  ( 778.7502325331095108, -264.3510508353232353, -304.6391490659818828 ) ) ;
#41569 =( GEOMETRIC_REPRESENTATION_CONTEXT ( 3 ) GLOBAL_UNCERTAINTY_ASSIGNED_CONTEXT ( ( #6702 ) ) GLOBAL_UNIT_ASSIGNED_CONTEXT ( ( #15190, #853, #21878 ) ) REPRESENTATION_CONTEXT ( 'NONE', 'WORKASPACE' ) );
#41570 = CARTESIAN_POINT ( 'NONE',  ( 744.6391490659812007, -422.7363362996975980, 338.7502325331110455 ) ) ;
#41571 = CARTESIAN_POINT ( 'NONE',  ( 814.2001403089898304, -281.3618753856923718, -347.4397851343538264 ) ) ;
#41572 = LINE ( 'NONE', #17312, #20586 ) ;
#41573 = CARTESIAN_POINT ( 'NONE',  ( 747.2067596250078623, -411.1800572038738437, 352.2312462859687230 ) ) ;
#41574 = CARTESIAN_POINT ( 'NONE',  ( 787.4397851343537695, -21.72551174932956641, 374.2001403089903988 ) ) ;
#41575 = CARTESIAN_POINT ( 'NONE',  ( 785.3141322388236176, -357.7255117493285184, -364.4286716492789537 ) ) ;
#41576 = CARTESIAN_POINT ( 'NONE',  ( 796.7845633553578182, -33.62377810805116951, 358.5707757039688204 ) ) ;
#41577 = CARTESIAN_POINT ( 'NONE',  ( 781.2497674668890113, -36.35105083532390324, -375.3608509340180603 ) ) ;
#41578 = CARTESIAN_POINT ( 'NONE',  ( 772.3691319403857278, -143.2601417444144829, -315.8894580844506663 ) ) ;
#41579 = CARTESIAN_POINT ( 'NONE',  ( 744.9990715423526808, -162.3510508353235196, 341.2370466360926002 ) ) ;
#41580 = LINE ( 'NONE', #16879, #32860 ) ;
#41581 = ORIENTED_EDGE ( 'NONE', *, *, #3591, .F. ) ;
#41582 = CARTESIAN_POINT ( 'NONE',  ( 759.9864689768902508, -50.08914811296584446, -354.9819416627836404 ) ) ;
#41583 = CARTESIAN_POINT ( 'NONE',  ( 794.1144889064781864, -178.1692326535052473, -360.9840315886528401 ) ) ;
#41584 = CARTESIAN_POINT ( 'NONE',  ( 758.0580252608178853, -174.4527844766018063, 328.0187753319985404 ) ) ;
#41585 = EDGE_CURVE ( 'NONE', #4358, #14962, #7836, .T. ) ;
#41586 = CARTESIAN_POINT ( 'NONE',  ( 764.3348316497523456, 1.285312801039623753, -308.6759233522265617 ) ) ;
#41587 = CARTESIAN_POINT ( 'NONE',  ( 803.6646147819162707, -281.9073299311469327, 348.8264449731211130 ) ) ;
#41588 = VECTOR ( 'NONE', #38735, 1000.000000000000000 ) ;
#41589 = FACE_OUTER_BOUND ( 'NONE', #25996, .T. ) ;
#41590 = CIRCLE ( 'NONE', #43075, 6.118999999999985562 ) ;
#41591 = ORIENTED_EDGE ( 'NONE', *, *, #3268, .F. ) ;
#41592 = CARTESIAN_POINT ( 'NONE',  ( 760.5453621957607311, -21.07832356259667250, 323.8424801807151425 ) ) ;
#41593 = CARTESIAN_POINT ( 'NONE',  ( 749.5768839229115201, -300.5545181178797520, -358.0661480581553064 ) ) ;
#41594 = ADVANCED_FACE ( 'NONE', ( #4364 ), #24438, .F. ) ;
#41595 = CARTESIAN_POINT ( 'NONE',  ( 745.7998596910086917, -269.3618753856924286, 332.5602148656461168 ) ) ;
#41596 = CARTESIAN_POINT ( 'NONE',  ( 779.4763451958990572, -320.7363362996979390, 365.0264073115438919 ) ) ;
#41597 = CARTESIAN_POINT ( 'NONE',  ( 789.6640940660590786, -442.9180389616178672, 363.1300863558843162 ) ) ;
#41598 = CARTESIAN_POINT ( 'NONE',  ( 804.8461984189677878, -146.1908817542438896, -336.9566956441385628 ) ) ;
#41599 = CARTESIAN_POINT ( 'NONE',  ( 767.8955696845333705, -96.45278447660203369, -362.1676090361162323 ) ) ;
#41600 = CARTESIAN_POINT ( 'NONE',  ( 801.9419747391806368, -306.4527844766013800, -351.9812246680014027 ) ) ;
#41601 = ORIENTED_EDGE ( 'NONE', *, *, #44984, .T. ) ;
#41602 = CIRCLE ( 'NONE', #9123, 9.999999999999980460 ) ;
#41603 = CARTESIAN_POINT ( 'NONE',  ( 786.6156483768007774, -313.4419599262320730, 315.5913626894246136 ) ) ;
#41604 = CARTESIAN_POINT ( 'NONE',  ( 791.7608162188021197, 205.0000000000000568, -329.9999999999999432 ) ) ;
#41605 = CARTESIAN_POINT ( 'NONE',  ( 775.8780910478218402, -105.2817908451530968, 364.9511171171680530 ) ) ;
#41606 = CARTESIAN_POINT ( 'NONE',  ( 757.8323909638827445, -2.634602658420536869, 352.1044303154654358 ) ) ;
#41607 = EDGE_LOOP ( 'NONE', ( #36258, #9343 ) ) ;
#41608 = CARTESIAN_POINT ( 'NONE',  ( 807.2620300519052989, -384.0090635724249637, -318.0141637701419768 ) ) ;
#41609 = DIRECTION ( 'NONE',  ( -1.000000000000000000, 0.000000000000000000, 0.000000000000000000 ) ) ;
#41610 = EDGE_CURVE ( 'NONE', #637, #16382, #9039, .T. ) ;
#41611 = CARTESIAN_POINT ( 'NONE',  ( 815.3608509340175488, -242.7363362996980811, 341.2497674668889545 ) ) ;
#41612 = CARTESIAN_POINT ( 'NONE',  ( 771.2633955100217236, -335.9073299311468190, -363.4237431249939618 ) ) ;
#41613 = EDGE_CURVE ( 'NONE', #43251, #39517, #4580, .T. ) ;
#41614 = CARTESIAN_POINT ( 'NONE',  ( 787.4999999999992042, -512.9681489794448908, -370.0000000000000000 ) ) ;
#41615 = CARTESIAN_POINT ( 'NONE',  ( 766.9102291470427417, -186.5545181178801215, -318.6633372737382501 ) ) ;
#41616 = CARTESIAN_POINT ( 'NONE',  ( 813.1304606946830518, -89.90732993114750116, 352.3570229623690580 ) ) ;
#41617 =( GEOMETRIC_REPRESENTATION_CONTEXT ( 3 ) GLOBAL_UNCERTAINTY_ASSIGNED_CONTEXT ( ( #30104 ) ) GLOBAL_UNIT_ASSIGNED_CONTEXT ( ( #24309, #2850, #6312 ) ) REPRESENTATION_CONTEXT ( 'NONE', 'WORKASPACE' ) );
#41618 = CARTESIAN_POINT ( 'NONE',  ( 809.2691622578233819, -452.9681489794448908, 335.3267997378328005 ) ) ;
#41619 = CARTESIAN_POINT ( 'NONE',  ( 751.6929314249750860, -390.9982390220556567, -318.8095938919659034 ) ) ;
#41620 = DIRECTION ( 'NONE',  ( 0.000000000000000000, 0.000000000000000000, -1.000000000000000000 ) ) ;
#41621 = CARTESIAN_POINT ( 'NONE',  ( 814.2805881961230625, -313.6454272087888171, 331.2368401574024119 ) ) ;
#41622 = CARTESIAN_POINT ( 'NONE',  ( 784.4999999999993179, -512.9681489794448908, -339.9999999999999432 ) ) ;
#41623 = CARTESIAN_POINT ( 'NONE',  ( 811.0346526505616112, -278.6346026584196807, 323.0537975583477532 ) ) ;
#41624 = CARTESIAN_POINT ( 'NONE',  ( 787.4397851343537695, -21.72551174932956641, -374.2001403089903988 ) ) ;
#41625 = CARTESIAN_POINT ( 'NONE',  ( 804.6798772138708955, -231.7255117493288310, -334.6312213355107019 ) ) ;
#41626 = DIRECTION ( 'NONE',  ( -0.000000000000000000, 1.000000000000000000, -0.000000000000000000 ) ) ;
#41627 = CARTESIAN_POINT ( 'NONE',  ( 778.2165204200184689, -406.8164208402375266, 364.9363028652563230 ) ) ;
#41628 = CARTESIAN_POINT ( 'NONE',  ( 793.0897708529556667, -150.5545181178802352, 361.3366627262616362 ) ) ;
#41629 = CARTESIAN_POINT ( 'NONE',  ( 778.7629533639073998, -32.73633629969879877, -375.0009284576466371 ) ) ;
#41630 = CARTESIAN_POINT ( 'NONE',  ( 803.2186876482843445, -55.98741447168748664, -350.0220218866286928 ) ) ;
#41631 = CARTESIAN_POINT ( 'NONE',  ( 798.0661480581538854, -74.53286901714196233, 309.5768839229118043 ) ) ;
#41632 = CARTESIAN_POINT ( 'NONE',  ( 800.2193346964446619, -378.9982390220557136, 355.1360043628816925 ) ) ;
#41633 = DIRECTION ( 'NONE',  ( 0.000000000000000000, 0.000000000000000000, 1.000000000000000000 ) ) ;
#41634 = AXIS2_PLACEMENT_3D ( 'NONE', #30440, #2263, #40846 ) ;
#41635 = EDGE_CURVE ( 'NONE', #2904, #11665, #930, .T. ) ;
#41636 =( NAMED_UNIT ( * ) PLANE_ANGLE_UNIT ( ) SI_UNIT ( $, .RADIAN. ) );
#41637 = CARTESIAN_POINT ( 'NONE',  ( 752.4576283171824116, -141.0783235625962959, 317.7880784355627952 ) ) ;
#41638 = CARTESIAN_POINT ( 'NONE',  ( 781.7834795799800531, -418.8164208402374129, 315.0636971347436202 ) ) ;
#41639 = ORIENTED_EDGE ( 'NONE', *, *, #4887, .T. ) ;
#41640 = CARTESIAN_POINT ( 'NONE',  ( 774.6312213355099630, -47.36187538569312494, -364.6798772138717482 ) ) ;
#41641 = CIRCLE ( 'NONE', #18767, 10.00000000000000888 ) ;
#41642 = EDGE_CURVE ( 'NONE', #10343, #22935, #11522, .T. ) ;
#41643 = CARTESIAN_POINT ( 'NONE',  ( 787.6308680596127942, -371.2601417444136587, -364.1105419155492768 ) ) ;
#41645 = CARTESIAN_POINT ( 'NONE',  ( 774.6858677611749044, -177.7255117493290868, 315.5713283507209894 ) ) ;
#41644 = CARTESIAN_POINT ( 'NONE',  ( 800.2193346964447755, -186.9982390220563104, 355.1360043628815788 ) ) ;
#41646 = ORIENTED_EDGE ( 'NONE', *, *, #33669, .T. ) ;
#41647 = CARTESIAN_POINT ( 'NONE',  ( 776.2433038121456548, -348.8965053807774552, -374.8207195650711014 ) ) ;
#41648 = CARTESIAN_POINT ( 'NONE',  ( 767.9999999999992042, 178.9475563372491251, 320.0000000000000000 ) ) ;
#41649 = ORIENTED_EDGE ( 'NONE', *, *, #36318, .F. ) ;
#41650 = CARTESIAN_POINT ( 'NONE',  ( 774.6312213355099630, -407.3618753856920307, 364.6798772138717482 ) ) ;
#41651 = EDGE_LOOP ( 'NONE', ( #27728, #14847, #34203, #7932, #28062 ) ) ;
#41652 =( NAMED_UNIT ( * ) SI_UNIT ( $, .STERADIAN. ) SOLID_ANGLE_UNIT ( ) );
#41653 = ADVANCED_FACE ( 'NONE', ( #22128 ), #1766, .F. ) ;
#41654 = CARTESIAN_POINT ( 'NONE',  ( 777.5031285880264704, -214.8164208402380666, -374.9108240113588408 ) ) ;
#41655 = CARTESIAN_POINT ( 'NONE',  ( 796.7737145352015204, -140.6346026584201070, 370.7187646348536987 ) ) ;
#41656 = VECTOR ( 'NONE', #44637, 1000.000000000000000 ) ;
#41657 = ORIENTED_EDGE ( 'NONE', *, *, #28639, .F. ) ;
#41658 = CARTESIAN_POINT ( 'NONE',  ( 800.0135310231082713, -206.0891481129653471, -325.0180583372163028 ) ) ;
#41659 = VECTOR ( 'NONE', #12480, 1000.000000000000000 ) ;
#41660 = EDGE_LOOP ( 'NONE', ( #41440, #32408, #20527, #4234 ) ) ;
#41661 = CARTESIAN_POINT ( 'NONE',  ( 768.0187753319979720, -320.6346026584195670, -318.0580252608186242 ) ) ;
#41662 = CARTESIAN_POINT ( 'NONE',  ( 797.6776695296629214, -19.54369356751139364, -357.6776695296636603 ) ) ;
#41663 = AXIS2_PLACEMENT_3D ( 'NONE', #43268, #39359, #7489 ) ;
#41664 = CARTESIAN_POINT ( 'NONE',  ( 761.2382568024794409, -207.6237781080506295, 356.9571628226838129 ) ) ;
#41665 = CARTESIAN_POINT ( 'NONE',  ( 799.9999999999993179, 205.0000000000000568, 319.9999999999999432 ) ) ;
#41666 = DIRECTION ( 'NONE',  ( 0.000000000000000000, 0.000000000000000000, 1.000000000000000000 ) ) ;
#41667 = EDGE_LOOP ( 'NONE', ( #42678, #22538 ) ) ;
#41668 = CARTESIAN_POINT ( 'NONE',  ( 804.4286716492782716, 6.638124614306706306, -345.3141322388244703 ) ) ;
#41669 = CARTESIAN_POINT ( 'NONE',  ( 200.7583438952258916, 294.6698570112193920, -224.9999999999999716 ) ) ;
#41670 = FACE_OUTER_BOUND ( 'NONE', #30326, .T. ) ;
#41671 = ORIENTED_EDGE ( 'NONE', *, *, #23841, .F. ) ;
#41672 = CARTESIAN_POINT ( 'NONE',  ( 802.2119215644370342, -246.0090635724253900, -367.5423716828165084 ) ) ;
#41673 = CARTESIAN_POINT ( 'NONE',  ( 760.0363995740630116, -130.9181544815166660, 368.7758568127991907 ) ) ;
#41674 = AXIS2_PLACEMENT_3D ( 'NONE', #33230, #12210, #5947 ) ;
#41676 = CARTESIAN_POINT ( 'NONE',  ( 774.6858677611749044, -225.7255117493289163, -315.5713283507209894 ) ) ;
#41675 = CARTESIAN_POINT ( 'NONE',  ( 949.5497976682736407, 120.6654763175833693, -2132.806278688367456 ) ) ;
#41677 = CARTESIAN_POINT ( 'NONE',  ( 798.7617431975189675, -387.6237781080499758, -323.0428371773161871 ) ) ;
#41678 = EDGE_CURVE ( 'NONE', #56, #5612, #14960, .T. ) ;
#41679 = LINE ( 'NONE', #13499, #45166 ) ;
#41680 = DIRECTION ( 'NONE',  ( 5.551115123125783688E-16, -1.000000000000000000, 0.000000000000000000 ) ) ;
#41681 = CARTESIAN_POINT ( 'NONE',  ( 755.3028492785439312, -87.28179084515316788, -335.9200461376539693 ) ) ;
#41682 = VECTOR ( 'NONE', #33848, 1000.000000000000000 ) ;
#41683 = AXIS2_PLACEMENT_3D ( 'NONE', #16114, #30199, #35832 ) ;
#41684 = CARTESIAN_POINT ( 'NONE',  ( 783.7953271457878373, -368.1908817542433212, 375.1787889125761239 ) ) ;
#41685 = CARTESIAN_POINT ( 'NONE',  ( -769.9999999999992042, 205.0000000000000568, -360.0000000000000000 ) ) ;
#41686 = CARTESIAN_POINT ( 'NONE',  ( 759.8311093483677041, 25.83076734649409545, -310.9282345327691814 ) ) ;
#41687 = CARTESIAN_POINT ( 'NONE',  ( 745.0891759886404770, -268.2709662947833067, -342.4968714119734159 ) ) ;
#41688 = CARTESIAN_POINT ( 'NONE',  ( 803.4237431249931660, 8.819942796124882634, 331.2633955100225194 ) ) ;
#41689 = CARTESIAN_POINT ( 'NONE',  ( 764.8639956371174549, -80.08914811296574499, -319.7806653035542013 ) ) ;
#41690 = CARTESIAN_POINT ( 'NONE',  ( 745.7194118038753459, -229.6454272087890729, 348.7631598425976449 ) ) ;
#41691 = CARTESIAN_POINT ( 'NONE',  ( 812.6845335610512393, -175.9874144716871172, -353.5525998758768651 ) ) ;
#41692 = CARTESIAN_POINT ( 'NONE',  ( 800.9747183278959710, -204.9982390220562820, 311.9810565676471583 ) ) ;
#41693 = CARTESIAN_POINT ( 'NONE',  ( 782.4968714119720516, -418.8164208402374129, -305.0891759886411023 ) ) ;
#41694 = DIRECTION ( 'NONE',  ( -0.000000000000000000, 1.110223024625155554E-15, 1.000000000000000000 ) ) ;
#41695 = AXIS2_PLACEMENT_3D ( 'NONE', #3746, #31901, #42083 ) ;
#41696 = CARTESIAN_POINT ( 'NONE',  ( 794.9819416627830151, -276.9982390220559978, 319.9864689768909898 ) ) ;
#41697 = AXIS2_PLACEMENT_3D ( 'NONE', #30723, #32545, #215 ) ;
#41698 = CARTESIAN_POINT ( 'NONE',  ( 793.0897708529556667, -54.55451811788054783, 361.3366627262616362 ) ) ;
#41699 = CARTESIAN_POINT ( 'NONE',  ( 802.1676090361156639, -422.6346026584192259, -327.8955696845344505 ) ) ;
#41700 = VECTOR ( 'NONE', #44816, 1000.000000000000000 ) ;
#41701 = FACE_OUTER_BOUND ( 'NONE', #3940, .T. ) ;
#41702 = EDGE_CURVE ( 'NONE', #10586, #32983, #24526, .T. ) ;
#41703 = CARTESIAN_POINT ( 'NONE',  ( 799.9999999999993179, -512.9681489794448908, -339.9999999999999432 ) ) ;
#41705 = CARTESIAN_POINT ( 'NONE',  ( 765.0180583372156207, -312.9982390220559409, 360.0135310231089534 ) ) ;
#41704 = CARTESIAN_POINT ( 'NONE',  ( 776.9566956441375396, -108.8965053807782084, 364.8461984189686405 ) ) ;
#41706 = EDGE_LOOP ( 'NONE', ( #24490, #22050, #17418, #42120 ) ) ;
#41707 = CARTESIAN_POINT ( 'NONE',  ( 765.8855110935204493, -262.1692326535049347, -319.0159684113471599 ) ) ;
#41708 = CARTESIAN_POINT ( 'NONE',  ( 801.9419747391806368, -90.45278447660209054, 351.9812246680014027 ) ) ;
#41709 = CARTESIAN_POINT ( 'NONE',  ( 746.7653713866222915, -257.2601417444141134, -351.0478386215610271 ) ) ;
#41710 = LINE ( 'NONE', #3601, #40091 ) ;
#41711 = CARTESIAN_POINT ( 'NONE',  ( 776.2433038121456548, -372.8965053807773415, 374.8207195650711014 ) ) ;
#41712 = ORIENTED_EDGE ( 'NONE', *, *, #45233, .T. ) ;
#41713 = CARTESIAN_POINT ( 'NONE',  ( 801.9419747391806368, -282.4527844766014937, 351.9812246680014027 ) ) ;
#41714 = CARTESIAN_POINT ( 'NONE',  ( 773.3843516231979720, -37.44195992623299674, -364.4086373105754433 ) ) ;
#41715 = CARTESIAN_POINT ( 'NONE',  ( 781.7834795799800531, -178.8164208402381519, -315.0636971347436202 ) ) ;
#41716 = CARTESIAN_POINT ( 'NONE',  ( 785.3141322388236176, -405.7255117493283478, 364.4286716492789537 ) ) ;
#41717 = EDGE_CURVE ( 'NONE', #30556, #10806, #25606, .T. ) ;
#41718 = VECTOR ( 'NONE', #13923, 1000.000000000000000 ) ;
#41719 = CARTESIAN_POINT ( 'NONE',  ( 751.9810565676468741, -122.0891481129656171, -360.9747183278973921 ) ) ;
#41720 = CARTESIAN_POINT ( 'NONE',  ( 758.0580252608178853, -102.4527844766020337, -328.0187753319985404 ) ) ;
#41721 = ORIENTED_EDGE ( 'NONE', *, *, #7796, .T. ) ;
#41722 = CARTESIAN_POINT ( 'NONE',  ( 757.0176451133909268, -37.09997266333514432, -349.9200121543848354 ) ) ;
#41723 = CARTESIAN_POINT ( 'NONE',  ( 759.0159684113467620, -352.9181544815159555, -325.8855110935213020 ) ) ;
#41725 = CARTESIAN_POINT ( 'NONE',  ( 773.4516893846965786, -451.6454272087884192, 315.8398074228977066 ) ) ;
#41724 = CARTESIAN_POINT ( 'NONE',  ( 785.3687786644884454, -131.3618753856928834, 315.3201227861279676 ) ) ;
#41726 = CARTESIAN_POINT ( 'NONE',  ( 803.8651313633788504, -101.2601417444146250, 332.4468031744301015 ) ) ;
#41729 = CARTESIAN_POINT ( 'NONE',  ( 786.2056067578752163, -371.8055962898682765, 374.4686193811670023 ) ) ;
#41728 = DIRECTION ( 'NONE',  ( 0.000000000000000000, 0.000000000000000000, 1.000000000000000000 ) ) ;
#41727 = FACE_OUTER_BOUND ( 'NONE', #41706, .T. ) ;
#41730 = CARTESIAN_POINT ( 'NONE',  ( 763.8424801807145741, -354.0090635724250774, -320.5453621957614700 ) ) ;
#41731 = CARTESIAN_POINT ( 'NONE',  ( 785.3687786644884454, -347.3618753856922012, -315.3201227861279676 ) ) ;
#41732 = CARTESIAN_POINT ( 'NONE',  ( 783.7953271457878373, -128.1908817542439465, -375.1787889125761239 ) ) ;
#41733 = CARTESIAN_POINT ( 'NONE',  ( 793.5525998758768083, -7.099972663335241130, 372.6845335610516941 ) ) ;
#41734 = VECTOR ( 'NONE', #11000, 1000.000000000000000 ) ;
#41736 = DIRECTION ( 'NONE',  ( 0.000000000000000000, 0.000000000000000000, 1.000000000000000000 ) ) ;
#41735 = CARTESIAN_POINT ( 'NONE',  ( 879.9999999999992042, 249.9999999999998295, 360.0000000000000000 ) ) ;
#41737 = CARTESIAN_POINT ( 'NONE',  ( 758.6633372737375112, -308.5328690171412518, -326.9102291470432533 ) ) ;
#41738 = CARTESIAN_POINT ( 'NONE',  ( 750.9282345327678740, -136.9181544815166376, -319.8311093483690115 ) ) ;
#41739 = CYLINDRICAL_SURFACE ( 'NONE', #17873, 2.749999999999863665 ) ;
#41740 = CARTESIAN_POINT ( 'NONE',  ( 831.1634899080286232, 259.9999999999998863, -208.0249999999998920 ) ) ;
#41741 = VECTOR ( 'NONE', #31774, 1000.000000000000000 ) ;
#41742 = CARTESIAN_POINT ( 'NONE',  ( 760.7433823573367135, -348.0090635724251342, 355.9930595647440441 ) ) ;
#41743 = CARTESIAN_POINT ( 'NONE',  ( 814.8207195650702488, -314.1908817542433781, 336.2433038121456548 ) ) ;
#41744 = CARTESIAN_POINT ( 'NONE',  ( 801.1904061080338124, -164.0891481129654892, -368.3070685750236066 ) ) ;
#41745 = CARTESIAN_POINT ( 'NONE',  ( 767.9999999999992042, 205.0000000000000568, 339.9999999999999432 ) ) ;
#41746 = VECTOR ( 'NONE', #12544, 1000.000000000000000 ) ;
#41747 = CARTESIAN_POINT ( 'NONE',  ( 783.7953271457878373, -104.1908817542440175, 375.1787889125761239 ) ) ;
#41748 = CARTESIAN_POINT ( 'NONE',  ( 772.4837098697144029, -287.3618753856923718, -374.5518280994205611 ) ) ;
#41749 = CIRCLE ( 'NONE', #26993, 9.999999999999982236 ) ;
#41750 = DIRECTION ( 'NONE',  ( -1.000000000000000000, 0.000000000000000000, 0.000000000000000000 ) ) ;
#41751 = PRODUCT_DEFINITION_SHAPE ( 'NONE', 'NONE',  #33777 ) ;
#41752 = CARTESIAN_POINT ( 'NONE',  ( 180.7583438952259201, 394.6698570112193920, -244.9999999999999716 ) ) ;
#41753 = CARTESIAN_POINT ( 'NONE',  ( 788.8264449731200330, -189.1800572038744122, 363.6646147819171233 ) ) ;
#41754 = AXIS2_PLACEMENT_3D ( 'NONE', #9863, #23935, #45203 ) ;
#41755 = ORIENTED_EDGE ( 'NONE', *, *, #16194, .F. ) ;
#41756 = CARTESIAN_POINT ( 'NONE',  ( 747.6481478633932056, -421.0999726633340288, 353.4146539503763620 ) ) ;
#41757 = CARTESIAN_POINT ( 'NONE',  ( 781.2497674668890113, -372.3510508353228374, -375.3608509340180603 ) ) ;
#41758 = CARTESIAN_POINT ( 'NONE',  ( 815.2698199232961542, -136.8164208402382371, -342.5225473063383106 ) ) ;
#41759 = CARTESIAN_POINT ( 'NONE',  ( 787.5531968255692163, -45.82724539060783542, 316.1348686366205811 ) ) ;
#41760 = CARTESIAN_POINT ( 'NONE',  ( 804.7487373415286811, -379.5436935675102745, -364.7487373415288516 ) ) ;
#41761 = CARTESIAN_POINT ( 'NONE',  ( 799.9999999999993179, -462.9681489794448339, 362.3606797749978909 ) ) ;
#41762 = CARTESIAN_POINT ( 'NONE',  ( 744.9990715423526808, 5.648949164675971524, 341.2370466360926002 ) ) ;
#41763 = ORIENTED_EDGE ( 'NONE', *, *, #15648, .F. ) ;
#41764 = CARTESIAN_POINT ( 'NONE',  ( 805.9055244015594326, -147.6237781080508285, -315.8990559732753240 ) ) ;
#41765 = CYLINDRICAL_SURFACE ( 'NONE', #9849, 7.999999999999896083 ) ;
#41766 = CARTESIAN_POINT ( 'NONE',  ( 747.3154664389472828, -259.9874144716869182, 326.4474001241230781 ) ) ;
#41767 = CARTESIAN_POINT ( 'NONE',  ( 755.5713283507202505, -125.3618753856928834, 334.6858677611754729 ) ) ;
#41768 = ORIENTED_EDGE ( 'NONE', *, *, #1284, .F. ) ;
#41769 = AXIS2_PLACEMENT_3D ( 'NONE', #5868, #29893, #16260 ) ;
#41770 = VECTOR ( 'NONE', #1228, 1000.000000000000000 ) ;
#41771 = CARTESIAN_POINT ( 'NONE',  ( 757.8323909638827445, -290.6346026584195101, 352.1044303154654358 ) ) ;
#41772 = CARTESIAN_POINT ( 'NONE',  ( 787.4397851343537695, 2.274488250670355871, -374.2001403089903988 ) ) ;
#41773 = CYLINDRICAL_SURFACE ( 'NONE', #28335, 10.00000000000000888 ) ;
#41774 = ORIENTED_EDGE ( 'NONE', *, *, #45346, .F. ) ;
#41775 = ORIENTED_EDGE ( 'NONE', *, *, #20676, .T. ) ;
#41776 = CONICAL_SURFACE ( 'NONE', #43966, 8.024999999999948841, 0.7853981633963380560 ) ;
#41777 = CARTESIAN_POINT ( 'NONE',  ( 765.0180583372156207, -24.99823902205683268, 360.0135310231089534 ) ) ;
#41778 = CARTESIAN_POINT ( 'NONE',  ( 800.2193346964447755, -258.9982390220561115, -355.1360043628815788 ) ) ;
#41779 = AXIS2_PLACEMENT_3D ( 'NONE', #27005, #40639, #41102 ) ;
#41781 = CARTESIAN_POINT ( 'NONE',  ( 805.9055244015594326, -243.6237781080504590, 315.8990559732753240 ) ) ;
#41780 = CARTESIAN_POINT ( 'NONE',  ( 808.0189434323515343, -374.0891481129647786, 319.0252816721025511 ) ) ;
#41782 = CARTESIAN_POINT ( 'NONE',  ( 800.9840315886518738, -268.9181544815162397, -354.1144889064786412 ) ) ;
#41783 = CARTESIAN_POINT ( 'NONE',  ( 771.2633955100217236, -239.9073299311470748, -363.4237431249939618 ) ) ;
#41784 = CARTESIAN_POINT ( 'NONE',  ( 791.9812246680005501, -404.6346026584193396, -361.9419747391813189 ) ) ;
#41785 = CARTESIAN_POINT ( 'NONE',  ( 774.6858677611749044, -81.72551174932937101, -315.5713283507209894 ) ) ;
#41786 = CARTESIAN_POINT ( 'NONE',  ( 803.4237431249931660, -231.1800572038743553, 331.2633955100225194 ) ) ;
#41787 = ORIENTED_EDGE ( 'NONE', *, *, #30289, .T. ) ;
#41788 = CARTESIAN_POINT ( 'NONE',  ( 749.2812353651451076, -342.4527844766013231, 323.2262854647983090 ) ) ;
#41789 = DIRECTION ( 'NONE',  ( -1.000000000000000000, 0.000000000000000000, 0.000000000000000000 ) ) ;
#41790 = CARTESIAN_POINT ( 'NONE',  ( 766.4474001241216001, -43.09997266333511590, -307.3154664389482491 ) ) ;
#41791 = CARTESIAN_POINT ( 'NONE',  ( 799.9999999999993179, 166.4563064324884465, 319.9999999999999432 ) ) ;
#41792 = CARTESIAN_POINT ( 'NONE',  ( 919.9999999999993179, 154.9999999999998863, 360.0000000000000000 ) ) ;
#41793 = CARTESIAN_POINT ( 'NONE',  ( 801.5560724626406000, -216.5545181178800931, 326.7756240680316182 ) ) ;
#41794 = CARTESIAN_POINT ( 'NONE',  ( 771.2633955100217236, -119.9073299311474443, 363.4237431249939618 ) ) ;
#41795 = ORIENTED_EDGE ( 'NONE', *, *, #32094, .T. ) ;
#41796 = CARTESIAN_POINT ( 'NONE',  ( 804.4086373105744769, -1.645427208789804308, -333.3843516231986541 ) ) ;
#41797 = CARTESIAN_POINT ( 'NONE',  ( 812.7932403749906598, -87.18005720387481006, -327.7687537140311633 ) ) ;
#41798 = CARTESIAN_POINT ( 'NONE',  ( 803.2186876482843445, -295.9874144716866908, 350.0220218866286928 ) ) ;
#41799 = AXIS2_PLACEMENT_3D ( 'NONE', #39816, #36320, #15754 ) ;
#41800 = CARTESIAN_POINT ( 'NONE',  ( 768.0187753319979720, -440.6346026584191122, -318.0580252608186242 ) ) ;
#41801 = CARTESIAN_POINT ( 'NONE',  ( 757.8323909638828582, -50.63460265842038410, -352.1044303154654358 ) ) ;
#41802 = CARTESIAN_POINT ( 'NONE',  ( 814.2001403089898304, -449.3618753856918602, 347.4397851343538264 ) ) ;
#41803 = CARTESIAN_POINT ( 'NONE',  ( 759.0252816721024374, -192.9982390220562820, -368.0189434323527280 ) ) ;
#41804 = CARTESIAN_POINT ( 'NONE',  ( 777.4774526936600978, -178.2709662947835625, 304.7301800767027657 ) ) ;
#41805 = CARTESIAN_POINT ( 'NONE',  ( 803.6646147819161570, -89.90732993114750116, 348.8264449731210561 ) ) ;
#41806 = VECTOR ( 'NONE', #5927, 1000.000000000000000 ) ;
#41807 = LINE ( 'NONE', #30473, #35054 ) ;
#41808 = DIRECTION ( 'NONE',  ( 0.000000000000000000, 0.000000000000000000, -1.000000000000000000 ) ) ;
#41809 = CARTESIAN_POINT ( 'NONE',  ( 815.0009284576459549, -270.3510508353231216, -338.7629533639073429 ) ) ;
#41810 = AXIS2_PLACEMENT_3D ( 'NONE', #14345, #249, #18039 ) ;
#41811 = CARTESIAN_POINT ( 'NONE',  ( 762.1177392798416577, -402.5545181178795247, 309.8865473780659272 ) ) ;
#41812 = CARTESIAN_POINT ( 'NONE',  ( 805.0032342141412300, -277.5436935675105019, -314.9967657858571783 ) ) ;
#41813 = CARTESIAN_POINT ( 'NONE',  ( 989.9999999999992042, 239.9999999999998863, 350.0000000000000000 ) ) ;
#41814 = CARTESIAN_POINT ( 'NONE',  ( 814.2001403089898304, -401.3618753856920307, 347.4397851343538264 ) ) ;
#41815 = CARTESIAN_POINT ( 'NONE',  ( 746.8695393053151292, -5.907329931147799584, 327.6429770376306578 ) ) ;
#41816 = CARTESIAN_POINT ( 'NONE',  ( 797.6776695296629214, -379.5436935675102745, -357.6776695296636603 ) ) ;
#41817 = AXIS2_PLACEMENT_3D ( 'NONE', #17712, #17015, #42179 ) ;
#41818 = CARTESIAN_POINT ( 'NONE',  ( 801.3366627262608972, -32.53286901714208312, 353.0897708529566899 ) ) ;
#41819 = CARTESIAN_POINT ( 'NONE',  ( 751.2241431872005251, -64.16923265350563099, -359.9636004259367610 ) ) ;
#41820 = CARTESIAN_POINT ( 'NONE',  ( 770.0799878456142551, -181.9874144716870887, -362.9823548866085616 ) ) ;
#41821 = CARTESIAN_POINT ( 'NONE',  ( 803.8556311672234642, -153.6237781080508000, 365.6418435158340117 ) ) ;
#41822 = CARTESIAN_POINT ( 'NONE',  ( 765.0180583372156207, -0.9982390220569063999, 360.0135310231089534 ) ) ;
#41823 = ORIENTED_EDGE ( 'NONE', *, *, #40181, .T. ) ;
#41824 = CARTESIAN_POINT ( 'NONE',  ( 778.2165204200184689, -46.81642084023858530, -364.9363028652563230 ) ) ;
#41825 = CARTESIAN_POINT ( 'NONE',  ( 803.2186876482843445, -199.9874144716870603, -350.0220218866286928 ) ) ;
#41826 = CARTESIAN_POINT ( 'NONE',  ( 764.8639956371174549, -152.0891481129655460, 319.7806653035542013 ) ) ;
#41827 = CARTESIAN_POINT ( 'NONE',  ( 756.1443688327750579, 2.376221891948710585, -314.3581564841659315 ) ) ;
#41828 = CARTESIAN_POINT ( 'NONE',  ( 758.0580252608178853, -294.4527844766013800, 328.0187753319985404 ) ) ;
#41829 = DIRECTION ( 'NONE',  ( 1.000000000000000000, 0.000000000000000000, 0.000000000000000000 ) ) ;
#41830 = ORIENTED_EDGE ( 'NONE', *, *, #16234, .F. ) ;
#41831 = CARTESIAN_POINT ( 'NONE',  ( 793.2243759319678702, -26.53286901714210799, 318.4439275373583200 ) ) ;
#41832 = CARTESIAN_POINT ( 'NONE',  ( 755.8990559732751535, -299.4636090269707438, -365.9055244015606831 ) ) ;
#41833 = AXIS2_PLACEMENT_3D ( 'NONE', #25817, #32760, #8505 ) ;
#41834 = CARTESIAN_POINT ( 'NONE',  ( 763.2262854647970016, -248.6346026584197659, 309.2812353651462445 ) ) ;
#41835 = CARTESIAN_POINT ( 'NONE',  ( 783.0745993439762742, -344.1908817542433212, 365.1016975059196739 ) ) ;
#41836 = CARTESIAN_POINT ( 'NONE',  ( 805.9055244015594326, 20.37622189194865285, 315.8990559732753240 ) ) ;
#41837 = EDGE_CURVE ( 'NONE', #18319, #40061, #30404, .T. ) ;
#41838 = CARTESIAN_POINT ( 'NONE',  ( 761.4292242960306112, -137.4636090269711985, -323.2154366446414429 ) ) ;
#41839 = CARTESIAN_POINT ( 'NONE',  ( 803.6646147819161570, -137.9073299311473875, -348.8264449731210561 ) ) ;
#41840 = CARTESIAN_POINT ( 'NONE',  ( 792.1044303154646968, -300.4527844766013231, -317.8323909638837677 ) ) ;
#41841 = ORIENTED_EDGE ( 'NONE', *, *, #32811, .F. ) ;
#41842 = CARTESIAN_POINT ( 'NONE',  ( 796.7845633553578182, -321.6237781080502600, 358.5707757039688204 ) ) ;
#41843 = DIRECTION ( 'NONE',  ( -0.000000000000000000, 1.000000000000000000, -0.000000000000000000 ) ) ;
#41844 = AXIS2_PLACEMENT_3D ( 'NONE', #15154, #1048, #10772 ) ;
#41845 = CARTESIAN_POINT ( 'NONE',  ( 790.9844846989617508, -118.3726999360621619, 317.2208543904092721 ) ) ;
#41846 = CARTESIAN_POINT ( 'NONE',  ( 778.2165204200184689, 1.183579159761269040, 364.9363028652563230 ) ) ;
#41847 = ORIENTED_EDGE ( 'NONE', *, *, #11703, .T. ) ;
#41848 = CARTESIAN_POINT ( 'NONE',  ( 745.5313806188320314, -375.2817908451523294, -333.7943932421247268 ) ) ;
#41849 = CARTESIAN_POINT ( 'NONE',  ( 786.4999999999993179, -110.5936016518799221, 750.6326042729449455 ) ) ;
#41850 = CARTESIAN_POINT ( 'NONE',  ( 807.2620300519052989, -240.0090635724253900, 318.0141637701419768 ) ) ;
#41851 = CARTESIAN_POINT ( 'NONE',  ( 801.3366627262608972, -200.5328690171415644, 353.0897708529566899 ) ) ;
#41852 = CARTESIAN_POINT ( 'NONE',  ( 757.8323909638827445, -314.6346026584194533, -352.1044303154654358 ) ) ;
#41853 = CARTESIAN_POINT ( 'NONE',  ( 799.9999999999993179, 166.4563064324884465, 319.9999999999999432 ) ) ;
#41854 = CARTESIAN_POINT ( 'NONE',  ( 755.3028492785439312, -207.2817908451527842, -335.9200461376539693 ) ) ;
#41855 = EDGE_CURVE ( 'NONE', #32983, #12347, #22574, .T. ) ;
#41856 = CARTESIAN_POINT ( 'NONE',  ( 763.2262854647970016, -80.63460265842029173, 309.2812353651462445 ) ) ;
#41857 = CARTESIAN_POINT ( 'NONE',  ( 806.8957046614239061, -452.9681489794451181, 342.6393539086462852 ) ) ;
#41858 = CARTESIAN_POINT ( 'NONE',  ( 814.5518280994195948, -423.7255117493282341, -332.4837098697145166 ) ) ;
#41859 = DIRECTION ( 'NONE',  ( 1.000000000000000000, -0.000000000000000000, -0.000000000000000000 ) ) ;
#41860 = CARTESIAN_POINT ( 'NONE',  ( 810.4231160770870019, -360.5545181178796383, 321.9338519418446936 ) ) ;
#41861 = CARTESIAN_POINT ( 'NONE',  ( 786.4999999999993179, -512.9681489794448908, -329.9999999999999432 ) ) ;
#41862 = CARTESIAN_POINT ( 'NONE',  ( 751.9810565676468741, -290.0891481129650629, 360.9747183278973921 ) ) ;
#41863 = CARTESIAN_POINT ( 'NONE',  ( 812.7932403749906598, -63.18005720387488822, -327.7687537140311633 ) ) ;
#41864 = ADVANCED_FACE ( 'NONE', ( #1108 ), #1553, .F. ) ;
#41865 = CARTESIAN_POINT ( 'NONE',  ( 759.7806653035534055, -270.9982390220561115, -324.8639956371180801 ) ) ;
#41866 = CYLINDRICAL_SURFACE ( 'NONE', #7041, 6.118999999999985562 ) ;
#41867 = CARTESIAN_POINT ( 'NONE',  ( 759.7806653035534055, -390.9982390220557136, 324.8639956371180801 ) ) ;
#41868 = CARTESIAN_POINT ( 'NONE',  ( 780.5236548040995785, -164.7363362996983938, 314.9735926884559944 ) ) ;
#41869 = CARTESIAN_POINT ( 'NONE',  ( 795.8262568251477660, -22.37269993606246743, -308.3538107759623585 ) ) ;
#41870 = CARTESIAN_POINT ( 'NONE',  ( 773.3843516231979720, -37.44195992623299674, -364.4086373105754433 ) ) ;
#41871 = CARTESIAN_POINT ( 'NONE',  ( 744.9990715423526808, -66.35105083532378956, 341.2370466360926002 ) ) ;
#41872 = CARTESIAN_POINT ( 'NONE',  ( 771.1735550268780344, -417.1800572038736732, 316.3353852180828198 ) ) ;
#41873 = AXIS2_PLACEMENT_3D ( 'NONE', #28759, #25513, #14682 ) ;
#41874 = CARTESIAN_POINT ( 'NONE',  ( 311.1634899080286232, 240.0000000000000000, -197.2499999999964473 ) ) ;
#41875 = CARTESIAN_POINT ( 'NONE',  ( 800.0135310231082713, -422.0891481129647218, 325.0180583372163028 ) ) ;
#41876 = ORIENTED_EDGE ( 'NONE', *, *, #3160, .T. ) ;
#41877 = CARTESIAN_POINT ( 'NONE',  ( 781.7834795799800531, -58.81642084023854267, -315.0636971347436202 ) ) ;
#41878 = CARTESIAN_POINT ( 'NONE',  ( 756.1348686366196716, -353.2601417444137724, -347.5531968255698416 ) ) ;
#41880 = CARTESIAN_POINT ( 'NONE',  ( 755.3201227861273992, -195.7255117493290015, 345.3687786644892981 ) ) ;
#41879 = CARTESIAN_POINT ( 'NONE',  ( 758.0580252608178853, -222.4527844766016642, 328.0187753319985404 ) ) ;
#41881 = CARTESIAN_POINT ( 'NONE',  ( 814.8230680027162407, -389.8055962898682765, -333.7305795820267917 ) ) ;
#41882 = LINE ( 'NONE', #13704, #16818 ) ;
#41883 = VERTEX_POINT ( 'NONE', #11751 ) ;
#41884 = CARTESIAN_POINT ( 'NONE',  ( 767.8955696845333705, -384.4527844766011526, 362.1676090361162323 ) ) ;
#41885 = EDGE_CURVE ( 'NONE', #15194, #45131, #39716, .T. ) ;
#41886 = EDGE_LOOP ( 'NONE', ( #11108, #41061, #30017, #24245 ) ) ;
#41887 = CARTESIAN_POINT ( 'NONE',  ( 772.4837098697144029, -215.3618753856925423, -374.5518280994205611 ) ) ;
#41888 = CARTESIAN_POINT ( 'NONE',  ( 814.9108240113580450, -136.2709662947837330, 337.5031285880265273 ) ) ;
#41889 = VERTEX_POINT ( 'NONE', #36896 ) ;
#41890 = CARTESIAN_POINT ( 'NONE',  ( 771.2633955100217236, -215.9073299311471317, -363.4237431249939618 ) ) ;
#41891 = EDGE_LOOP ( 'NONE', ( #3077, #35630 ) ) ;
#41892 = CARTESIAN_POINT ( 'NONE',  ( 804.9363028652555840, -352.2709662947830225, -338.2165204200192079 ) ) ;
#41893 = CARTESIAN_POINT ( 'NONE',  ( 785.3141322388236176, -21.72551174932956641, -364.4286716492789537 ) ) ;
#41894 = CARTESIAN_POINT ( 'NONE',  ( 805.1016975059191054, -246.8965053807777679, 343.0745993439771837 ) ) ;
#41895 = CYLINDRICAL_SURFACE ( 'NONE', #29945, 19.99999999999998934 ) ;
#41896 = CARTESIAN_POINT ( 'NONE',  ( -769.9999999999992042, 205.0000000000000568, -360.0000000000000000 ) ) ;
#41897 = VERTEX_POINT ( 'NONE', #29965 ) ;
#41898 = CARTESIAN_POINT ( 'NONE',  ( 774.6312213355099630, 0.6381246143067236254, -364.6798772138717482 ) ) ;
#41899 = CARTESIAN_POINT ( 'NONE',  ( 791.4804426738954817, -453.0432664090020580, -367.7164109511201673 ) ) ;
#41900 = CARTESIAN_POINT ( 'NONE',  ( -28.63011601220122415, -365.3551492539851893, -18.13243251470705886 ) ) ;
#41901 = ORIENTED_EDGE ( 'NONE', *, *, #2759, .F. ) ;
#41902 = CARTESIAN_POINT ( 'NONE',  ( 814.2805881961230625, -289.6454272087889308, -331.2368401574024119 ) ) ;
#41903 = CARTESIAN_POINT ( 'NONE',  ( 745.1792804349281596, -134.1908817542439181, 343.7566961878542884 ) ) ;
#41904 = AXIS2_PLACEMENT_3D ( 'NONE', #23613, #6762, #2846 ) ;
#41906 = CARTESIAN_POINT ( 'NONE',  ( 781.8018195045266339, -214.2709662947834488, -365.1927285166406705 ) ) ;
#41905 = DIRECTION ( 'NONE',  ( -1.000000000000000000, 0.000000000000000000, -0.000000000000000000 ) ) ;
#41907 = EDGE_CURVE ( 'NONE', #26595, #12779, #15651, .T. ) ;
#41908 = CARTESIAN_POINT ( 'NONE',  ( 805.1016975059191054, -390.8965053807772279, -343.0745993439771837 ) ) ;
#41909 = CARTESIAN_POINT ( 'NONE',  ( 779.9999999999992042, 126.4563064324884465, -339.9999999999999432 ) ) ;
#41910 = CARTESIAN_POINT ( 'NONE',  ( 802.1676090361155502, 9.365397341579424051, -327.8955696845344505 ) ) ;
#41911 = CARTESIAN_POINT ( 'NONE',  ( 763.0428371773158460, -107.4636090269713122, -358.7617431975195359 ) ) ;
#41912 = EDGE_CURVE ( 'NONE', #27925, #13298, #15445, .T. ) ;
#41913 = CARTESIAN_POINT ( 'NONE',  ( 812.3518521366052028, -385.0999726633340856, 326.5853460496235243 ) ) ;
#41914 = CARTESIAN_POINT ( 'NONE',  ( -769.9999999999992042, 240.0000000000000853, -360.0000000000000000 ) ) ;
#41915 = CARTESIAN_POINT ( 'NONE',  ( 773.7943932421234194, 0.1944037101305369775, -305.5313806188329409 ) ) ;
#41916 = CARTESIAN_POINT ( 'NONE',  ( 792.3570229623691148, -309.1800572038740711, -373.1304606946836770 ) ) ;
#41917 = LINE ( 'NONE', #20648, #37154 ) ;
#41918 = DIRECTION ( 'NONE',  ( 1.000000000000000000, -0.000000000000000000, -0.000000000000000000 ) ) ;
#41919 = CARTESIAN_POINT ( 'NONE',  ( 781.8018195045266339, -70.27096629478397460, -365.1927285166406705 ) ) ;
#41920 = CARTESIAN_POINT ( 'NONE',  ( 766.4474001241216001, -235.0999726633344835, 307.3154664389482491 ) ) ;
#41921 = CARTESIAN_POINT ( 'NONE',  ( 771.2368401574024119, -181.4419599262325278, -374.2805881961240857 ) ) ;
#41922 = CARTESIAN_POINT ( 'NONE',  ( 767.7687537140311633, -191.9073299311471885, 372.7932403749916830 ) ) ;
#41923 = CARTESIAN_POINT ( 'NONE',  ( 807.2620300519052989, -0.009063572426172561425, -318.0141637701419768 ) ) ;
#41924 = EDGE_CURVE ( 'NONE', #41190, #21010, #43596, .T. ) ;
#41925 = ADVANCED_FACE ( 'NONE', ( #14983 ), #44049, .F. ) ;
#41926 = DIRECTION ( 'NONE',  ( 0.000000000000000000, 0.000000000000000000, 1.000000000000000000 ) ) ;
#41927 = CARTESIAN_POINT ( 'NONE',  ( 755.3201227861273992, -291.7255117493285752, 345.3687786644892981 ) ) ;
#41928 = CARTESIAN_POINT ( 'NONE',  ( 799.2566176426618085, -48.00906357242602951, 324.0069404352559559 ) ) ;
#41929 = CARTESIAN_POINT ( 'NONE',  ( 755.0636971347428243, -436.2709662947827951, -341.7834795799807353 ) ) ;
#41930 = DIRECTION ( 'NONE',  ( 0.000000000000000000, 0.000000000000000000, 1.000000000000000000 ) ) ;
#41931 = FACE_BOUND ( 'NONE', #13827, .T. ) ;
#41933 = CARTESIAN_POINT ( 'NONE',  ( 788.7366044899766848, -323.9073299311468190, 316.5762568750059813 ) ) ;
#41932 = CARTESIAN_POINT ( 'NONE',  ( 766.7756240680305382, -134.5328690171417350, 361.5560724626415663 ) ) ;
#41934 = ORIENTED_EDGE ( 'NONE', *, *, #6964, .T. ) ;
#41935 = CARTESIAN_POINT ( 'NONE',  ( 766.7756240680305382, -254.5328690171413655, -361.5560724626415663 ) ) ;
#41936 = CARTESIAN_POINT ( 'NONE',  ( 771.2633955100217236, -95.90732993114751537, 363.4237431249939618 ) ) ;
#41937 = CARTESIAN_POINT ( 'NONE',  ( 805.9055244015594326, -243.6237781080504590, -315.8990559732753240 ) ) ;
#41938 = LINE ( 'NONE', #10504, #29758 ) ;
#41939 = CARTESIAN_POINT ( 'NONE',  ( 815.0009284576459549, -414.3510508353227237, 338.7629533639073429 ) ) ;
#41940 = EDGE_CURVE ( 'NONE', #120, #34305, #26273, .T. ) ;
#41941 = ORIENTED_EDGE ( 'NONE', *, *, #44258, .F. ) ;
#41942 = CARTESIAN_POINT ( 'NONE',  ( 788.8264449731200330, -285.1800572038740711, 363.6646147819171233 ) ) ;
#41943 = CIRCLE ( 'NONE', #36751, 7.999999999999896083 ) ;
#41944 = EDGE_CURVE ( 'NONE', #19824, #14734, #12417, .T. ) ;
#41945 = CARTESIAN_POINT ( 'NONE',  ( 784.0799538623451781, -35.80559628986934229, -364.6971507214555572 ) ) ;
#41946 = CARTESIAN_POINT ( 'NONE',  ( 797.8594530101008786, -157.5436935675108998, -322.1405469898980982 ) ) ;
#41947 = CARTESIAN_POINT ( 'NONE',  ( 797.6776695296629214, -211.5436935675107861, -357.6776695296636603 ) ) ;
#41948 = CARTESIAN_POINT ( 'NONE',  ( 800.0135310231082713, -422.0891481129647218, 325.0180583372163028 ) ) ;
#41949 = CARTESIAN_POINT ( 'NONE',  ( 746.8695393053150156, -125.9073299311474159, -327.6429770376306010 ) ) ;
#41950 = CARTESIAN_POINT ( 'NONE',  ( 803.6646147819162707, -89.90732993114752958, -348.8264449731211130 ) ) ;
#41951 = ORIENTED_EDGE ( 'NONE', *, *, #23016, .T. ) ;
#41952 = CARTESIAN_POINT ( 'NONE',  ( 801.5560724626406000, -48.55451811788057626, -326.7756240680316182 ) ) ;
#41953 = CARTESIAN_POINT ( 'NONE',  ( 801.5560724626406000, -384.5545181178795247, -326.7756240680316182 ) ) ;
#41955 = CARTESIAN_POINT ( 'NONE',  ( 775.8780910478218402, -441.2817908451521021, 364.9511171171680530 ) ) ;
#41954 = CARTESIAN_POINT ( 'NONE',  ( 804.6798772138708955, -111.7255117493293000, 334.6312213355107019 ) ) ;
#41956 = CARTESIAN_POINT ( 'NONE',  ( 787.6308680596127942, -107.2601417444145824, 364.1105419155492768 ) ) ;
#41959 = CARTESIAN_POINT ( 'NONE',  ( 815.1787889125755555, -366.8965053807773984, 343.7953271457877804 ) ) ;
#41958 = DIRECTION ( 'NONE',  ( -0.000000000000000000, 1.000000000000000000, -0.000000000000000000 ) ) ;
#41957 = DIRECTION ( 'NONE',  ( -1.000000000000000000, -0.000000000000000000, -0.000000000000000000 ) ) ;
#41960 = VERTEX_POINT ( 'NONE', #8947 ) ;
#41961 = CARTESIAN_POINT ( 'NONE',  ( 776.9254006560222479, -356.1908817542432075, -314.8983024940802125 ) ) ;
#41962 = CARTESIAN_POINT ( 'NONE',  ( 792.1044303154645831, -348.4527844766012663, -317.8323909638837677 ) ) ;
#41963 = CARTESIAN_POINT ( 'NONE',  ( 749.5768839229115201, -156.5545181178802636, -358.0661480581553064 ) ) ;
#41964 = ADVANCED_FACE ( 'NONE', ( #37110 ), #26735, .F. ) ;
#41965 = CARTESIAN_POINT ( 'NONE',  ( 749.5768839229115201, -36.55451811788061178, 358.0661480581553064 ) ) ;
#41967 = CARTESIAN_POINT ( 'NONE',  ( -454.7528517110260964, 200.0000000000001137, 350.0000000000000000 ) ) ;
#41966 = DIRECTION ( 'NONE',  ( 0.000000000000000000, 0.000000000000000000, 1.000000000000000000 ) ) ;
#41968 = EDGE_CURVE ( 'NONE', #25624, #13889, #40815, .T. ) ;
#41969 = CARTESIAN_POINT ( 'NONE',  ( 803.2186876482843445, -295.9874144716866908, -350.0220218866286928 ) ) ;
#41970 = CARTESIAN_POINT ( 'NONE',  ( 764.8639956371174549, -440.0891481129644944, -319.7806653035542013 ) ) ;
#41971 = CARTESIAN_POINT ( 'NONE',  ( 786.2694204179717872, -141.2817908451530400, -305.1769319972829067 ) ) ;
#41972 = CARTESIAN_POINT ( 'NONE',  ( -919.9999999999993179, 154.9999999999998863, -360.0000000000000000 ) ) ;
#41973 = FACE_OUTER_BOUND ( 'NONE', #9737, .T. ) ;
#41974 = CARTESIAN_POINT ( 'NONE',  ( 802.5472867521000353, -364.3726999360614514, 350.8726784830461156 ) ) ;
#41975 = EDGE_CURVE ( 'NONE', #35390, #33022, #41280, .T. ) ;
#41976 = CARTESIAN_POINT ( 'NONE',  ( 746.4236121716829757, -351.8272453906068336, 328.8385539511384650 ) ) ;
#41977 = CARTESIAN_POINT ( 'NONE',  ( 751.9810565676468741, -170.0891481129654608, -360.9747183278973921 ) ) ;
#41978 = CARTESIAN_POINT ( 'NONE',  ( 521.6730038022808458, 229.9999999999999432, -2132.806278688367456 ) ) ;
#41979 = AXIS2_PLACEMENT_3D ( 'NONE', #10908, #24976, #3519 ) ;
#41980 = CARTESIAN_POINT ( 'NONE',  ( 768.9521613784389729, -105.8272453906076578, 373.2346286133773106 ) ) ;
#41981 = CARTESIAN_POINT ( 'NONE',  ( 745.4481719005789273, -291.7255117493285752, -347.5162901302853129 ) ) ;
#41982 = DIRECTION ( 'NONE',  ( 0.000000000000000000, 0.000000000000000000, -1.000000000000000000 ) ) ;
#41983 = DIRECTION ( 'NONE',  ( 1.000000000000000000, 0.000000000000000000, 0.000000000000000000 ) ) ;
#41984 = CARTESIAN_POINT ( 'NONE',  ( 754.8072714833581358, -172.8164208402381234, 338.1981804954720587 ) ) ;
#41985 = CARTESIAN_POINT ( 'NONE',  ( 771.3260364891663130, -427.6454272087885897, 306.0683387631859773 ) ) ;
#41986 = CARTESIAN_POINT ( 'NONE',  ( 778.7502325331095108, -384.3510508353227806, -304.6391490659818828 ) ) ;
#41987 = CARTESIAN_POINT ( 'NONE',  ( 814.2001403089898304, -113.3618753856929260, -347.4397851343538264 ) ) ;
#41988 = CARTESIAN_POINT ( 'NONE',  ( 808.3070685750230950, -378.9982390220555999, -361.1904061080339261 ) ) ;
#41989 = CARTESIAN_POINT ( 'NONE',  ( 927.9999999999992042, 219.9999999999998863, 350.0000000000000000 ) ) ;
#41990 = CARTESIAN_POINT ( 'NONE',  ( 751.2241431872005251, 7.830767346494148740, 359.9636004259367610 ) ) ;
#41991 = ORIENTED_EDGE ( 'NONE', *, *, #6908, .T. ) ;
#41992 = CARTESIAN_POINT ( 'NONE',  ( 748.3538107759620743, -160.7146871989598651, -355.8262568251490165 ) ) ;
#41993 = FACE_OUTER_BOUND ( 'NONE', #44021, .T. ) ;
#41994 = CARTESIAN_POINT ( 'NONE',  ( 801.9858362298568863, -315.0783235625957559, 312.7379699480935642 ) ) ;
#41995 = CARTESIAN_POINT ( 'NONE',  ( 778.1981804954715471, -130.2709662947837614, 314.8072714833591021 ) ) ;
#41996 = ORIENTED_EDGE ( 'NONE', *, *, #23271, .F. ) ;
#41997 = CARTESIAN_POINT ( 'NONE',  ( 765.0180583372156207, -312.9982390220559409, 360.0135310231089534 ) ) ;
#41998 = CARTESIAN_POINT ( 'NONE',  ( 811.0346526505616112, -14.63460265842049424, -323.0537975583477532 ) ) ;
#41999 = CARTESIAN_POINT ( 'NONE',  ( -728.8365100919714905, 240.0000000000001990, -202.7499999999889440 ) ) ;
#42000 = ORIENTED_EDGE ( 'NONE', *, *, #11651, .T. ) ;
#42001 = CARTESIAN_POINT ( 'NONE',  ( 750.9282345327678740, -400.9181544815159555, -319.8311093483690115 ) ) ;
#42002 = AXIS2_PLACEMENT_3D ( 'NONE', #2534, #37646, #20088 ) ;
#42003 = ORIENTED_EDGE ( 'NONE', *, *, #33200, .F. ) ;
#42004 = CARTESIAN_POINT ( 'NONE',  ( 774.6312213355099630, -23.36187538569318889, 364.6798772138717482 ) ) ;
#42005 = CARTESIAN_POINT ( 'NONE',  ( 795.1360043628807261, -260.0891481129650060, -360.2193346964456282 ) ) ;
#42007 = CARTESIAN_POINT ( 'NONE',  ( 747.3154664389472828, -235.9874144716868898, 326.4474001241230781 ) ) ;
#42006 = CARTESIAN_POINT ( 'NONE',  ( 815.2698199232962679, -376.8164208402375834, 342.5225473063383674 ) ) ;
#42008 = CARTESIAN_POINT ( 'NONE',  ( 769.9779781133707957, -259.0999726633343698, -316.7813123517150871 ) ) ;
#42009 = CARTESIAN_POINT ( 'NONE',  ( 804.4286716492782716, -257.3618753856924286, -345.3141322388244703 ) ) ;
#42010 = CARTESIAN_POINT ( 'NONE',  ( 801.9419747391806368, -450.4527844766009821, -351.9812246680014027 ) ) ;
#42011 = CARTESIAN_POINT ( 'NONE',  ( 765.0180583372156207, -96.99823902205660886, -360.0135310231089534 ) ) ;
#42012 = CARTESIAN_POINT ( 'NONE',  ( 803.6646147819161570, -257.9073299311469896, 348.8264449731210561 ) ) ;
#42013 = CARTESIAN_POINT ( 'NONE',  ( 758.8095938919642549, -392.0891481129648355, 311.6929314249763365 ) ) ;
#42014 = CARTESIAN_POINT ( 'NONE',  ( 879.9999999999992042, 430.0000000000002842, -244.9999999999999716 ) ) ;
#42015 = CARTESIAN_POINT ( 'NONE',  ( 773.7305795820266212, -57.28179084515326736, -374.8230680027170365 ) ) ;
#42016 = PLANE ( 'NONE',  #10114 ) ;
#42017 = CARTESIAN_POINT ( 'NONE',  ( 707.2824899080285377, 256.4999999999999432, -199.9999999999990337 ) ) ;
#42018 = CARTESIAN_POINT ( 'NONE',  ( 784.1219089521767955, -261.2817908451526705, 315.0488828828318333 ) ) ;
#42019 = CARTESIAN_POINT ( 'NONE',  ( 754.8072714833581358, -124.8164208402383508, 338.1981804954720587 ) ) ;
#42020 = ORIENTED_EDGE ( 'NONE', *, *, #37682, .F. ) ;
#42021 = CARTESIAN_POINT ( 'NONE',  ( 804.1105419155481968, -3.827245390607979303, -347.6308680596136469 ) ) ;
#42022 = CARTESIAN_POINT ( 'NONE',  ( 772.5602148656447525, -57.72551174932945628, -305.7998596910095443 ) ) ;
#42023 = CARTESIAN_POINT ( 'NONE',  ( 759.2295555964440155, -304.1692326535048210, 353.9708237608231229 ) ) ;
#42024 = FACE_BOUND ( 'NONE', #32924, .T. ) ;
#42025 = CARTESIAN_POINT ( 'NONE',  ( 762.1177392798416577, 5.445481882119263872, 309.8865473780659272 ) ) ;
#42026 = CARTESIAN_POINT ( 'NONE',  ( 804.7487373415286811, -211.5436935675107861, -364.7487373415288516 ) ) ;
#42027 = CARTESIAN_POINT ( 'NONE',  ( 749.2812353651451076, -174.4527844766018063, 323.2262854647983090 ) ) ;
#42028 = CARTESIAN_POINT ( 'NONE',  ( 755.0636971347428243, -76.27096629478394618, 341.7834795799807353 ) ) ;
#42029 = DIRECTION ( 'NONE',  ( -0.000000000000000000, 1.000000000000000000, -0.000000000000000000 ) ) ;
#42030 = CARTESIAN_POINT ( 'NONE',  ( 793.4146539503750546, -265.9874144716867477, -307.6481478633938877 ) ) ;
#42031 = CARTESIAN_POINT ( 'NONE',  ( 764.1737431748507561, -418.3726999360612808, 371.6461892240376415 ) ) ;
#42032 = CARTESIAN_POINT ( 'NONE',  ( 745.7998596910086917, -269.3618753856924286, -332.5602148656461168 ) ) ;
#42033 = DIRECTION ( 'NONE',  ( -1.880165489482579047E-16, -1.000000000000000000, -0.000000000000000000 ) ) ;
#42034 = CARTESIAN_POINT ( 'NONE',  ( 789.9200121543843807, -361.9874144716864635, 317.0176451133914384 ) ) ;
#42035 = CARTESIAN_POINT ( 'NONE',  ( 767.6429770376291799, -33.18005720387498769, 306.8695393053162093 ) ) ;
#42036 = CARTESIAN_POINT ( 'NONE',  ( 815.1787889125755555, -30.89650538077846065, -343.7953271457877804 ) ) ;
#42037 = CARTESIAN_POINT ( 'NONE',  ( 755.3201227861273992, -387.7255117493283478, -345.3687786644892981 ) ) ;
#42038 = CARTESIAN_POINT ( 'NONE',  ( 794.1144889064781864, -10.16923265350579442, 360.9840315886528401 ) ) ;
#42039 = CARTESIAN_POINT ( 'NONE',  ( 804.6798772138708955, -207.7255117493289447, -334.6312213355107019 ) ) ;
#42040 = CARTESIAN_POINT ( 'NONE',  ( 811.6461892240364477, -52.71468719896020616, -324.1737431748509835 ) ) ;
#42041 = CARTESIAN_POINT ( 'NONE',  ( 801.3366627262608972, -200.5328690171415644, -353.0897708529566899 ) ) ;
#42042 = CARTESIAN_POINT ( 'NONE',  ( 759.8311093483677041, -214.1692326535052189, 310.9282345327691814 ) ) ;
#42043 = CARTESIAN_POINT ( 'NONE',  ( 759.7806653035535192, -6.998239022056886860, 324.8639956371181370 ) ) ;
#42044 = ORIENTED_EDGE ( 'NONE', *, *, #7550, .F. ) ;
#42045 = CARTESIAN_POINT ( 'NONE',  ( 787.6308680596127942, -203.2601417444143124, -364.1105419155492768 ) ) ;
#42046 = CARTESIAN_POINT ( 'NONE',  ( 794.9819416627830151, -204.9982390220562820, 319.9864689768909898 ) ) ;
#42047 = CARTESIAN_POINT ( 'NONE',  ( 745.1769319972822814, -17.80559628986940979, -346.2694204179732083 ) ) ;
#42048 = CARTESIAN_POINT ( 'NONE',  ( 764.8639956371174549, -320.0891481129648923, 319.7806653035542581 ) ) ;
#42049 = DIRECTION ( 'NONE',  ( 0.000000000000000000, 0.000000000000000000, 1.000000000000000000 ) ) ;
#42050 = ORIENTED_EDGE ( 'NONE', *, *, #7810, .T. ) ;
#42051 = CARTESIAN_POINT ( 'NONE',  ( 756.1348686366196716, -41.26014174441479554, 347.5531968255698416 ) ) ;
#42052 = CARTESIAN_POINT ( 'NONE',  ( 766.4474001241216001, -307.0999726633343130, -307.3154664389482491 ) ) ;
#42053 = CARTESIAN_POINT ( 'NONE',  ( 751.6929314249750860, -246.9982390220560831, 318.8095938919659034 ) ) ;
#42054 = CARTESIAN_POINT ( 'NONE',  ( 757.0176451133909268, -349.0999726633342561, 349.9200121543848354 ) ) ;
#42055 = CARTESIAN_POINT ( 'NONE',  ( 788.7631598425961101, 22.55804007376682918, 305.7194118038759143 ) ) ;
#42056 = CARTESIAN_POINT ( 'NONE',  ( 796.1575198192839480, -150.0090635724257027, -359.4546378042384163 ) ) ;
#42057 = CARTESIAN_POINT ( 'NONE',  ( 757.8323909638827445, -146.6346026584200217, -352.1044303154654358 ) ) ;
#42058 = CARTESIAN_POINT ( 'NONE',  ( 792.1044303154646968, -348.4527844766012095, -317.8323909638837677 ) ) ;
#42059 = ORIENTED_EDGE ( 'NONE', *, *, #11972, .T. ) ;
#42060 = CARTESIAN_POINT ( 'NONE',  ( 800.9747183278959710, -300.9982390220559409, 311.9810565676471583 ) ) ;
#42061 = CARTESIAN_POINT ( 'NONE',  ( 804.9511171171677688, -317.8055962898684470, 335.8780910478229202 ) ) ;
#42062 = DIRECTION ( 'NONE',  ( -0.000000000000000000, 1.000000000000000000, -0.000000000000000000 ) ) ;
#42063 = CARTESIAN_POINT ( 'NONE',  ( 801.5560724626406000, -120.5545181178803205, 326.7756240680316182 ) ) ;
#42064 = CARTESIAN_POINT ( 'NONE',  ( 759.7806653035534055, -6.998239022056885972, 324.8639956371180801 ) ) ;
#42065 = ORIENTED_EDGE ( 'NONE', *, *, #37315, .F. ) ;
#42066 = CARTESIAN_POINT ( 'NONE',  ( 744.6391490659812007, -374.7363362996978253, -338.7502325331110455 ) ) ;
#42067 = PLANE ( 'NONE',  #37240 ) ;
#42068 = CARTESIAN_POINT ( 'NONE',  ( 797.8822607201568644, -246.5545181178799510, 370.1134526219340160 ) ) ;
#42069 = CARTESIAN_POINT ( 'NONE',  ( 770.0799878456142551, -181.9874144716870887, 362.9823548866085616 ) ) ;
#42070 = CARTESIAN_POINT ( 'NONE',  ( 797.8594530101008786, -325.5436935675105019, -322.1405469898980982 ) ) ;
#42071 = CARTESIAN_POINT ( 'NONE',  ( 911.9999999999993179, 154.9999999999998863, 350.0000000000000000 ) ) ;
#42072 = CARTESIAN_POINT ( 'NONE',  ( 780.5236548040995785, -212.7363362996982232, -314.9735926884559944 ) ) ;
#42073 = CARTESIAN_POINT ( 'NONE',  ( 751.9810565676468741, -26.08914811296592262, 360.9747183278973921 ) ) ;
#42074 = CARTESIAN_POINT ( 'NONE',  ( 814.9108240113580450, -64.27096629478397460, 337.5031285880265273 ) ) ;
#42075 = CARTESIAN_POINT ( 'NONE',  ( 802.3178104526313064, -452.9681489794448339, 352.6268974387025423 ) ) ;
#42076 = CARTESIAN_POINT ( 'NONE',  ( 763.0537975583476964, -408.4527844766009821, -371.0346526505628617 ) ) ;
#42077 = CARTESIAN_POINT ( 'NONE',  ( 831.1634899080286232, 259.9999999999998863, -191.9749999999999943 ) ) ;
#42078 = CARTESIAN_POINT ( 'NONE',  ( 814.4686193811664907, -339.2817908451524431, 346.2056067578752732 ) ) ;
#42079 = FACE_OUTER_BOUND ( 'NONE', #2545, .T. ) ;
#42080 = CARTESIAN_POINT ( 'NONE',  ( 804.7487373415286811, -331.5436935675104451, 364.7487373415288516 ) ) ;
#42081 = CARTESIAN_POINT ( 'NONE',  ( 787.4397851343537695, -69.72551174932942786, -374.2001403089903988 ) ) ;
#42082 = CARTESIAN_POINT ( 'NONE',  ( 788.7366044899766848, -299.9073299311468759, -316.5762568750059813 ) ) ;
#42083 = DIRECTION ( 'NONE',  ( 0.000000000000000000, 0.000000000000000000, -1.000000000000000000 ) ) ;
#42084 = CARTESIAN_POINT ( 'NONE',  ( 797.8594530101008786, -397.5436935675100472, 322.1405469898980982 ) ) ;
#42085 = CARTESIAN_POINT ( 'NONE',  ( 759.0159684113467620, -160.9181544815165807, 325.8855110935213020 ) ) ;
#42086 = CARTESIAN_POINT ( 'NONE',  ( 793.5525998758768083, -31.09997266333516919, -372.6845335610516941 ) ) ;
#42087 = CARTESIAN_POINT ( 'NONE',  ( 789.9200121543843807, -73.98741447168741558, -317.0176451133914384 ) ) ;
#42088 = CARTESIAN_POINT ( 'NONE',  ( 813.9316612368132837, -79.44195992623286884, 348.6739635108323228 ) ) ;
#42089 = CARTESIAN_POINT ( 'NONE',  ( 764.8639956371174549, -392.0891481129647786, 319.7806653035542581 ) ) ;
#42090 = CARTESIAN_POINT ( 'NONE',  ( 829.9999999999992042, 579.9999999999998863, -360.0000000000000000 ) ) ;
#42091 = FILL_AREA_STYLE_COLOUR ( '', #8542 ) ;
#42092 = CARTESIAN_POINT ( 'NONE',  ( 774.6858677611749044, -9.725511749329603717, -315.5713283507209894 ) ) ;
#42094 = ORIENTED_EDGE ( 'NONE', *, *, #2411, .T. ) ;
#42093 = CARTESIAN_POINT ( 'NONE',  ( 783.0433043558608688, -96.89650538077825104, -315.1538015810313027 ) ) ;
#42095 = CARTESIAN_POINT ( 'NONE',  ( 774.6858677611749044, -57.72551174932945628, -315.5713283507209894 ) ) ;
#42096 = CARTESIAN_POINT ( 'NONE',  ( 755.0488828828309806, -377.8055962898682765, -344.1219089521771934 ) ) ;
#42098 = CARTESIAN_POINT ( 'NONE',  ( 757.8323909638828582, -242.6346026584197659, 352.1044303154654358 ) ) ;
#42097 = CARTESIAN_POINT ( 'NONE',  ( 756.5762568750052424, -219.1800572038744122, 348.7366044899774238 ) ) ;
#42099 = ORIENTED_EDGE ( 'NONE', *, *, #5239, .F. ) ;
#42100 = CARTESIAN_POINT ( 'NONE',  ( 764.3348316497523456, -406.7146871989590409, -308.6759233522265617 ) ) ;
#42101 = DIRECTION ( 'NONE',  ( -1.000000000000000000, -0.000000000000000000, 0.000000000000000000 ) ) ;
#42102 = ORIENTED_EDGE ( 'NONE', *, *, #42169, .F. ) ;
#42103 = CARTESIAN_POINT ( 'NONE',  ( 771.1735550268778070, -441.1800572038735027, 316.3353852180827630 ) ) ;
#42104 = EDGE_LOOP ( 'NONE', ( #18675, #6018 ) ) ;
#42105 = CARTESIAN_POINT ( 'NONE',  ( 804.7487373415286811, -235.5436935675107293, -364.7487373415288516 ) ) ;
#42106 = CARTESIAN_POINT ( 'NONE',  ( 787.4397851343537695, -141.7255117493291721, 374.2001403089903988 ) ) ;
#42107 = VERTEX_POINT ( 'NONE', #9170 ) ;
#42108 = CARTESIAN_POINT ( 'NONE',  ( 804.4286716492782716, -233.3618753856925423, -345.3141322388244703 ) ) ;
#42109 = VERTEX_POINT ( 'NONE', #27407 ) ;
#42110 = CARTESIAN_POINT ( 'NONE',  ( 758.0580252608178853, -366.4527844766012095, -328.0187753319985404 ) ) ;
#42111 = CARTESIAN_POINT ( 'NONE',  ( 756.5762568750052424, -3.180057203875080063, -348.7366044899774238 ) ) ;
#42112 = CARTESIAN_POINT ( 'NONE',  ( 770.0799878456142551, -229.9874144716869466, 362.9823548866085616 ) ) ;
#42113 = CARTESIAN_POINT ( 'NONE',  ( 789.9999999999992042, 205.0000000000000568, -339.9999999999999432 ) ) ;
#42114 = EDGE_CURVE ( 'NONE', #44996, #44015, #12637, .T. ) ;
#42115 = CARTESIAN_POINT ( 'NONE',  ( 911.9999999999993179, 219.9999999999998863, -360.0000000000000000 ) ) ;
#42116 = ORIENTED_EDGE ( 'NONE', *, *, #22196, .F. ) ;
#42117 = CARTESIAN_POINT ( 'NONE',  ( 759.7806653035534055, -30.99823902205680071, -324.8639956371180801 ) ) ;
#42118 = PLANE ( 'NONE',  #3270 ) ;
#42119 = LINE ( 'NONE', #9791, #17473 ) ;
#42120 = ORIENTED_EDGE ( 'NONE', *, *, #35917, .T. ) ;
#42121 = CARTESIAN_POINT ( 'NONE',  ( 768.9521613784389729, -273.8272453906071746, -373.2346286133773106 ) ) ;
#42122 = CARTESIAN_POINT ( 'NONE',  ( 811.3240766477731540, -124.3726999360621619, 355.6651683502462902 ) ) ;
#42124 = CARTESIAN_POINT ( 'NONE',  ( 788.8264449731200330, -237.1800572038742985, -363.6646147819171233 ) ) ;
#42123 = DIRECTION ( 'NONE',  ( -1.644774851296528363E-16, 1.000000000000000000, 0.000000000000000000 ) ) ;
#42125 = CARTESIAN_POINT ( 'NONE',  ( 764.0069404352550464, -399.0783235625955285, -359.2566176426627180 ) ) ;
#42126 = CARTESIAN_POINT ( 'NONE',  ( 911.9749999999993406, 154.9999999999998863, 350.0000000000000000 ) ) ;
#42127 = FACE_OUTER_BOUND ( 'NONE', #22217, .T. ) ;
#42128 = CARTESIAN_POINT ( 'NONE',  ( 772.4468031744293057, -105.8272453906076578, -363.8651313633793620 ) ) ;
#42129 = CARTESIAN_POINT ( 'NONE',  ( 814.8207195650702488, -386.1908817542432075, 336.2433038121456548 ) ) ;
#42130 = FACE_OUTER_BOUND ( 'NONE', #28022, .T. ) ;
#42131 = CARTESIAN_POINT ( 'NONE',  ( 813.2346286133761168, 18.73985825558501972, -328.9521613784389160 ) ) ;
#42132 = CARTESIAN_POINT ( 'NONE',  ( 814.9108240113580450, -304.2709662947832499, -337.5031285880265273 ) ) ;
#42133 = CYLINDRICAL_SURFACE ( 'NONE', #2505, 10.00000000000000888 ) ;
#42134 = CARTESIAN_POINT ( 'NONE',  ( 939.9999999999992042, 62.85347435602262323, -357.4246812887967621 ) ) ;
#42135 = CARTESIAN_POINT ( 'NONE',  ( 785.3141322388236176, -69.72551174932942786, -364.4286716492789537 ) ) ;
#42136 = CARTESIAN_POINT ( 'NONE',  ( 783.7953271457878373, -248.1908817542435202, 375.1787889125761239 ) ) ;
#42137 = CARTESIAN_POINT ( 'NONE',  ( 749.8865473780648472, -188.5328690171416497, -322.1177392798429082 ) ) ;
#42138 = CARTESIAN_POINT ( 'NONE',  ( 814.2001403089898304, -185.3618753856926844, 347.4397851343538264 ) ) ;
#42139 = CARTESIAN_POINT ( 'NONE',  ( 808.0189434323515343, -446.0891481129646081, -319.0252816721025511 ) ) ;
#42140 = DIRECTION ( 'NONE',  ( 0.000000000000000000, -1.000000000000000000, 0.000000000000000000 ) ) ;
#42141 = EDGE_CURVE ( 'NONE', #34629, #20464, #6834, .T. ) ;
#42142 = CARTESIAN_POINT ( 'NONE',  ( 754.8072714833581358, -292.8164208402376971, 338.1981804954720587 ) ) ;
#42143 = CARTESIAN_POINT ( 'NONE',  ( 766.0291762391763086, -82.91815448151682233, 360.7704444035551319 ) ) ;
#42144 = CARTESIAN_POINT ( 'NONE',  ( 789.5670355615794733, -453.0432664090020012, -363.0970091259334822 ) ) ;
#42145 = DIRECTION ( 'NONE',  ( 1.000000000000000000, -0.000000000000000000, 0.000000000000000000 ) ) ;
#42146 = DIRECTION ( 'NONE',  ( -0.000000000000000000, 0.000000000000000000, -1.000000000000000000 ) ) ;
#42148 = CARTESIAN_POINT ( 'NONE',  ( 774.6858677611749044, -321.7255117493286320, 315.5713283507209894 ) ) ;
#42147 = CARTESIAN_POINT ( 'NONE',  ( 757.2208543904082489, -112.7146871989600356, 350.9844846989624330 ) ) ;
#42149 = VERTEX_POINT ( 'NONE', #34337 ) ;
#42150 = CARTESIAN_POINT ( 'NONE',  ( 794.1144889064781864, -274.1692326535049915, -360.9840315886528401 ) ) ;
#42151 = CARTESIAN_POINT ( 'NONE',  ( 762.3223304703356007, -79.54369356751119824, 322.3223304703362828 ) ) ;
#42152 = CARTESIAN_POINT ( 'NONE',  ( 745.1769319972822814, -281.8055962898686175, -346.2694204179732083 ) ) ;
#42153 = CARTESIAN_POINT ( 'NONE',  ( 1238.921997096861332, 430.0000000000002842, -244.9999999999999716 ) ) ;
#42154 = CARTESIAN_POINT ( 'NONE',  ( 815.1787889125755555, -414.8965053807771710, 343.7953271457877804 ) ) ;
#42155 = ORIENTED_EDGE ( 'NONE', *, *, #22701, .T. ) ;
#42156 = CARTESIAN_POINT ( 'NONE',  ( 800.0135310231082713, -302.0891481129650629, 325.0180583372163028 ) ) ;
#42157 = CARTESIAN_POINT ( 'NONE',  ( 761.2382568024794409, -39.62377810805116951, -356.9571628226838129 ) ) ;
#42158 = CARTESIAN_POINT ( 'NONE',  ( 759.7806653035534055, -198.9982390220562252, -324.8639956371180801 ) ) ;
#42159 = CARTESIAN_POINT ( 'NONE',  ( 803.4237431249931660, -399.1800572038738437, 331.2633955100225194 ) ) ;
#42160 = EDGE_CURVE ( 'NONE', #43869, #31480, #38046, .T. ) ;
#42161 = CARTESIAN_POINT ( 'NONE',  ( 796.7737145352015204, -140.6346026584201070, -370.7187646348536987 ) ) ;
#42162=STYLED_ITEM('',(#45744),#17465);
#42163 = CARTESIAN_POINT ( 'NONE',  ( 757.8323909638828582, -98.63460265842023489, -352.1044303154654358 ) ) ;
#42164 = ORIENTED_EDGE ( 'NONE', *, *, #33494, .T. ) ;
#42165 = CARTESIAN_POINT ( 'NONE',  ( 769.0155153010367712, -394.3726999360613377, -362.7791456095907279 ) ) ;
#42167 = CARTESIAN_POINT ( 'NONE',  ( 790.0220218866281812, -439.0999726633339719, 363.2186876482849129 ) ) ;
#42166 = CARTESIAN_POINT ( 'NONE',  ( 759.7806653035534055, -126.9982390220565094, 324.8639956371180801 ) ) ;
#42168 = CARTESIAN_POINT ( 'NONE',  ( 757.2208543904082489, -112.7146871989600356, 350.9844846989624330 ) ) ;
#42169 = EDGE_CURVE ( 'NONE', #5383, #38472, #42972, .T. ) ;
#42172 = CARTESIAN_POINT ( 'NONE',  ( 812.6845335610512393, -391.9874144716864066, 353.5525998758768651 ) ) ;
#42171 = CARTESIAN_POINT ( 'NONE',  ( 799.9999999999993179, 205.0000000000000568, 245.0000000000000284 ) ) ;
#42170 = CARTESIAN_POINT ( 'NONE',  ( 949.5497976682736407, 120.6654763175833693, 339.9999999999999432 ) ) ;
#42173 = EDGE_CURVE ( 'NONE', #16933, #24181, #15673, .T. ) ;
#42174 = VERTEX_POINT ( 'NONE', #16801 ) ;
#42175 = CARTESIAN_POINT ( 'NONE',  ( 755.1538015810308480, -350.1908817542433212, -343.0433043558613804 ) ) ;
#42176 = CARTESIAN_POINT ( 'NONE',  ( 759.7806653035534055, -366.9982390220556567, -324.8639956371180801 ) ) ;
#42177 = CARTESIAN_POINT ( 'NONE',  ( 766.4474001241216001, -163.0999726633347677, -307.3154664389482491 ) ) ;
#42178 = CARTESIAN_POINT ( 'NONE',  ( 781.2370466360911223, -44.73633629969875614, 304.9990715423533629 ) ) ;
#42180 = FACE_OUTER_BOUND ( 'NONE', #27549, .T. ) ;
#42179 = DIRECTION ( 'NONE',  ( 1.000000000000000000, 0.000000000000000000, 0.000000000000000000 ) ) ;
#42181 = CARTESIAN_POINT ( 'NONE',  ( 757.2208543904082489, -280.7146871989594956, -350.9844846989624330 ) ) ;
#42182 = CARTESIAN_POINT ( 'NONE',  ( 771.1735550268778070, -441.1800572038735027, -316.3353852180827630 ) ) ;
#42183 = CARTESIAN_POINT ( 'NONE',  ( 746.4236121716829757, -159.8272453906075157, -328.8385539511384650 ) ) ;
#42184 = FACE_OUTER_BOUND ( 'NONE', #42104, .T. ) ;
#42185 = CARTESIAN_POINT ( 'NONE',  ( 989.9999999999992042, 249.9999999999998863, -350.0000000000000000 ) ) ;
#42186 = CARTESIAN_POINT ( 'NONE',  ( 780.5236548040995785, -380.7363362996977116, 314.9735926884559944 ) ) ;
#42187 = CARTESIAN_POINT ( 'NONE',  ( 814.2805881961230625, -337.6454272087888171, 331.2368401574024119 ) ) ;
#42188 = CARTESIAN_POINT ( 'NONE',  ( 814.9108240113580450, -208.2709662947835341, -337.5031285880265273 ) ) ;
#42189 = EDGE_CURVE ( 'NONE', #33196, #19590, #44280, .T. ) ;
#42190 = CARTESIAN_POINT ( 'NONE',  ( 441.1634899080286232, 239.9999999999999716, -202.7499999999971010 ) ) ;
#42191 = DIRECTION ( 'NONE',  ( -0.000000000000000000, 1.000000000000000000, -0.000000000000000000 ) ) ;
#42192 = CARTESIAN_POINT ( 'NONE',  ( 781.2370466360911223, -140.7363362996984506, 304.9990715423533629 ) ) ;
#42193 = ADVANCED_FACE ( 'NONE', ( #24169 ), #30880, .F. ) ;
#42194 = CARTESIAN_POINT ( 'NONE',  ( 754.0944755984390895, -111.6237781080509279, -364.1009440267246760 ) ) ;
#42195 = CARTESIAN_POINT ( 'NONE',  ( 767.7687537140311633, -335.9073299311468190, -372.7932403749916830 ) ) ;
#42196 = CARTESIAN_POINT ( 'NONE',  ( 786.4999999999993179, -496.5085659523897448, -356.8883017825714319 ) ) ;
#42197 = LINE ( 'NONE', #16581, #43390 ) ;
#42198 = CARTESIAN_POINT ( 'NONE',  ( 762.1405469898971887, -193.5436935675108714, 357.8594530101015607 ) ) ;
#42199 = VECTOR ( 'NONE', #17019, 1000.000000000000000 ) ;
#42200 = ORIENTED_EDGE ( 'NONE', *, *, #20424, .T. ) ;
#42201 = CARTESIAN_POINT ( 'NONE',  ( 750.9282345327678740, -448.9181544815156144, 319.8311093483690115 ) ) ;
#42202 = CARTESIAN_POINT ( 'NONE',  ( 758.0141637701419768, -375.0783235625955285, -367.2620300519063790 ) ) ;
#42203 = CARTESIAN_POINT ( 'NONE',  ( 745.4481719005789273, -147.7255117493291152, -347.5162901302853129 ) ) ;
#42204 = CARTESIAN_POINT ( 'NONE',  ( 749.2812353651451076, -438.4527844766009821, -323.2262854647983090 ) ) ;
#42205 = CARTESIAN_POINT ( 'NONE',  ( -775.4999999999993179, -365.3551492539851893, -18.13243251470705886 ) ) ;
#42206 = CARTESIAN_POINT ( 'NONE',  ( 810.1134526219336749, -8.532869017142163059, 357.8822607201570349 ) ) ;
#42207 = ORIENTED_EDGE ( 'NONE', *, *, #14906, .T. ) ;
#42208 = CARTESIAN_POINT ( 'NONE',  ( 744.8212110874229666, -186.8965053807779668, -336.2046728542121627 ) ) ;
#42209 = CARTESIAN_POINT ( 'NONE',  ( -786.4999999999993179, -365.3551492539851893, -28.13243251470704109 ) ) ;
#42210 = CARTESIAN_POINT ( 'NONE',  ( 800.1688906516307043, -322.1692326535048210, 369.0717654672308186 ) ) ;
#42211 = CARTESIAN_POINT ( 'NONE',  ( 805.1927285166399315, -136.8164208402382656, 341.8018195045277707 ) ) ;
#42212 = VERTEX_POINT ( 'NONE', #2705 ) ;
#42213 = EDGE_CURVE ( 'NONE', #18941, #7747, #30190, .T. ) ;
#42214 = CARTESIAN_POINT ( 'NONE',  ( 757.8323909638827445, -314.6346026584194533, 352.1044303154654358 ) ) ;
#42215 = EDGE_CURVE ( 'NONE', #20750, #27073, #2933, .T. ) ;
#42216 = CARTESIAN_POINT ( 'NONE',  ( 813.1304606946830518, -17.90732993114776406, -352.3570229623690580 ) ) ;
#42217 = AXIS2_PLACEMENT_3D ( 'NONE', #18908, #22803, #32761 ) ;
#42218 = LINE ( 'NONE', #34605, #35733 ) ;
#42219 = VERTEX_POINT ( 'NONE', #30651 ) ;
#42220 = CARTESIAN_POINT ( 'NONE',  ( 814.8207195650702488, -410.1908817542430370, -336.2433038121456548 ) ) ;
#42221 = ORIENTED_EDGE ( 'NONE', *, *, #34585, .T. ) ;
#42222 = CARTESIAN_POINT ( 'NONE',  ( 785.3687786644884454, -275.3618753856923149, -315.3201227861279676 ) ) ;
#42223 = EDGE_CURVE ( 'NONE', #6383, #10220, #5711, .T. ) ;
#42225 = CARTESIAN_POINT ( 'NONE',  ( 751.2241431872005251, -256.1692326535049915, 359.9636004259367610 ) ) ;
#42224 = CARTESIAN_POINT ( 'NONE',  ( 814.2001403089898304, -377.3618753856920875, 347.4397851343538264 ) ) ;
#42226 = EDGE_CURVE ( 'NONE', #43683, #34870, #45188, .T. ) ;
#42227 = CARTESIAN_POINT ( 'NONE',  ( 755.5913626894240451, -253.6454272087889876, -346.6156483768012890 ) ) ;
#42228 = CARTESIAN_POINT ( 'NONE',  ( 788.8264449731200330, -237.1800572038742985, -363.6646147819171233 ) ) ;
#42229 = CARTESIAN_POINT ( 'NONE',  ( 959.5497976682736407, 239.9999999999998863, 350.0000000000000000 ) ) ;
#42230 = CARTESIAN_POINT ( 'NONE',  ( 758.0580252608178853, -102.4527844766020337, -328.0187753319985404 ) ) ;
#42231 = CARTESIAN_POINT ( 'NONE',  ( 791.9812246680005501, -236.6346026584198228, 361.9419747391813189 ) ) ;
#42232 = CARTESIAN_POINT ( 'NONE',  ( 813.1304606946830518, -377.9073299311466485, 352.3570229623690580 ) ) ;
#42234 = DIRECTION ( 'NONE',  ( 0.000000000000000000, -1.000000000000000000, 0.000000000000000000 ) ) ;
#42233 = CARTESIAN_POINT ( 'NONE',  ( -879.9999999999992042, 240.0000000000002274, -219.9999999999999716 ) ) ;
#42235 = CARTESIAN_POINT ( 'NONE',  ( 797.8822607201568644, -54.55451811788054783, -370.1134526219340160 ) ) ;
#42236 = CARTESIAN_POINT ( 'NONE',  ( 879.9999999999992042, 239.9999999999998863, -179.9999999999999716 ) ) ;
#42237 = CARTESIAN_POINT ( 'NONE',  ( 999.9999999999992042, 249.9999999999998863, 359.0000000000000000 ) ) ;
#42238 = CARTESIAN_POINT ( 'NONE',  ( 790.0220218866281812, -247.0999726633344835, 363.2186876482849129 ) ) ;
#42239 = CARTESIAN_POINT ( 'NONE',  ( 797.8594530101008786, -109.5436935675110988, 322.1405469898980982 ) ) ;
#42240 = ORIENTED_EDGE ( 'NONE', *, *, #27263, .T. ) ;
#42241 = CARTESIAN_POINT ( 'NONE',  ( 804.4086373105744769, -25.64542720878973014, -333.3843516231986541 ) ) ;
#42242 = CARTESIAN_POINT ( 'NONE',  ( 800.9747183278959710, -108.9982390220565804, -311.9810565676471583 ) ) ;
#42243 = CARTESIAN_POINT ( 'NONE',  ( 779.4709603349208464, -288.3510508353231216, 314.7162404726379918 ) ) ;
#42244 = CARTESIAN_POINT ( 'NONE',  ( 801.9419747391806368, -450.4527844766009821, -351.9812246680014027 ) ) ;
#42245 = CARTESIAN_POINT ( 'NONE',  ( 766.4474001241216001, -43.09997266333511590, 307.3154664389482491 ) ) ;
#42246 = CARTESIAN_POINT ( 'NONE',  ( 782.4968714119720516, -250.8164208402379245, -305.0891759886411023 ) ) ;
#42247 = CARTESIAN_POINT ( 'NONE',  ( 796.7737145352015204, -164.6346026584200217, 370.7187646348536987 ) ) ;
#42248 = CARTESIAN_POINT ( 'NONE',  ( 774.6312213355099630, -95.36187538569294020, 364.6798772138717482 ) ) ;
#42249 = AXIS2_PLACEMENT_3D ( 'NONE', #12135, #1713, #43540 ) ;
#42250 = DIRECTION ( 'NONE',  ( 1.000000000000000000, 0.000000000000000000, 0.000000000000000000 ) ) ;
#42251 = CARTESIAN_POINT ( 'NONE',  ( 771.2368401574024119, -277.4419599262322436, -374.2805881961240857 ) ) ;
#42252 = CARTESIAN_POINT ( 'NONE',  ( 793.5525998758768083, -439.0999726633339719, 372.6845335610516941 ) ) ;
#42253 = CARTESIAN_POINT ( 'NONE',  ( 787.4397851343537695, -333.7255117493286320, -374.2001403089903988 ) ) ;
#42254 = FACE_BOUND ( 'NONE', #16958, .T. ) ;
#42255 = CARTESIAN_POINT ( 'NONE',  ( 755.8398074228967971, -355.4419599262319593, 333.4516893846970333 ) ) ;
#42256 = CARTESIAN_POINT ( 'NONE',  ( 787.5162901302840055, -35.36187538569316047, 305.4481719005793252 ) ) ;
#42257 = CARTESIAN_POINT ( 'NONE',  ( 788.8264449731200330, -381.1800572038737869, -363.6646147819171233 ) ) ;
#42258 = CARTESIAN_POINT ( 'NONE',  ( 772.3691319403857278, -47.26014174441477422, 315.8894580844506663 ) ) ;
#42259 = CARTESIAN_POINT ( 'NONE',  ( 798.0661480581538854, -50.53286901714203339, -309.5768839229118043 ) ) ;
#42260 = CARTESIAN_POINT ( 'NONE',  ( 798.0661480581538854, -194.5328690171415644, 309.5768839229118043 ) ) ;
#42261 = CARTESIAN_POINT ( 'NONE',  ( 801.9419747391806368, -18.45278447660230725, 351.9812246680014027 ) ) ;
#42262 = ADVANCED_FACE ( 'NONE', ( #20246 ), #2009, .F. ) ;
#42263 = VERTEX_POINT ( 'NONE', #33882 ) ;
#42264 = CARTESIAN_POINT ( 'NONE',  ( 795.9930595647434757, -195.0783235625961538, -320.7433823573372820 ) ) ;
#42265 = CARTESIAN_POINT ( 'NONE',  ( 802.1676090361156639, -182.6346026584199649, 327.8955696845344505 ) ) ;
#42266 = CARTESIAN_POINT ( 'NONE',  ( 776.2433038121456548, -36.89650538077844288, -374.8207195650711014 ) ) ;
#42267 = CARTESIAN_POINT ( 'NONE',  ( 791.9812246680005501, -332.6346026584195101, 361.9419747391813189 ) ) ;
#42268 = LINE ( 'NONE', #10872, #16111 ) ;
#42269 = ORIENTED_EDGE ( 'NONE', *, *, #19866, .T. ) ;
#42270 = CARTESIAN_POINT ( 'NONE',  ( 757.2208543904082489, -40.71468719896024879, 350.9844846989624330 ) ) ;
#42271 = CARTESIAN_POINT ( 'NONE',  ( 814.2805881961230625, -313.6454272087888171, -331.2368401574024119 ) ) ;
#42272 = CARTESIAN_POINT ( 'NONE',  ( 813.1304606946831655, -257.9073299311469327, 352.3570229623691716 ) ) ;
#42273 = CARTESIAN_POINT ( 'NONE',  ( 815.1787889125755555, -6.896505380778533478, 343.7953271457877804 ) ) ;
#42274 = CARTESIAN_POINT ( 'NONE',  ( 755.1538015810308480, -158.1908817542438612, -343.0433043558613804 ) ) ;
#42275 = CARTESIAN_POINT ( 'NONE',  ( 767.8955696845333705, -144.4527844766018632, -362.1676090361162323 ) ) ;
#42276 = VECTOR ( 'NONE', #35514, 1000.000000000000000 ) ;
#42277 = CARTESIAN_POINT ( 'NONE',  ( 771.2633955100217236, -335.9073299311468190, -363.4237431249939618 ) ) ;
#42278 = EDGE_LOOP ( 'NONE', ( #9077, #1795 ) ) ;
#42279 = CARTESIAN_POINT ( 'NONE',  ( 801.1904061080336987, -284.0891481129650629, 368.3070685750235498 ) ) ;
#42280 = FACE_OUTER_BOUND ( 'NONE', #4851, .T. ) ;
#42281 = CARTESIAN_POINT ( 'NONE',  ( 784.0799538623451781, -347.8055962898683333, 364.6971507214555572 ) ) ;
#42282 = CARTESIAN_POINT ( 'NONE',  ( 317.2824899080285945, 256.5000000000000000, -199.9999999999963336 ) ) ;
#42283 = CARTESIAN_POINT ( 'NONE',  ( 802.5472867521000353, -148.3726999360620198, 350.8726784830461156 ) ) ;
#42284 = CARTESIAN_POINT ( 'NONE',  ( 774.6312213355099630, 0.6381246143067236254, 364.6798772138717482 ) ) ;
#42285 = ORIENTED_EDGE ( 'NONE', *, *, #3156, .F. ) ;
#42286 = CARTESIAN_POINT ( 'NONE',  ( 813.5763878283155464, -363.8272453906068336, -351.1614460488615350 ) ) ;
#42287 = CARTESIAN_POINT ( 'NONE',  ( 782.4968714119720516, -10.81642084023869543, -305.0891759886411023 ) ) ;
#42288 = CARTESIAN_POINT ( 'NONE',  ( 766.4474001241216001, -235.0999726633344835, 307.3154664389482491 ) ) ;
#42289 = CARTESIAN_POINT ( 'NONE',  ( 804.9511171171677688, -197.8055962898688733, 335.8780910478229202 ) ) ;
#42290 = CARTESIAN_POINT ( 'NONE',  ( 794.9819416627830151, -372.9982390220557704, -319.9864689768909898 ) ) ;
#42291 = AXIS2_PLACEMENT_3D ( 'NONE', #6128, #3364, #34989 ) ;
#42292 = CARTESIAN_POINT ( 'NONE',  ( 796.1575198192839480, -438.0090635724247932, 359.4546378042384163 ) ) ;
#42293 = CARTESIAN_POINT ( 'NONE',  ( 759.0159684113467620, -232.9181544815163249, -325.8855110935213020 ) ) ;
#42294 = CARTESIAN_POINT ( 'NONE',  ( 782.4968714119720516, -10.81642084023869543, 305.0891759886411023 ) ) ;
#42295 = CARTESIAN_POINT ( 'NONE',  ( 787.4397851343537695, -69.72551174932942786, 374.2001403089903988 ) ) ;
#42296 = DIRECTION ( 'NONE',  ( -0.000000000000000000, 1.000000000000000000, -0.000000000000000000 ) ) ;
#42297 = CARTESIAN_POINT ( 'NONE',  ( 746.8695393053151292, -413.9073299311465348, -327.6429770376306578 ) ) ;
#42298 = DIRECTION ( 'NONE',  ( -0.000000000000000000, -0.000000000000000000, 1.000000000000000000 ) ) ;
#42299 = CARTESIAN_POINT ( 'NONE',  ( 791.0478386215596629, -357.8272453906068904, 306.7653713866226326 ) ) ;
#42300 = FACE_OUTER_BOUND ( 'NONE', #11715, .T. ) ;
#42301 = CARTESIAN_POINT ( 'NONE',  ( 772.4837098697144029, -335.3618753856920307, 374.5518280994205611 ) ) ;
#42302 = CARTESIAN_POINT ( 'NONE',  ( 754.9967657858570647, -49.54369356751129061, -365.0032342141425374 ) ) ;
#42303 = CARTESIAN_POINT ( 'NONE',  ( 802.1676090361156639, -278.6346026584196807, -327.8955696845344505 ) ) ;
#42304 = CARTESIAN_POINT ( 'NONE',  ( 311.1634899080286232, 260.0000000000000000, -199.9999999999963336 ) ) ;
#42305 = CARTESIAN_POINT ( 'NONE',  ( 781.7834795799800531, -418.8164208402374129, 315.0636971347436202 ) ) ;
#42306 = CARTESIAN_POINT ( 'NONE',  ( 773.4516893846965786, -163.6454272087893003, 315.8398074228977066 ) ) ;
#42307 = CARTESIAN_POINT ( 'NONE',  ( 745.1792804349281596, -14.19088175424431242, -343.7566961878542884 ) ) ;
#42308 = CARTESIAN_POINT ( 'NONE',  ( 758.6633372737375112, -68.53286901714197654, -326.9102291470432533 ) ) ;
#42309 = CARTESIAN_POINT ( 'NONE',  ( 801.9858362298568863, -99.07832356259642381, 312.7379699480935642 ) ) ;
#42310 = CARTESIAN_POINT ( 'NONE',  ( 803.6646147819162707, -401.9073299311464211, 348.8264449731211130 ) ) ;
#42311 = FACE_OUTER_BOUND ( 'NONE', #43736, .T. ) ;
#42312 = CARTESIAN_POINT ( 'NONE',  ( 803.8556311672234642, -153.6237781080508000, 365.6418435158340117 ) ) ;
#42313 = CARTESIAN_POINT ( 'NONE',  ( 800.2193346964447755, 5.001760977943074948, -355.1360043628815788 ) ) ;
#42314 = ORIENTED_EDGE ( 'NONE', *, *, #44997, .T. ) ;
#42315 = CARTESIAN_POINT ( 'NONE',  ( 800.2193346964447755, -90.99823902205663728, -355.1360043628815788 ) ) ;
#42316 = CARTESIAN_POINT ( 'NONE',  ( 770.0799878456142551, -397.9874144716864066, -362.9823548866085616 ) ) ;
#42318 = CARTESIAN_POINT ( 'NONE',  ( 804.4286716492782716, -233.3618753856925423, 345.3141322388244703 ) ) ;
#42317 = CARTESIAN_POINT ( 'NONE',  ( 755.0636971347428243, -244.2709662947834204, 341.7834795799807353 ) ) ;
#42319 = CARTESIAN_POINT ( 'NONE',  ( 761.9338519418445230, -398.5328690171409107, -370.4231160770881957 ) ) ;
#42320 = CARTESIAN_POINT ( 'NONE',  ( 801.1904061080336987, 3.910851887033985896, 368.3070685750235498 ) ) ;
#42321 = FACE_OUTER_BOUND ( 'NONE', #29882, .T. ) ;
#42322 = VERTEX_POINT ( 'NONE', #6404 ) ;
#42323 = CARTESIAN_POINT ( 'NONE',  ( 797.8594530101008786, -421.5436935675101040, 322.1405469898980982 ) ) ;
#42324 = VECTOR ( 'NONE', #23636, 1000.000000000000000 ) ;
#42325 = ORIENTED_EDGE ( 'NONE', *, *, #8056, .F. ) ;
#42326 = CARTESIAN_POINT ( 'NONE',  ( 763.2262854647970016, -248.6346026584197659, -309.2812353651462445 ) ) ;
#42327 = CARTESIAN_POINT ( 'NONE',  ( 814.5518280994195948, -159.7255117493291436, 332.4837098697145166 ) ) ;
#42328 = ORIENTED_EDGE ( 'NONE', *, *, #6905, .F. ) ;
#42329 = CARTESIAN_POINT ( 'NONE',  ( 762.3223304703356007, -247.5436935675106724, -322.3223304703362828 ) ) ;
#42330 = ORIENTED_EDGE ( 'NONE', *, *, #8660, .T. ) ;
#42331 = CARTESIAN_POINT ( 'NONE',  ( 755.0636971347428243, -364.2709662947830793, -341.7834795799807353 ) ) ;
#42332 = CARTESIAN_POINT ( 'NONE',  ( 765.0180583372156207, -24.99823902205683268, -360.0135310231089534 ) ) ;
#42333 = CARTESIAN_POINT ( 'NONE',  ( 765.8855110935204493, -238.1692326535050768, 319.0159684113471599 ) ) ;
#42334 = CARTESIAN_POINT ( 'NONE',  ( -28.63011601220122415, -544.8427095258973623, -350.0000000000000000 ) ) ;
#42335 = DIRECTION ( 'NONE',  ( 0.000000000000000000, 0.000000000000000000, -1.000000000000000000 ) ) ;
#42336 = ORIENTED_EDGE ( 'NONE', *, *, #44180, .F. ) ;
#42337 = CARTESIAN_POINT ( 'NONE',  ( 755.3201227861273992, -27.72551174932954510, -345.3687786644892981 ) ) ;
#42338 = DIRECTION ( 'NONE',  ( -0.000000000000000000, 1.000000000000000000, -0.000000000000000000 ) ) ;
#42339 = CARTESIAN_POINT ( 'NONE',  ( -180.7583438952261474, 1.505115564641941601E-13, -244.9999999999999716 ) ) ;
#42340 = AXIS2_PLACEMENT_3D ( 'NONE', #5415, #29685, #5201 ) ;
#42341 = VERTEX_POINT ( 'NONE', #41740 ) ;
#42342 = CARTESIAN_POINT ( 'NONE',  ( 747.6481478633932056, -277.0999726633344267, -353.4146539503763620 ) ) ;
#42343 = CIRCLE ( 'NONE', #38662, 2.749999999999919176 ) ;
#42344 = CARTESIAN_POINT ( 'NONE',  ( 797.8822607201568644, -150.5545181178802352, 370.1134526219340160 ) ) ;
#42346 = CARTESIAN_POINT ( 'NONE',  ( 768.0187753319979720, -248.6346026584197659, -318.0580252608186242 ) ) ;
#42345 = DIRECTION ( 'NONE',  ( 0.000000000000000000, 0.000000000000000000, -1.000000000000000000 ) ) ;
#42347 = CARTESIAN_POINT ( 'NONE',  ( 756.1348686366196716, -401.2601417444137155, -347.5531968255698416 ) ) ;
#42348 = DIRECTION ( 'NONE',  ( 0.000000000000000000, 0.000000000000000000, 1.000000000000000000 ) ) ;
#42349 = CARTESIAN_POINT ( 'NONE',  ( 775.8780910478218402, -105.2817908451530968, -364.9511171171680530 ) ) ;
#42350 = CARTESIAN_POINT ( 'NONE',  ( 746.4236121716829757, -375.8272453906069472, 328.8385539511384650 ) ) ;
#42351 = LINE ( 'NONE', #45615, #14479 ) ;
#42352 = CARTESIAN_POINT ( 'NONE',  ( 764.3348316497523456, 1.285312801039623753, -308.6759233522265617 ) ) ;
#42353 = CARTESIAN_POINT ( 'NONE',  ( 812.7932403749906598, -327.1800572038741279, -327.7687537140311633 ) ) ;
#42354 = LINE ( 'NONE', #35421, #12832 ) ;
#42355 = CARTESIAN_POINT ( 'NONE',  ( 759.9864689768902508, -2.089148112965993231, 354.9819416627836404 ) ) ;
#42356 = CARTESIAN_POINT ( 'NONE',  ( 804.6798772138708955, -87.72551174932937101, -334.6312213355107019 ) ) ;
#42357 = VECTOR ( 'NONE', #11317, 1000.000000000000000 ) ;
#42358 = CARTESIAN_POINT ( 'NONE',  ( 799.9636004259356241, -262.9181544815162965, 311.2241431872006956 ) ) ;
#42359 = CARTESIAN_POINT ( 'NONE',  ( 800.1688906516307043, -202.1692326535051905, -369.0717654672308186 ) ) ;
#42360 = CARTESIAN_POINT ( 'NONE',  ( 811.0346526505616112, -206.6346026584198512, 323.0537975583477532 ) ) ;
#42361 = CARTESIAN_POINT ( 'NONE',  ( 786.2694204179717872, 2.718209154846545683, -305.1769319972829067 ) ) ;
#42362 = CARTESIAN_POINT ( 'NONE',  ( 831.1634899080286232, 259.9999999999998863, -202.7499999999998295 ) ) ;
#42363 = CIRCLE ( 'NONE', #21720, 8.000000000000007105 ) ;
#42364 = CARTESIAN_POINT ( 'NONE',  ( 788.8264449731200330, -285.1800572038740711, 363.6646147819171233 ) ) ;
#42365 = CARTESIAN_POINT ( 'NONE',  ( 776.9254006560222479, -92.19088175424406018, 314.8983024940802125 ) ) ;
#42366 = CARTESIAN_POINT ( 'NONE',  ( 804.9363028652555840, -448.2709662947827951, -338.2165204200192079 ) ) ;
#42367 = FACE_OUTER_BOUND ( 'NONE', #36141, .T. ) ;
#42368 = DIRECTION ( 'NONE',  ( 1.000000000000000000, 0.000000000000000000, 0.000000000000000000 ) ) ;
#42370 = CARTESIAN_POINT ( 'NONE',  ( 788.7366044899766848, -347.9073299311467053, 316.5762568750059813 ) ) ;
#42369 = CARTESIAN_POINT ( 'NONE',  ( 800.7704444035546203, -124.1692326535054463, 326.0291762391768771 ) ) ;
#42371 = VERTEX_POINT ( 'NONE', #16330 ) ;
#42372 = CARTESIAN_POINT ( 'NONE',  ( 799.4546378042377910, -297.0783235625957559, -356.1575198192848006 ) ) ;
#42373 = CARTESIAN_POINT ( 'NONE',  ( 758.0580252608178853, -78.45278447660211896, 328.0187753319985404 ) ) ;
#42374 = CARTESIAN_POINT ( 'NONE',  ( 755.8990559732751535, -395.4636090269705164, 365.9055244015606831 ) ) ;
#42375 = CIRCLE ( 'NONE', #2540, 2.749999999999863665 ) ;
#42376 = CARTESIAN_POINT ( 'NONE',  ( 788.7631598425961101, -289.4419599262321299, -305.7194118038759143 ) ) ;
#42377 = FACE_BOUND ( 'NONE', #5085, .T. ) ;
#42378 = CARTESIAN_POINT ( 'NONE',  ( 766.5853460496234675, -421.9874144716863498, 372.3518521366060554 ) ) ;
#42379 = ORIENTED_EDGE ( 'NONE', *, *, #2366, .T. ) ;
#42380 = CARTESIAN_POINT ( 'NONE',  ( 791.9812246680005501, -332.6346026584195101, 361.9419747391813189 ) ) ;
#42381 = CARTESIAN_POINT ( 'NONE',  ( 801.3366627262608972, -56.53286901714201917, -353.0897708529566899 ) ) ;
#42382 = CARTESIAN_POINT ( 'NONE',  ( 771.2633955100217236, -167.9073299311473022, -363.4237431249939618 ) ) ;
#42383 = CARTESIAN_POINT ( 'NONE',  ( 771.2633955100217236, -215.9073299311471317, -363.4237431249939618 ) ) ;
#42384 = CARTESIAN_POINT ( 'NONE',  ( 797.6776695296629214, -403.5436935675101608, 357.6776695296636603 ) ) ;
#42385 = CARTESIAN_POINT ( 'NONE',  ( 815.2698199232961542, -160.8164208402382371, -342.5225473063383106 ) ) ;
#42386 = CARTESIAN_POINT ( 'NONE',  ( 797.8594530101009923, -133.5436935675110419, -322.1405469898982119 ) ) ;
#42387 = VERTEX_POINT ( 'NONE', #30412 ) ;
#42388 = CARTESIAN_POINT ( 'NONE',  ( 763.0428371773158460, -395.4636090269705164, -358.7617431975195359 ) ) ;
#42389 = CIRCLE ( 'NONE', #26878, 8.024999999999948841 ) ;
#42391 = CARTESIAN_POINT ( 'NONE',  ( 804.6971507214547046, -435.2817908451521021, 344.0799538623459739 ) ) ;
#42390 = CARTESIAN_POINT ( 'NONE',  ( 758.0580252608178853, -126.4527844766019626, 328.0187753319985404 ) ) ;
#42392 = CARTESIAN_POINT ( 'NONE',  ( 801.3366627262608972, -128.5328690171417634, 353.0897708529566899 ) ) ;
#42395 = CARTESIAN_POINT ( 'NONE',  ( 815.0009284576459549, -390.3510508353227237, 338.7629533639073429 ) ) ;
#42394 = FACE_OUTER_BOUND ( 'NONE', #16123, .T. ) ;
#42393 = DIRECTION ( 'NONE',  ( 0.000000000000000000, 0.000000000000000000, 1.000000000000000000 ) ) ;
#42396 = VECTOR ( 'NONE', #26679, 1000.000000000000000 ) ;
#42397 = ORIENTED_EDGE ( 'NONE', *, *, #28049, .T. ) ;
#42398 = CARTESIAN_POINT ( 'NONE',  ( 800.9840315886518738, -388.9181544815158986, -354.1144889064786412 ) ) ;
#42399 = CARTESIAN_POINT ( 'NONE',  ( 755.0636971347428243, -364.2709662947830793, -341.7834795799807353 ) ) ;
#42400 = CARTESIAN_POINT ( 'NONE',  ( 815.3608509340175488, -170.7363362996983938, -341.2497674668889545 ) ) ;
#42401 = CARTESIAN_POINT ( 'NONE',  ( 754.3581564841646241, -17.46360902697157513, 316.1443688327762516 ) ) ;
#42403 = FACE_OUTER_BOUND ( 'NONE', #2573, .T. ) ;
#42402 = CARTESIAN_POINT ( 'NONE',  ( 187.1337867209877857, -190.2822455671962985, 69.00746428064726956 ) ) ;
#42404 = CARTESIAN_POINT ( 'NONE',  ( 802.1676090361156639, -446.6346026584189985, -327.8955696845344505 ) ) ;
#42405 = CARTESIAN_POINT ( 'NONE',  ( 745.5313806188320314, -159.2817908451529547, -333.7943932421247268 ) ) ;
#42406 = DIRECTION ( 'NONE',  ( 0.000000000000000000, -0.000000000000000000, -1.000000000000000000 ) ) ;
#42407 = CARTESIAN_POINT ( 'NONE',  ( 773.4999999999993179, -544.8427095258973623, -350.0000000000000000 ) ) ;
#42408 = CARTESIAN_POINT ( 'NONE',  ( 787.5531968255692163, -357.8272453906068904, 316.1348686366205811 ) ) ;
#42409 = AXIS2_PLACEMENT_3D ( 'NONE', #26613, #43948, #2138 ) ;
#42410 = CARTESIAN_POINT ( 'NONE',  ( 768.9521613784389729, -321.8272453906070609, 373.2346286133773106 ) ) ;
#42411 = AXIS2_PLACEMENT_3D ( 'NONE', #20544, #9695, #34854 ) ;
#42412 = CARTESIAN_POINT ( 'NONE',  ( 754.9967657858570647, -193.5436935675108714, -365.0032342141425943 ) ) ;
#42413 = DIRECTION ( 'NONE',  ( 1.000000000000000000, -0.000000000000000000, -0.000000000000000000 ) ) ;
#42414 = CARTESIAN_POINT ( 'NONE',  ( 771.1735550268778070, 14.81994279612486309, -316.3353852180827630 ) ) ;
#42415 = AXIS2_PLACEMENT_3D ( 'NONE', #39302, #25667, #39780 ) ;
#42416 = CARTESIAN_POINT ( 'NONE',  ( 746.4236121716829757, -159.8272453906075157, 328.8385539511384650 ) ) ;
#42417 = CARTESIAN_POINT ( 'NONE',  ( 744.9990715423526808, -114.3510508353236617, -341.2370466360926002 ) ) ;
#42418 = CARTESIAN_POINT ( 'NONE',  ( 782.4968714119720516, -106.8164208402383935, 305.0891759886411023 ) ) ;
#42419 = CARTESIAN_POINT ( 'NONE',  ( 800.9747183278959710, -324.9982390220559409, -311.9810565676471583 ) ) ;
#42420 = EDGE_CURVE ( 'NONE', #37557, #26190, #44507, .T. ) ;
#42421 = DIRECTION ( 'NONE',  ( 0.000000000000000000, 0.7071067811865526798, 0.7071067811865423547 ) ) ;
#42422 = DIRECTION ( 'NONE',  ( -0.000000000000000000, 1.000000000000000000, -0.000000000000000000 ) ) ;
#42423 = CARTESIAN_POINT ( 'NONE',  ( 778.1981804954714335, -202.2709662947834772, 314.8072714833589885 ) ) ;
#42424 = CARTESIAN_POINT ( 'NONE',  ( 801.5560724626406000, -0.5545181178807169209, 326.7756240680316182 ) ) ;
#42425 = CARTESIAN_POINT ( 'NONE',  ( 744.8212110874229666, -426.8965053807771142, -336.2046728542121627 ) ) ;
#42426 = CIRCLE ( 'NONE', #13678, 6.118999999999985562 ) ;
#42427 = CARTESIAN_POINT ( 'NONE',  ( 763.0537975583475827, -432.4527844766008684, -371.0346526505627480 ) ) ;
#42428 = DIRECTION ( 'NONE',  ( 1.000000000000000000, 0.000000000000000000, 0.000000000000000000 ) ) ;
#42429 = CARTESIAN_POINT ( 'NONE',  ( 813.9316612368132837, 16.55804007376685050, 348.6739635108323228 ) ) ;
#42430 = EDGE_LOOP ( 'NONE', ( #27794, #9561 ) ) ;
#42431 = EDGE_CURVE ( 'NONE', #43930, #14210, #9407, .T. ) ;
#42432 = VECTOR ( 'NONE', #3805, 1000.000000000000000 ) ;
#42433 = CARTESIAN_POINT ( 'NONE',  ( 803.8556311672234642, -177.6237781080507148, -365.6418435158340117 ) ) ;
#42434 = SURFACE_STYLE_FILL_AREA ( #7114 ) ;
#42435 = CARTESIAN_POINT ( 'NONE',  ( 795.6651683502461765, -298.7146871989593251, 371.3240766477733814 ) ) ;
#42436 = CARTESIAN_POINT ( 'NONE',  ( 788.7366044899766848, -131.9073299311473875, 316.5762568750059813 ) ) ;
#42437 = ORIENTED_EDGE ( 'NONE', *, *, #3789, .T. ) ;
#42438 = CARTESIAN_POINT ( 'NONE',  ( 759.9864689768902508, -146.0891481129655176, -354.9819416627836404 ) ) ;
#42439 = CARTESIAN_POINT ( 'NONE',  ( 778.2165204200184689, -286.8164208402378677, 364.9363028652563230 ) ) ;
#42440 = CARTESIAN_POINT ( 'NONE',  ( 749.2812353651451076, -30.45278447660226817, -323.2262854647983090 ) ) ;
#42441 = CARTESIAN_POINT ( 'NONE',  ( 801.1904061080338124, -92.08914811296570235, 368.3070685750236066 ) ) ;
#42442 = VECTOR ( 'NONE', #7382, 1000.000000000000114 ) ;
#42443 = EDGE_LOOP ( 'NONE', ( #39861, #13439, #36605, #357, #17040, #28841 ) ) ;
#42444 = CARTESIAN_POINT ( 'NONE',  ( 813.5763878283155464, -459.8272453906066062, -351.1614460488615350 ) ) ;
#42445 = AXIS2_PLACEMENT_3D ( 'NONE', #30868, #35005, #38478 ) ;
#42446 = ORIENTED_EDGE ( 'NONE', *, *, #28109, .T. ) ;
#42447 = APPLICATION_PROTOCOL_DEFINITION ( 'draft international standard', 'automotive_design', 1998, #14295 ) ;
#42448 = EDGE_CURVE ( 'NONE', #39697, #7984, #23036, .T. ) ;
#42449 = CARTESIAN_POINT ( 'NONE',  ( 797.8594530101008786, -13.54369356751140785, 322.1405469898980982 ) ) ;
#42450 = CARTESIAN_POINT ( 'NONE',  ( 794.9819416627830151, -300.9982390220559409, -319.9864689768909898 ) ) ;
#42451 = CIRCLE ( 'NONE', #29921, 2.749999999999919176 ) ;
#42453 = CARTESIAN_POINT ( 'NONE',  ( 815.0009284576459549, -294.3510508353230648, 338.7629533639073429 ) ) ;
#42452 = CARTESIAN_POINT ( 'NONE',  ( 745.0891759886404770, -388.2709662947829656, 342.4968714119734159 ) ) ;
#42454 = CARTESIAN_POINT ( 'NONE',  ( 781.2497674668890113, -84.35105083532374692, 375.3608509340180603 ) ) ;
#42455 = EDGE_CURVE ( 'NONE', #39212, #2677, #20118, .T. ) ;
#42456 = CARTESIAN_POINT ( 'NONE',  ( 801.5560724626406000, -288.5545181178798657, -326.7756240680316182 ) ) ;
#42457 = CARTESIAN_POINT ( 'NONE',  ( 781.8018195045266339, -238.2709662947833920, -365.1927285166406705 ) ) ;
#42458 = CARTESIAN_POINT ( 'NONE',  ( 771.1735550268780344, -441.1800572038736163, -316.3353852180828198 ) ) ;
#42459 = CARTESIAN_POINT ( 'NONE',  ( 756.3353852180819104, -125.9073299311474159, -331.1735550268788302 ) ) ;
#42460 = CARTESIAN_POINT ( 'NONE',  ( 1238.921997096861332, 430.0000000000002842, -320.0000000000000568 ) ) ;
#42461 = ORIENTED_EDGE ( 'NONE', *, *, #1788, .T. ) ;
#42462 = COLOUR_RGB ( '',0.7921568627450980005, 0.8196078431372548767, 0.9333333333333333481 ) ;
#42464 = CARTESIAN_POINT ( 'NONE',  ( 759.9999999999992042, -462.9681489794448339, 370.0000000000000568 ) ) ;
#42463 = PLANE ( 'NONE',  #44750 ) ;
#42465 = CARTESIAN_POINT ( 'NONE',  ( 757.7880784355613741, -42.00906357242603661, -312.4576283171834916 ) ) ;
#42466 = CARTESIAN_POINT ( 'NONE',  ( 115.7583438952258774, -600.0000000000000000, -244.9999999999999716 ) ) ;
#42467 = CARTESIAN_POINT ( 'NONE',  ( -26.63011601220122060, -513.1383975375929367, -369.9999999999999432 ) ) ;
#42468 = CIRCLE ( 'NONE', #28450, 30.00000000000008171 ) ;
#42469 = CARTESIAN_POINT ( 'NONE',  ( 755.1538015810308480, -254.1908817542435770, 343.0433043558613804 ) ) ;
#42470 = CARTESIAN_POINT ( 'NONE',  ( 755.3201227861273992, -123.7255117493292147, 345.3687786644892981 ) ) ;
#42471 = ORIENTED_EDGE ( 'NONE', *, *, #45593, .T. ) ;
#42472 = CARTESIAN_POINT ( 'NONE',  ( 802.9823548866075953, -1.099972663335260226, -330.0799878456151077 ) ) ;
#42473 = CARTESIAN_POINT ( 'NONE',  ( 814.5518280994195948, -87.72551174932935680, -332.4837098697145166 ) ) ;
#42474 = CARTESIAN_POINT ( 'NONE',  ( 754.9735926884551418, -306.3510508353230648, 340.5236548041000333 ) ) ;
#42475 = CARTESIAN_POINT ( 'NONE',  ( 879.9999999999990905, 469.9999999999998863, 210.0000000000000000 ) ) ;
#42476 = ADVANCED_FACE ( 'NONE', ( #612 ), #35019, .F. ) ;
#42477 = CARTESIAN_POINT ( 'NONE',  ( 802.2119215644370342, -54.00906357242601530, 367.5423716828165084 ) ) ;
#42478 = CARTESIAN_POINT ( 'NONE',  ( 744.7301800767019131, -244.8164208402378961, -337.4774526936615757 ) ) ;
#42479 = EDGE_CURVE ( 'NONE', #5495, #9195, #11234, .T. ) ;
#42480 = CARTESIAN_POINT ( 'NONE',  ( 804.7487373415286811, -187.5436935675108430, 364.7487373415288516 ) ) ;
#42481 = CARTESIAN_POINT ( 'NONE',  ( 788.8264449731200330, -69.18005720387488111, 363.6646147819171233 ) ) ;
#42482 = DIRECTION ( 'NONE',  ( 0.000000000000000000, 0.000000000000000000, -1.000000000000000000 ) ) ;
#42483 = CARTESIAN_POINT ( 'NONE',  ( 793.4146539503750546, -289.9874144716866908, -307.6481478633938877 ) ) ;
#42484 = AXIS2_PLACEMENT_3D ( 'NONE', #30339, #11893, #15803 ) ;
#42485 = CARTESIAN_POINT ( 'NONE',  ( 807.2620300519052989, -456.0090635724247932, 318.0141637701419768 ) ) ;
#42486 = CARTESIAN_POINT ( 'NONE',  ( 763.0537975583475827, -312.4527844766012663, -371.0346526505627480 ) ) ;
#42487 = CARTESIAN_POINT ( 'NONE',  ( 927.9999999999990905, 219.9999999999998863, 360.0000000000000000 ) ) ;
#42488 = CARTESIAN_POINT ( 'NONE',  ( 772.3691319403857278, -359.2601417444137724, 315.8894580844506663 ) ) ;
#42489 = VECTOR ( 'NONE', #16445, 1000.000000000000000 ) ;
#42490 = CARTESIAN_POINT ( 'NONE',  ( 810.7187646348534145, -42.45278447660223264, 356.7737145352016341 ) ) ;
#42491 = CARTESIAN_POINT ( 'NONE',  ( 802.1676090361156639, -398.6346026584193396, -327.8955696845344505 ) ) ;
#42492 = EDGE_CURVE ( 'NONE', #23058, #32406, #5367, .T. ) ;
#42493 = CARTESIAN_POINT ( 'NONE',  ( 756.1348686366196716, -41.26014174441479554, 347.5531968255698416 ) ) ;
#42494 = CARTESIAN_POINT ( 'NONE',  ( 773.7943932421234194, -71.80559628986922860, -305.5313806188329409 ) ) ;
#42495 = CARTESIAN_POINT ( 'NONE',  ( 805.9055244015594326, -219.6237781080506295, 315.8990559732753240 ) ) ;
#42496 = CARTESIAN_POINT ( 'NONE',  ( 792.1044303154646968, -12.45278447660232324, 317.8323909638837677 ) ) ;
#42497 = VECTOR ( 'NONE', #26977, 1000.000000000000114 ) ;
#42498 = ORIENTED_EDGE ( 'NONE', *, *, #45245, .F. ) ;
#42499 = CARTESIAN_POINT ( 'NONE',  ( 789.9200121543843807, -217.9874144716870035, -317.0176451133914384 ) ) ;
#42500 = CARTESIAN_POINT ( 'NONE',  ( 759.9864689768902508, -194.0891481129654039, 354.9819416627836404 ) ) ;
#42501 = VECTOR ( 'NONE', #20175, 1000.000000000000000 ) ;
#42502 = PRODUCT_DEFINITION_SHAPE ( 'NONE', 'NONE',  #28146 ) ;
#42503 = CARTESIAN_POINT ( 'NONE',  ( 793.4146539503750546, -49.98741447168749374, -307.6481478633938877 ) ) ;
#42504 = CARTESIAN_POINT ( 'NONE',  ( 804.9363028652555840, -328.2709662947831362, 338.2165204200192079 ) ) ;
#42505 = CARTESIAN_POINT ( 'NONE',  ( 792.6815175455323015, -452.9681489794447202, -361.6124358662449367 ) ) ;
#42506 = CARTESIAN_POINT ( 'NONE',  ( 779.9999999999992042, -452.9681489794448339, 339.9999999999999432 ) ) ;
#42507 = VERTEX_POINT ( 'NONE', #18178 ) ;
#42508 = CARTESIAN_POINT ( 'NONE',  ( 805.1016975059191054, -54.89650538077837183, 343.0745993439771837 ) ) ;
#42509 = CARTESIAN_POINT ( 'NONE',  ( 766.4474001241216001, -355.0999726633341993, -307.3154664389482491 ) ) ;
#42510 = EDGE_CURVE ( 'NONE', #17206, #12447, #28224, .T. ) ;
#42511 = CARTESIAN_POINT ( 'NONE',  ( 744.7301800767020268, -268.8164208402378677, 337.4774526936615189 ) ) ;
#42512 = CARTESIAN_POINT ( 'NONE',  ( 812.6845335610512393, -7.987414471687621642, 353.5525998758768651 ) ) ;
#42513 = CARTESIAN_POINT ( 'NONE',  ( 775.8780910478218402, -153.2817908451529831, -364.9511171171680530 ) ) ;
#42514 = CARTESIAN_POINT ( 'NONE',  ( 771.2633955100217236, -143.9073299311473590, -363.4237431249939618 ) ) ;
#42515 = CARTESIAN_POINT ( 'NONE',  ( 768.0187753319979720, -344.6346026584195101, -318.0580252608186242 ) ) ;
#42516 = ORIENTED_EDGE ( 'NONE', *, *, #30332, .T. ) ;
#42517 = VECTOR ( 'NONE', #22446, 1000.000000000000000 ) ;
#42518 = CARTESIAN_POINT ( 'NONE',  ( 813.1304606946830518, -281.9073299311468759, 352.3570229623690580 ) ) ;
#42519 = CYLINDRICAL_SURFACE ( 'NONE', #38085, 12.00000000000001066 ) ;
#42520 = CARTESIAN_POINT ( 'NONE',  ( 793.2243759319678702, -338.5328690171411381, 318.4439275373583200 ) ) ;
#42521 = AXIS2_PLACEMENT_3D ( 'NONE', #24790, #548, #28491 ) ;
#42522 = FACE_OUTER_BOUND ( 'NONE', #26179, .T. ) ;
#42523 = CARTESIAN_POINT ( 'NONE',  ( 759.0159684113467620, -160.9181544815165807, 325.8855110935213020 ) ) ;
#42524 = CARTESIAN_POINT ( 'NONE',  ( 762.3223304703356007, -7.543693567511430942, 322.3223304703362828 ) ) ;
#42525 = ORIENTED_EDGE ( 'NONE', *, *, #39431, .T. ) ;
#42526 = CARTESIAN_POINT ( 'NONE',  ( 755.8990559732751535, -395.4636090269705164, -365.9055244015606831 ) ) ;
#42527 = CARTESIAN_POINT ( 'NONE',  ( 777.4774526936600978, 13.72903370521577315, -304.7301800767028226 ) ) ;
#42528 = CARTESIAN_POINT ( 'NONE',  ( 783.0745993439762742, -224.1908817542436623, 365.1016975059196739 ) ) ;
#42529 = CARTESIAN_POINT ( 'NONE',  ( 788.6739635108323228, -223.6454272087891013, 373.9316612368139090 ) ) ;
#42530 = CARTESIAN_POINT ( 'NONE',  ( 796.7845633553578182, -201.6237781080506863, 358.5707757039688204 ) ) ;
#42531 = CARTESIAN_POINT ( 'NONE',  ( 795.1360043628807261, -356.0891481129647218, -360.2193346964456282 ) ) ;
#42532 = ADVANCED_FACE ( 'NONE', ( #28560, #41973 ), #42867, .F. ) ;
#42533 = CARTESIAN_POINT ( 'NONE',  ( 800.2193346964447755, 5.001760977943074948, 355.1360043628815788 ) ) ;
#42534 = DIRECTION ( 'NONE',  ( 0.000000000000000000, 0.000000000000000000, -1.000000000000000000 ) ) ;
#42535 = CARTESIAN_POINT ( 'NONE',  ( 799.2566176426618085, -216.0090635724255037, -324.0069404352559559 ) ) ;
#42536 = AXIS2_PLACEMENT_3D ( 'NONE', #24163, #23920, #13326 ) ;
#42537 = EDGE_CURVE ( 'NONE', #13600, #25447, #14481, .T. ) ;
#42538 = CARTESIAN_POINT ( 'NONE',  ( 808.3070685750230950, -18.99823902205683979, 361.1904061080339261 ) ) ;
#42539 = CARTESIAN_POINT ( 'NONE',  ( 796.9462024416508257, -84.45278447660206211, 308.9653473494370246 ) ) ;
#42540 = CARTESIAN_POINT ( 'NONE',  ( 919.9999999999993179, 154.9999999999998863, -360.0000000000000000 ) ) ;
#42541 = CARTESIAN_POINT ( 'NONE',  ( 804.7487373415286811, -427.5436935675101040, -364.7487373415288516 ) ) ;
#42542 = DIRECTION ( 'NONE',  ( -1.000000000000000000, 0.000000000000000000, 0.000000000000000000 ) ) ;
#42543 = CARTESIAN_POINT ( 'NONE',  ( 795.8262568251477660, -358.3726999360613945, 308.3538107759623585 ) ) ;
#42544 = DIRECTION ( 'NONE',  ( 0.000000000000000000, 0.000000000000000000, -1.000000000000000000 ) ) ;
#42545 = CARTESIAN_POINT ( 'NONE',  ( 782.4968714119720516, -322.8164208402377540, 305.0891759886411023 ) ) ;
#42546 = CARTESIAN_POINT ( 'NONE',  ( 792.3570229623688874, -45.18005720387493085, -373.1304606946836202 ) ) ;
#42547 = EDGE_CURVE ( 'NONE', #45022, #6383, #20923, .T. ) ;
#42548 = CARTESIAN_POINT ( 'NONE',  ( 778.1981804954714335, -274.2709662947833067, -314.8072714833589885 ) ) ;
#42549 = DIRECTION ( 'NONE',  ( 1.644774851296528363E-16, -1.000000000000000000, 0.000000000000000000 ) ) ;
#42550 = PRODUCT_DEFINITION ( 'UNKNOWN', '', #9073, #31185 ) ;
#42551 = CARTESIAN_POINT ( 'NONE',  ( 755.3201227861273992, -435.7255117493282341, 345.3687786644892981 ) ) ;
#42552 = CARTESIAN_POINT ( 'NONE',  ( 769.0155153010367712, -178.3726999360619629, 362.7791456095907279 ) ) ;
#42553 = CARTESIAN_POINT ( 'NONE',  ( 813.5763878283155464, -75.82724539060775726, -351.1614460488615350 ) ) ;
#42554 = CARTESIAN_POINT ( 'NONE',  ( 804.9511171171677688, -77.80559628986920018, -335.8780910478229202 ) ) ;
#42555 = CARTESIAN_POINT ( 'NONE',  ( 744.9990715423526808, -90.35105083532373271, 341.2370466360926002 ) ) ;
#42556 = CARTESIAN_POINT ( 'NONE',  ( 792.1044303154646968, -420.4527844766009821, 317.8323909638837677 ) ) ;
#42557 = CARTESIAN_POINT ( 'NONE',  ( 788.8264449731200330, 2.819942796124898177, -363.6646147819171233 ) ) ;
#42559 = VERTEX_POINT ( 'NONE', #13799 ) ;
#42558 = CARTESIAN_POINT ( 'NONE',  ( 804.1601925771018387, -103.4419599262327836, -346.5483106153029098 ) ) ;
#42560 = CARTESIAN_POINT ( 'NONE',  ( 800.2193346964447755, -114.9982390220565236, -355.1360043628815788 ) ) ;
#42561 = VECTOR ( 'NONE', #42917, 1000.000000000000114 ) ;
#42562 = CARTESIAN_POINT ( 'NONE',  ( 779.4709603349208464, -408.3510508353227806, -314.7162404726379918 ) ) ;
#42564 = CARTESIAN_POINT ( 'NONE',  ( 785.3141322388236176, -237.7255117493289163, 364.4286716492789537 ) ) ;
#42563 = CARTESIAN_POINT ( 'NONE',  ( 764.8639956371174549, -224.0891481129653187, 319.7806653035542013 ) ) ;
#42565 = AXIS2_PLACEMENT_3D ( 'NONE', #35519, #44852, #16674 ) ;
#42566 = ORIENTED_EDGE ( 'NONE', *, *, #7470, .F. ) ;
#42567 = CARTESIAN_POINT ( 'NONE',  ( 805.9055244015594326, -411.6237781080499758, -315.8990559732753240 ) ) ;
#42568 = CARTESIAN_POINT ( 'NONE',  ( -728.8365100919714905, 256.5000000000001705, -199.9999999999890861 ) ) ;
#42569 = ORIENTED_EDGE ( 'NONE', *, *, #38186, .T. ) ;
#42570 = CARTESIAN_POINT ( 'NONE',  ( 755.0636971347428243, -412.2709662947829088, 341.7834795799807353 ) ) ;
#42571 = ORIENTED_EDGE ( 'NONE', *, *, #25287, .F. ) ;
#42572 = ORIENTED_EDGE ( 'NONE', *, *, #14023, .F. ) ;
#42573 = VECTOR ( 'NONE', #5877, 1000.000000000000114 ) ;
#42574 = CARTESIAN_POINT ( 'NONE',  ( 792.3570229623688874, -237.1800572038742985, -373.1304606946836202 ) ) ;
#42575 = CARTESIAN_POINT ( 'NONE',  ( 782.5225473063383106, -166.2709662947836478, 375.2698199232970637 ) ) ;
#42576 = CARTESIAN_POINT ( 'NONE',  ( 802.5472867521000353, -268.3726999360616787, 350.8726784830461156 ) ) ;
#42577 = ORIENTED_EDGE ( 'NONE', *, *, #16352, .T. ) ;
#42578 = CARTESIAN_POINT ( 'NONE',  ( 801.9858362298568863, -195.0783235625961538, 312.7379699480935642 ) ) ;
#42579 = CARTESIAN_POINT ( 'NONE',  ( 804.4286716492782716, -257.3618753856924286, -345.3141322388244703 ) ) ;
#42580 = ORIENTED_EDGE ( 'NONE', *, *, #24391, .F. ) ;
#42581 = CARTESIAN_POINT ( 'NONE',  ( 792.1044303154645831, -348.4527844766012663, -317.8323909638837677 ) ) ;
#42582 = CARTESIAN_POINT ( 'NONE',  ( 768.0187753319979720, -8.634602658420517329, -318.0580252608186242 ) ) ;
#42583 = CARTESIAN_POINT ( 'NONE',  ( 758.6633372737375112, -236.5328690171414792, 326.9102291470432533 ) ) ;
#42584 = DIRECTION ( 'NONE',  ( -0.000000000000000000, -0.000000000000000000, -1.000000000000000000 ) ) ;
#42585 = DIRECTION ( 'NONE',  ( -1.000000000000000000, -0.000000000000000000, -0.000000000000000000 ) ) ;
#42586 = ORIENTED_EDGE ( 'NONE', *, *, #41968, .T. ) ;
#42587 = CARTESIAN_POINT ( 'NONE',  ( 756.3353852180819104, -29.90732993114771787, -331.1735550268788302 ) ) ;
#42588 = CARTESIAN_POINT ( 'NONE',  ( 831.1634899080286232, 239.9999999999999147, -199.9999999999999432 ) ) ;
#42589 = FACE_BOUND ( 'NONE', #41891, .T. ) ;
#42590 = ORIENTED_EDGE ( 'NONE', *, *, #1301, .T. ) ;
#42591 = CARTESIAN_POINT ( 'NONE',  ( 802.2119215644370342, -270.0090635724253048, -367.5423716828165084 ) ) ;
#42592 = CIRCLE ( 'NONE', #30775, 2.749999999999919176 ) ;
#42594 = CARTESIAN_POINT ( 'NONE',  ( 797.6776695296629214, -259.5436935675106156, -357.6776695296636603 ) ) ;
#42593 = DIRECTION ( 'NONE',  ( 1.000000000000000000, -0.000000000000000000, -0.000000000000000000 ) ) ;
#42595 = CARTESIAN_POINT ( 'NONE',  ( 754.9735926884551418, -402.3510508353228374, -340.5236548041000333 ) ) ;
#42596 = DIRECTION ( 'NONE',  ( 0.000000000000000000, -1.000000000000000000, 0.000000000000000000 ) ) ;
#42597 = CARTESIAN_POINT ( 'NONE',  ( 769.0155153010367712, -130.3726999360621619, -362.7791456095907279 ) ) ;
#42598 = VECTOR ( 'NONE', #35018, 1000.000000000000000 ) ;
#42599 = CARTESIAN_POINT ( 'NONE',  ( 989.9999999999992042, 240.0000000000001990, -201.9999999999999716 ) ) ;
#42600 = CARTESIAN_POINT ( 'NONE',  ( 795.6651683502461765, 13.28531280103958423, -371.3240766477733814 ) ) ;
#42601 = CARTESIAN_POINT ( 'NONE',  ( 754.9967657858570647, -313.5436935675103882, -365.0032342141425943 ) ) ;
#42602 = DIRECTION ( 'NONE',  ( 0.000000000000000000, 1.000000000000000000, 0.000000000000000000 ) ) ;
#42603 = CARTESIAN_POINT ( 'NONE',  ( 781.8018195045266339, -22.27096629478410250, 365.1927285166406705 ) ) ;
#42604 = CONICAL_SURFACE ( 'NONE', #44064, 8.024999999999948841, 0.7853981633963380560 ) ;
#42605 = CARTESIAN_POINT ( 'NONE',  ( 764.1737431748507561, -250.3726999360618208, 371.6461892240376415 ) ) ;
#42606 = CARTESIAN_POINT ( 'NONE',  ( 759.8311093483677041, -190.1692326535052189, -310.9282345327691814 ) ) ;
#42607 = CARTESIAN_POINT ( 'NONE',  ( 744.7301800767019131, -220.8164208402379529, 337.4774526936615757 ) ) ;
#42608 = CARTESIAN_POINT ( 'NONE',  ( 763.2262854647970016, -440.6346026584191122, -309.2812353651462445 ) ) ;
#42609 = CARTESIAN_POINT ( 'NONE',  ( -598.8365100919716042, 260.0000000000001705, -197.2499999999901092 ) ) ;
#42610 = CARTESIAN_POINT ( 'NONE',  ( 755.5713283507202505, -341.3618753856922012, 334.6858677611754729 ) ) ;
#42611 = CARTESIAN_POINT ( 'NONE',  ( 769.9779781133707957, -91.09997266333496668, 316.7813123517150871 ) ) ;
#42612 = CARTESIAN_POINT ( 'NONE',  ( 755.1538015810308480, -86.19088175424408860, 343.0433043558613804 ) ) ;
#42613 = CARTESIAN_POINT ( 'NONE',  ( 756.7813123517142913, 4.012585528312341054, -329.9779781133712504 ) ) ;
#42614 = FACE_OUTER_BOUND ( 'NONE', #8598, .T. ) ;
#42615 = CARTESIAN_POINT ( 'NONE',  ( 786.4999999999993179, 26.27639943461401018, 900.0000000000001137 ) ) ;
#42617 = CARTESIAN_POINT ( 'NONE',  ( 778.2165204200184689, -358.8164208402375834, 364.9363028652563230 ) ) ;
#42616 = CARTESIAN_POINT ( 'NONE',  ( 763.2154366446407039, -141.6237781080508569, 321.4292242960311228 ) ) ;
#42618 = ORIENTED_EDGE ( 'NONE', *, *, #23553, .F. ) ;
#42619 = CARTESIAN_POINT ( 'NONE',  ( 789.9200121543843807, -289.9874144716866908, -317.0176451133914384 ) ) ;
#42620 = CARTESIAN_POINT ( 'NONE',  ( 803.4237431249931660, -135.1800572038746679, 331.2633955100225194 ) ) ;
#42621 = CARTESIAN_POINT ( 'NONE',  ( 813.2346286133761168, -293.2601417444139429, -328.9521613784389160 ) ) ;
#42622 = CARTESIAN_POINT ( 'NONE',  ( -468.8365100919714337, 240.0000000000001421, -197.2499999999910187 ) ) ;
#42623 = CARTESIAN_POINT ( 'NONE',  ( 764.3348316497523456, -430.7146871989590409, 308.6759233522265617 ) ) ;
#42624 = ORIENTED_EDGE ( 'NONE', *, *, #18364, .F. ) ;
#42625 = CARTESIAN_POINT ( 'NONE',  ( 788.7366044899766848, -323.9073299311468190, 316.5762568750059813 ) ) ;
#42626 = CARTESIAN_POINT ( 'NONE',  ( 766.7756240680305382, -86.53286901714194812, -361.5560724626415663 ) ) ;
#42627 = CARTESIAN_POINT ( 'NONE',  ( 755.0636971347428243, -148.2709662947837330, -341.7834795799807353 ) ) ;
#42628 = CARTESIAN_POINT ( 'NONE',  ( 762.1405469898971887, -217.5436935675107293, -357.8594530101015607 ) ) ;
#42629 = CARTESIAN_POINT ( 'NONE',  ( 755.3201227861273992, -411.7255117493282910, 345.3687786644892981 ) ) ;
#42630 = CARTESIAN_POINT ( 'NONE',  ( 810.7187646348534145, -162.4527844766018632, -356.7737145352016341 ) ) ;
#42631 = ORIENTED_EDGE ( 'NONE', *, *, #6342, .T. ) ;
#42632 = CARTESIAN_POINT ( 'NONE',  ( 759.7806653035535192, -150.9982390220564241, -324.8639956371181370 ) ) ;
#42633 = VERTEX_POINT ( 'NONE', #35702 ) ;
#42634 = VECTOR ( 'NONE', #6535, 1000.000000000000000 ) ;
#42635 = CARTESIAN_POINT ( 'NONE',  ( 780.5236548040995785, -380.7363362996977116, -314.9735926884559944 ) ) ;
#42636 = CARTESIAN_POINT ( 'NONE',  ( 769.9779781133707957, -427.0999726633338582, 316.7813123517150871 ) ) ;
#42637 = CARTESIAN_POINT ( 'NONE',  ( 754.9735926884551418, -138.3510508353236048, 340.5236548041000333 ) ) ;
#42640 = CARTESIAN_POINT ( 'NONE',  ( 793.4146539503750546, -385.9874144716864066, 307.6481478633938877 ) ) ;
#42639 = PLANE ( 'NONE',  #5580 ) ;
#42638 = CYLINDRICAL_SURFACE ( 'NONE', #435, 10.00000000000000888 ) ;
#42641 = ORIENTED_EDGE ( 'NONE', *, *, #20155, .T. ) ;
#42642 = CARTESIAN_POINT ( 'NONE',  ( 757.4527132478984868, -400.3726999360612808, -329.1273215169538844 ) ) ;
#42643 = DIRECTION ( 'NONE',  ( 0.000000000000000000, 0.000000000000000000, -1.000000000000000000 ) ) ;
#42644 = CARTESIAN_POINT ( 'NONE',  ( 747.6481478633932056, -181.0999726633347109, -353.4146539503763620 ) ) ;
#42645 = CARTESIAN_POINT ( 'NONE',  ( 804.1009440267234822, -23.46360902697155026, 314.0944755984392600 ) ) ;
#42647 = DIRECTION ( 'NONE',  ( -0.000000000000000000, -0.000000000000000000, -1.000000000000000000 ) ) ;
#42646 = LINE ( 'NONE', #42861, #16756 ) ;
#42648 = LINE ( 'NONE', #31566, #37266 ) ;
#42649 = CARTESIAN_POINT ( 'NONE',  ( 786.2694204179717872, -189.2817908451528979, -305.1769319972829067 ) ) ;
#42650 = DIRECTION ( 'NONE',  ( 0.000000000000000000, 0.3826834323650836200, 0.9238795325112892920 ) ) ;
#42651 = DIRECTION ( 'NONE',  ( 1.000000000000000000, 0.000000000000000000, 0.000000000000000000 ) ) ;
#42652 = CARTESIAN_POINT ( 'NONE',  ( 804.8461984189677878, -362.1908817542432644, 336.9566956441385628 ) ) ;
#42653 = CARTESIAN_POINT ( 'NONE',  ( 745.1792804349281596, -350.1908817542433212, 343.7566961878542884 ) ) ;
#42654 = CARTESIAN_POINT ( 'NONE',  ( 751.9810565676468741, -218.0891481129653187, -360.9747183278973921 ) ) ;
#42655 = CARTESIAN_POINT ( 'NONE',  ( 1820.038553321469863, 240.0000000000001990, 201.9999999999999716 ) ) ;
#42656 = CARTESIAN_POINT ( 'NONE',  ( 788.7366044899766848, 12.09267006885214180, -316.5762568750059813 ) ) ;
#42657 = CARTESIAN_POINT ( 'NONE',  ( 773.7305795820266212, -129.2817908451530400, 374.8230680027170365 ) ) ;
#42658 = CARTESIAN_POINT ( 'NONE',  ( 747.3154664389472828, -91.98741447168737295, -326.4474001241230781 ) ) ;
#42659 = CARTESIAN_POINT ( 'NONE',  ( 814.9108240113580450, -112.2709662947838325, 337.5031285880265273 ) ) ;
#42660 = CARTESIAN_POINT ( 'NONE',  ( 814.5518280994195948, -327.7255117493285184, -332.4837098697145734 ) ) ;
#42661 = CARTESIAN_POINT ( 'NONE',  ( -208.8365100919714052, 260.0000000000001137, -191.9749999999926899 ) ) ;
#42662 = DIRECTION ( 'NONE',  ( -1.000000000000000000, 0.000000000000000000, 0.000000000000000000 ) ) ;
#42663 = CARTESIAN_POINT ( 'NONE',  ( 781.7834795799800531, -202.8164208402380950, 315.0636971347436202 ) ) ;
#42664 = CARTESIAN_POINT ( 'NONE',  ( 807.2620300519052989, -456.0090635724247932, 318.0141637701419768 ) ) ;
#42665 = CARTESIAN_POINT ( 'NONE',  ( 759.8311093483677041, -406.1692326535045368, -310.9282345327691814 ) ) ;
#42666 = VECTOR ( 'NONE', #14573, 1000.000000000000000 ) ;
#42667 = CARTESIAN_POINT ( 'NONE',  ( 758.8095938919642549, -416.0891481129645513, -311.6929314249763365 ) ) ;
#42668 = CARTESIAN_POINT ( 'NONE',  ( -786.4999999999993179, -544.8427095258973623, -350.0000000000000000 ) ) ;
#42669 = CARTESIAN_POINT ( 'NONE',  ( 812.6845335610512393, 16.01258552831230375, 353.5525998758768651 ) ) ;
#42670 = ORIENTED_EDGE ( 'NONE', *, *, #36816, .F. ) ;
#42671 = CARTESIAN_POINT ( 'NONE',  ( 766.5853460496234675, -181.9874144716870887, -372.3518521366060554 ) ) ;
#42672 = CARTESIAN_POINT ( 'NONE',  ( 781.2497674668890113, -324.3510508353229511, 375.3608509340180603 ) ) ;
#42673 = CARTESIAN_POINT ( 'NONE',  ( 794.9819416627830151, -156.9982390220564241, 319.9864689768909898 ) ) ;
#42674 = VERTEX_POINT ( 'NONE', #150 ) ;
#42675 = CARTESIAN_POINT ( 'NONE',  ( 768.0187753319979720, -320.6346026584195670, 318.0580252608186242 ) ) ;
#42676 = CARTESIAN_POINT ( 'NONE',  ( 744.7301800767019131, -28.81642084023863148, -337.4774526936615757 ) ) ;
#42677 = CARTESIAN_POINT ( 'NONE',  ( 755.2512626584698410, -79.54369356751119824, 315.2512626584710915 ) ) ;
#42678 = ORIENTED_EDGE ( 'NONE', *, *, #17953, .T. ) ;
#42679 = CARTESIAN_POINT ( 'NONE',  ( 815.3608509340175488, -434.7363362996975980, -341.2497674668889545 ) ) ;
#42680 = ORIENTED_EDGE ( 'NONE', *, *, #38536, .F. ) ;
#42681 = CARTESIAN_POINT ( 'NONE',  ( 781.7834795799800531, -10.81642084023869543, 315.0636971347436202 ) ) ;
#42683 = CARTESIAN_POINT ( 'NONE',  ( 812.6845335610512393, -271.9874144716868045, 353.5525998758768651 ) ) ;
#42682 = CARTESIAN_POINT ( 'NONE',  ( 772.5602148656447525, -393.7255117493283478, 305.7998596910095443 ) ) ;
#42684 = CARTESIAN_POINT ( 'NONE',  ( 791.1614460488616487, -59.26014174441473870, 373.5763878283158874 ) ) ;
#42685 = CARTESIAN_POINT ( 'NONE',  ( 772.4468031744293057, -273.8272453906071746, -363.8651313633793620 ) ) ;
#42686 = CARTESIAN_POINT ( 'NONE',  ( 762.1405469898971887, -289.5436935675103882, -357.8594530101015607 ) ) ;
#42687 = CARTESIAN_POINT ( 'NONE',  ( 754.8072714833583632, -436.8164208402372992, -338.1981804954721156 ) ) ;
#42688 = EDGE_CURVE ( 'NONE', #30209, #16040, #6863, .T. ) ;
#42689 = B_SPLINE_CURVE_WITH_KNOTS ( 'NONE', 3,
 ( #31669, #27516, #16914, #41618, #27980, #23590, #20591, #41397, #34686, #27303, #34908, #45554, #17599, #38385, #9974, #17135, #20809, #6278, #41857, #30993, #37921, #6968, #10201, #3273, #42075, #36, #21053, #24279, #30772, #17365, #13449, #13226, #24045, #6734, #6045, #45312 ),
 .UNSPECIFIED., .F., .F.,
 ( 4, 2, 2, 2, 2, 2, 2, 2, 2, 2, 2, 2, 2, 2, 2, 2, 2, 4 ),
 ( 0.0008252806733485880007, 0.001104729680136533072, 0.001384178686924478251, 0.001943076700500593040, 0.002501974714076708045, 0.003060872727652823484, 0.004178668754804788950, 0.005296464781956755283, 0.007532056836260687949, 0.009767648890564618880, 0.01423883299917248421, 0.01871001710778034607, 0.02094560916208429782, 0.02318120121638824610, 0.02765238532499614266, 0.02988797737930003542, 0.03212356943360392819, 0.03659475354221209537 ),
 .UNSPECIFIED. ) ;
#42690 = CIRCLE ( 'NONE', #25711, 20.00000000000001776 ) ;
#42691 = CARTESIAN_POINT ( 'NONE',  ( 792.3570229623688874, -381.1800572038737869, 373.1304606946836202 ) ) ;
#42693 = CARTESIAN_POINT ( 'NONE',  ( -338.8365100919713200, 240.0000000000001421, -202.7499999999916724 ) ) ;
#42692 = LINE ( 'NONE', #22124, #29992 ) ;
#42694 = CARTESIAN_POINT ( 'NONE',  ( 776.2046728542105711, -68.19088175424413123, -304.8212110874238761 ) ) ;
#42695 = CARTESIAN_POINT ( 'NONE',  ( 187.1337867209877857, 62.79977829742938411, 207.3621835540872951 ) ) ;
#42696 = CARTESIAN_POINT ( 'NONE',  ( -858.8365100919713768, 260.0000000000002274, -199.9999999999881481 ) ) ;
#42697 = EDGE_CURVE ( 'NONE', #16430, #23506, #36378, .T. ) ;
#42698 = CARTESIAN_POINT ( 'NONE',  ( 766.0291762391763086, -274.9181544815161828, 360.7704444035551319 ) ) ;
#42699 = CARTESIAN_POINT ( 'NONE',  ( 759.7806653035534055, -150.9982390220563957, 324.8639956371180801 ) ) ;
#42700 = VERTEX_POINT ( 'NONE', #24387 ) ;
#42701 = CARTESIAN_POINT ( 'NONE',  ( 757.4527132478984868, -64.37269993606231822, -329.1273215169538844 ) ) ;
#42702 = CARTESIAN_POINT ( 'NONE',  ( 767.6429770376291799, -105.1800572038747390, -306.8695393053162093 ) ) ;
#42703 = CARTESIAN_POINT ( 'NONE',  ( 776.9566956441375396, -324.8965053807775121, 364.8461984189686405 ) ) ;
#42704 = DIRECTION ( 'NONE',  ( 0.000000000000000000, 0.000000000000000000, 1.000000000000000000 ) ) ;
#42705 = CARTESIAN_POINT ( 'NONE',  ( 815.3608509340175488, -50.73633629969874193, 341.2497674668889545 ) ) ;
#42706 = CARTESIAN_POINT ( 'NONE',  ( 805.0032342141412300, -229.5436935675106440, -314.9967657858571783 ) ) ;
#42707 = CARTESIAN_POINT ( 'NONE',  ( 781.8018195045266339, -94.27096629478386092, 365.1927285166406705 ) ) ;
#42708 = CARTESIAN_POINT ( 'NONE',  ( 799.9999999999993179, 205.0000000000000568, 329.9999999999999432 ) ) ;
#42709 = CARTESIAN_POINT ( 'NONE',  ( 758.0141637701419768, -303.0783235625957559, -367.2620300519063790 ) ) ;
#42710 = CARTESIAN_POINT ( 'NONE',  ( 745.7194118038753459, -445.6454272087883055, 348.7631598425976449 ) ) ;
#42711 = CARTESIAN_POINT ( 'NONE',  ( 808.3070685750230950, -306.9982390220558273, -361.1904061080339261 ) ) ;
#42712 = LINE ( 'NONE', #14998, #12128 ) ;
#42713 = CARTESIAN_POINT ( 'NONE',  ( 756.1348686366196716, -377.2601417444137724, 347.5531968255698416 ) ) ;
#42714 = CARTESIAN_POINT ( 'NONE',  ( 805.0032342141413437, -61.54369356751124798, 314.9967657858572352 ) ) ;
#42715 = CARTESIAN_POINT ( 'NONE',  ( 797.8594530101008786, -373.5436935675101040, -322.1405469898980982 ) ) ;
#42716 = CARTESIAN_POINT ( 'NONE',  ( 796.7845633553578182, -57.62377810805111267, 358.5707757039688204 ) ) ;
#42717 = CARTESIAN_POINT ( 'NONE',  ( 747.3154664389472828, -67.98741447168742980, -326.4474001241230781 ) ) ;
#42718 = CARTESIAN_POINT ( 'NONE',  ( 746.7653713866222915, -209.2601417444142839, 351.0478386215610271 ) ) ;
#42719 = CARTESIAN_POINT ( 'NONE',  ( 778.2165204200184689, -22.81642084023865280, 364.9363028652563230 ) ) ;
#42720 = CIRCLE ( 'NONE', #2155, 6.118999999999985562 ) ;
#42721 = EDGE_LOOP ( 'NONE', ( #27064, #10801, #4676, #12546 ) ) ;
#42722 = CARTESIAN_POINT ( 'NONE',  ( 805.0264073115434940, -198.3510508353234059, -339.4763451958999099 ) ) ;
#42723 = CARTESIAN_POINT ( 'NONE',  ( 771.2633955100217236, -191.9073299311471885, 363.4237431249939618 ) ) ;
#42724 = CARTESIAN_POINT ( 'NONE',  ( 744.8212110874229666, -18.89650538077849617, -336.2046728542121627 ) ) ;
#42725 = CARTESIAN_POINT ( 'NONE',  ( 762.1405469898973024, -337.5436935675102745, 357.8594530101016176 ) ) ;
#42726 = CARTESIAN_POINT ( 'NONE',  ( 802.3178104526313064, -452.9681489794448339, -352.6268974387025423 ) ) ;
#42727 = DIRECTION ( 'NONE',  ( -0.000000000000000000, 1.000000000000000000, -0.000000000000000000 ) ) ;
#42728 = ORIENTED_EDGE ( 'NONE', *, *, #41837, .F. ) ;
#42729 = CARTESIAN_POINT ( 'NONE',  ( 764.0069404352550464, -39.07832356259662276, 359.2566176426627180 ) ) ;
#42730 = CARTESIAN_POINT ( 'NONE',  ( 776.2046728542105711, -332.1908817542433781, -304.8212110874238761 ) ) ;
#42731 = CARTESIAN_POINT ( 'NONE',  ( 813.1304606946831655, -305.9073299311468190, 352.3570229623691716 ) ) ;
#42732 = EDGE_CURVE ( 'NONE', #30067, #39949, #14993, .T. ) ;
#42733 = CARTESIAN_POINT ( 'NONE',  ( 766.5853460496234675, -13.98741447168760033, 372.3518521366060554 ) ) ;
#42734 = CARTESIAN_POINT ( 'NONE',  ( 805.2837595273609850, -194.7363362996982517, -340.5290396650784714 ) ) ;
#42735 = CARTESIAN_POINT ( 'NONE',  ( 771.1735550268778070, -153.1800572038746395, -316.3353852180827630 ) ) ;
#42736 = CARTESIAN_POINT ( 'NONE',  ( 805.1927285166399315, -352.8164208402375266, -341.8018195045277707 ) ) ;
#42737 = ORIENTED_EDGE ( 'NONE', *, *, #8842, .T. ) ;
#42738 = CARTESIAN_POINT ( 'NONE',  ( 746.8695393053150156, -293.9073299311468759, 327.6429770376306010 ) ) ;
#42739 = CARTESIAN_POINT ( 'NONE',  ( 190.7583438952259485, 290.0000000000001137, -274.9999999999999432 ) ) ;
#42740 = CARTESIAN_POINT ( 'NONE',  ( 766.7756240680305382, -350.5328690171411381, 361.5560724626415663 ) ) ;
#42741 = EDGE_CURVE ( 'NONE', #33435, #7627, #9069, .T. ) ;
#42742 = DIRECTION ( 'NONE',  ( -0.000000000000000000, -1.110223024625155554E-15, -1.000000000000000000 ) ) ;
#42743 = ADVANCED_FACE ( 'NONE', ( #34789 ), #35252, .F. ) ;
#42744 = CARTESIAN_POINT ( 'NONE',  ( 776.9254006560222479, -164.1908817542438612, 314.8983024940802125 ) ) ;
#42745 = CARTESIAN_POINT ( 'NONE',  ( 771.2633955100217236, -47.90732993114767169, 363.4237431249939618 ) ) ;
#42746 = ORIENTED_EDGE ( 'NONE', *, *, #23016, .F. ) ;
#42747 = CARTESIAN_POINT ( 'NONE',  ( 778.7629533639073998, -416.7363362996975980, -375.0009284576466371 ) ) ;
#42748 = CARTESIAN_POINT ( 'NONE',  ( 759.0252816721024374, -0.9982390220569063999, -368.0189434323527280 ) ) ;
#42749 = CARTESIAN_POINT ( 'NONE',  ( 812.3518521366052028, -265.0999726633344267, 326.5853460496235243 ) ) ;
#42750 = VECTOR ( 'NONE', #10465, 1000.000000000000000 ) ;
#42751 = CARTESIAN_POINT ( 'NONE',  ( 761.2382568024794409, -207.6237781080506295, 356.9571628226838129 ) ) ;
#42752 = CARTESIAN_POINT ( 'NONE',  ( 754.8072714833581358, -364.8164208402374697, -338.1981804954720587 ) ) ;
#42753 = CARTESIAN_POINT ( 'NONE',  ( 765.0180583372156207, -0.9982390220569063999, 360.0135310231089534 ) ) ;
#42754 = CARTESIAN_POINT ( 'NONE',  ( 793.9708237608222134, -238.9181544815163534, -319.2295555964448681 ) ) ;
#42755 = CARTESIAN_POINT ( 'NONE',  ( 745.4481719005789273, -3.725511749329622813, 347.5162901302853129 ) ) ;
#42756 = CARTESIAN_POINT ( 'NONE',  ( 745.7998596910086917, -125.3618753856928834, 332.5602148656461168 ) ) ;
#42757 = DIRECTION ( 'NONE',  ( 4.625929269271485914E-16, -1.000000000000000000, 0.000000000000000000 ) ) ;
#42758 = CARTESIAN_POINT ( 'NONE',  ( 792.3570229623691148, -405.1800572038737869, -373.1304606946836770 ) ) ;
#42759 = PLANE ( 'NONE',  #29102 ) ;
#42760 = EDGE_CURVE ( 'NONE', #7627, #33435, #12021, .T. ) ;
#42761 = CARTESIAN_POINT ( 'NONE',  ( 748.6759233522253680, -352.3726999360614514, 324.3348316497537098 ) ) ;
#42762 = ADVANCED_FACE ( 'NONE', ( #7090 ), #38973, .F. ) ;
#42763 = LINE ( 'NONE', #36513, #1376 ) ;
#42764 = CARTESIAN_POINT ( 'NONE',  ( 745.0891759886404770, -340.2709662947831362, 342.4968714119734159 ) ) ;
#42765 = CARTESIAN_POINT ( 'NONE',  ( 814.9108240113580450, -40.27096629478405987, -337.5031285880265273 ) ) ;
#42766 = CARTESIAN_POINT ( 'NONE',  ( 768.0187753319979720, -296.6346026584195670, -318.0580252608186242 ) ) ;
#42767 = CARTESIAN_POINT ( 'NONE',  ( 879.9999999999990905, 479.9999999999998863, -210.0000000000000000 ) ) ;
#42768 = CARTESIAN_POINT ( 'NONE',  ( 803.6646147819161570, -425.9073299311463074, 348.8264449731210561 ) ) ;
#42769 = ADVANCED_FACE ( 'NONE', ( #1289 ), #1499, .F. ) ;
#42770 = CARTESIAN_POINT ( 'NONE',  ( 780.5236548040995785, -188.7363362996983085, 314.9735926884559944 ) ) ;
#42771 = CARTESIAN_POINT ( 'NONE',  ( 755.8990559732751535, -59.46360902697142592, -365.9055244015606831 ) ) ;
#42772 = CARTESIAN_POINT ( 'NONE',  ( 754.9735926884551418, -90.35105083532373271, -340.5236548041000333 ) ) ;
#42773 = CARTESIAN_POINT ( 'NONE',  ( 798.0661480581538854, -98.53286901714187707, 309.5768839229118043 ) ) ;
#42774 = CARTESIAN_POINT ( 'NONE',  ( 797.8594530101009923, -421.5436935675101040, 322.1405469898982119 ) ) ;
#42775 = CARTESIAN_POINT ( 'NONE',  ( 804.9363028652555840, 7.729033705215793582, -338.2165204200192079 ) ) ;
#42777 = ORIENTED_EDGE ( 'NONE', *, *, #43893, .F. ) ;
#42776 = CARTESIAN_POINT ( 'NONE',  ( 794.1144889064781864, -106.1692326535054889, -360.9840315886528401 ) ) ;
#42778 = CARTESIAN_POINT ( 'NONE',  ( 788.7366044899766848, -83.90732993114754379, -316.5762568750059813 ) ) ;
#42779 = CARTESIAN_POINT ( 'NONE',  ( 802.7791456095903868, -412.7146871989590409, -329.0155153010375102 ) ) ;
#42781 = CARTESIAN_POINT ( 'NONE',  ( 778.2165204200184689, -214.8164208402380666, 364.9363028652563230 ) ) ;
#42780 = CARTESIAN_POINT ( 'NONE',  ( 759.7806653035534055, -222.9982390220561399, 324.8639956371180801 ) ) ;
#42782 = CARTESIAN_POINT ( 'NONE',  ( 747.3154664389472828, -403.9874144716863498, -326.4474001241230781 ) ) ;
#42783 = DIRECTION ( 'NONE',  ( 0.000000000000000000, 0.000000000000000000, -1.000000000000000000 ) ) ;
#42784 = EDGE_LOOP ( 'NONE', ( #34999, #12158, #25397, #25960 ) ) ;
#42785 = CARTESIAN_POINT ( 'NONE',  ( 785.3141322388236176, -429.7255117493282910, 364.4286716492789537 ) ) ;
#42786 = EDGE_CURVE ( 'NONE', #32578, #9428, #43719, .T. ) ;
#42787 = ORIENTED_EDGE ( 'NONE', *, *, #23553, .T. ) ;
#42788 =( NAMED_UNIT ( * ) SI_UNIT ( $, .STERADIAN. ) SOLID_ANGLE_UNIT ( ) );
#42789 = CARTESIAN_POINT ( 'NONE',  ( 767.7687537140311633, -263.9073299311469327, -372.7932403749916830 ) ) ;
#42790 = CARTESIAN_POINT ( 'NONE',  ( 745.7998596910086917, -173.3618753856927128, 332.5602148656461168 ) ) ;
#42791 = EDGE_CURVE ( 'NONE', #5020, #25862, #34118, .T. ) ;
#42792 = CARTESIAN_POINT ( 'NONE',  ( 763.0428371773158460, -251.4636090269709143, 358.7617431975195359 ) ) ;
#42793 = CARTESIAN_POINT ( 'NONE',  ( 763.2154366446407039, -381.6237781080500326, 321.4292242960311228 ) ) ;
#42794 = ORIENTED_EDGE ( 'NONE', *, *, #6120, .T. ) ;
#42795 = CARTESIAN_POINT ( 'NONE',  ( 801.5560724626406000, -72.55451811788049099, -326.7756240680316182 ) ) ;
#42796 = CARTESIAN_POINT ( 'NONE',  ( 814.8230680027162407, -197.8055962898688733, 333.7305795820267917 ) ) ;
#42797 = CARTESIAN_POINT ( 'NONE',  ( 797.8594530101009923, -229.5436935675107009, -322.1405469898982119 ) ) ;
#42798 = ORIENTED_EDGE ( 'NONE', *, *, #33183, .F. ) ;
#42799 = CARTESIAN_POINT ( 'NONE',  ( 759.7806653035534055, -342.9982390220557136, -324.8639956371180801 ) ) ;
#42800 = CARTESIAN_POINT ( 'NONE',  ( 762.1405469898971887, -49.54369356751129061, -357.8594530101015607 ) ) ;
#42801 = CARTESIAN_POINT ( 'NONE',  ( 756.1348686366196716, -233.2601417444141987, 347.5531968255698416 ) ) ;
#42802 = LINE ( 'NONE', #21779, #18887 ) ;
#42803 = LINE ( 'NONE', #7256, #21892 ) ;
#42804 = EDGE_CURVE ( 'NONE', #13608, #38059, #29679, .T. ) ;
#42805 = ORIENTED_EDGE ( 'NONE', *, *, #11198, .F. ) ;
#42806 = CARTESIAN_POINT ( 'NONE',  ( 754.8072714833581358, -4.816420840238714085, -338.1981804954720587 ) ) ;
#42807 = CYLINDRICAL_SURFACE ( 'NONE', #39537, 2.749999999999863665 ) ;
#42808 = CARTESIAN_POINT ( 'NONE',  ( 791.7608162188021197, 178.9475563372491251, 320.0000000000000000 ) ) ;
#42809 = EDGE_LOOP ( 'NONE', ( #5723, #8428, #9154, #30110 ) ) ;
#42810 = CARTESIAN_POINT ( 'NONE',  ( 795.8262568251477660, -286.3726999360617356, -308.3538107759623585 ) ) ;
#42811 = CARTESIAN_POINT ( 'NONE',  ( 778.7629533639073998, -176.7363362996983369, 375.0009284576466371 ) ) ;
#42813 = CARTESIAN_POINT ( 'NONE',  ( 762.3223304703356007, -247.5436935675106724, -322.3223304703362828 ) ) ;
#42812 = DIRECTION ( 'NONE',  ( 0.000000000000000000, 0.000000000000000000, -1.000000000000000000 ) ) ;
#42814 = PLANE ( 'NONE',  #39301 ) ;
#42815 = CARTESIAN_POINT ( 'NONE',  ( 804.8461984189677878, -122.1908817542439749, -336.9566956441385628 ) ) ;
#42816 = CARTESIAN_POINT ( 'NONE',  ( 799.9636004259356241, -382.9181544815159555, 311.2241431872006956 ) ) ;
#42817 = CYLINDRICAL_SURFACE ( 'NONE', #19521, 7.999999999999896083 ) ;
#42818 = CARTESIAN_POINT ( 'NONE',  ( 766.5853460496234675, -13.98741447168760033, -372.3518521366060554 ) ) ;
#42819 = CARTESIAN_POINT ( 'NONE',  ( 751.6929314249750860, -294.9982390220559978, -318.8095938919659034 ) ) ;
#42820 = DIRECTION ( 'NONE',  ( -1.000000000000000000, 0.000000000000000000, 0.000000000000000000 ) ) ;
#42821 = CARTESIAN_POINT ( 'NONE',  ( 781.8018195045266339, 1.729033705215812011, 365.1927285166406705 ) ) ;
#42822 = CARTESIAN_POINT ( 'NONE',  ( 762.1177392798416577, -234.5545181178799794, 309.8865473780659272 ) ) ;
#42823 = CARTESIAN_POINT ( 'NONE',  ( 752.4576283171824116, -213.0783235625960401, -317.7880784355627952 ) ) ;
#42824 = CARTESIAN_POINT ( 'NONE',  ( 754.9967657858570647, -217.5436935675107293, 365.0032342141425374 ) ) ;
#42825 = CARTESIAN_POINT ( 'NONE',  ( 754.3581564841646241, 6.536390973028352924, -316.1443688327762516 ) ) ;
#42826 = CYLINDRICAL_SURFACE ( 'NONE', #35007, 6.118999999999985562 ) ;
#42827 = CARTESIAN_POINT ( 'NONE',  ( 791.9812246680005501, -308.6346026584195670, 361.9419747391813189 ) ) ;
#42828 = CARTESIAN_POINT ( 'NONE',  ( 796.1575198192839480, -78.00906357242591582, 359.4546378042384163 ) ) ;
#42829 = CARTESIAN_POINT ( 'NONE',  ( 780.5236548040995785, -68.73633629969867798, 314.9735926884559944 ) ) ;
#42830 = CARTESIAN_POINT ( 'NONE',  ( 772.3691319403857278, 24.73985825558500551, -315.8894580844506663 ) ) ;
#42831 = DIRECTION ( 'NONE',  ( 0.000000000000000000, -0.000000000000000000, 1.000000000000000000 ) ) ;
#42832 = CARTESIAN_POINT ( 'NONE',  ( 786.4999999999993179, -513.1383975375929367, -349.9999999999999432 ) ) ;
#42834 = CARTESIAN_POINT ( 'NONE',  ( 759.9864689768902508, -362.0891481129648923, 354.9819416627836404 ) ) ;
#42833 = CARTESIAN_POINT ( 'NONE',  ( 776.9566956441375396, -156.8965053807780805, 364.8461984189686405 ) ) ;
#42835 = ORIENTED_EDGE ( 'NONE', *, *, #40478, .T. ) ;
#42836 = CARTESIAN_POINT ( 'NONE',  ( 804.1601925771018387, -295.4419599262320730, -346.5483106153029098 ) ) ;
#42837 = CARTESIAN_POINT ( 'NONE',  ( 778.1981804954714335, -130.2709662947837899, 314.8072714833589885 ) ) ;
#42838 = CARTESIAN_POINT ( 'NONE',  ( 805.9055244015594326, -291.6237781080503169, -315.8990559732753240 ) ) ;
#42839 = DIRECTION ( 'NONE',  ( -1.000000000000000000, -0.000000000000000000, -0.000000000000000000 ) ) ;
#42840 = CARTESIAN_POINT ( 'NONE',  ( 801.9858362298568863, -435.0783235625953580, 312.7379699480935642 ) ) ;
#42841 = ORIENTED_EDGE ( 'NONE', *, *, #5210, .T. ) ;
#42842 = CARTESIAN_POINT ( 'NONE',  ( 788.8264449731200330, -333.1800572038740142, 363.6646147819171233 ) ) ;
#42843 = CARTESIAN_POINT ( 'NONE',  ( 793.2243759319678702, -74.53286901714196233, -318.4439275373583200 ) ) ;
#42844 = CARTESIAN_POINT ( 'NONE',  ( 804.9363028652555840, -160.2709662947836762, -338.2165204200192079 ) ) ;
#42845 = CARTESIAN_POINT ( 'NONE',  ( 756.5762568750052424, -435.1800572038737869, 348.7366044899774238 ) ) ;
#42846 = CARTESIAN_POINT ( 'NONE',  ( 801.1904061080336987, -140.0891481129654892, -368.3070685750235498 ) ) ;
#42847 = ORIENTED_EDGE ( 'NONE', *, *, #16352, .F. ) ;
#42848 = CARTESIAN_POINT ( 'NONE',  ( 781.7834795799800531, -154.8164208402382371, -315.0636971347436202 ) ) ;
#42849 = ORIENTED_EDGE ( 'NONE', *, *, #8063, .T. ) ;
#42850 = CARTESIAN_POINT ( 'NONE',  ( 755.3028492785439312, -375.2817908451523294, -335.9200461376539693 ) ) ;
#42851 = CARTESIAN_POINT ( 'NONE',  ( 804.9363028652555840, 7.729033705215793582, 338.2165204200192079 ) ) ;
#42852 = CARTESIAN_POINT ( 'NONE',  ( 755.8398074228967971, -115.4419599262327409, 333.4516893846970333 ) ) ;
#42855 = CARTESIAN_POINT ( 'NONE',  ( 747.3154664389472828, -403.9874144716863498, 326.4474001241230781 ) ) ;
#42854 = FACE_BOUND ( 'NONE', #12965, .T. ) ;
#42853 = DIRECTION ( 'NONE',  ( 0.000000000000000000, 0.000000000000000000, 1.000000000000000000 ) ) ;
#42856 = EDGE_LOOP ( 'NONE', ( #34553, #39023 ) ) ;
#42857 = CARTESIAN_POINT ( 'NONE',  ( 755.1538015810308480, -398.1908817542431507, -343.0433043558613804 ) ) ;
#42858 = DIRECTION ( 'NONE',  ( -0.000000000000000000, 1.000000000000000000, -0.000000000000000000 ) ) ;
#42859 = CARTESIAN_POINT ( 'NONE',  ( 814.2805881961230625, -169.6454272087892718, -331.2368401574024119 ) ) ;
#42860 = CARTESIAN_POINT ( 'NONE',  ( 786.2694204179717872, -69.28179084515321051, 305.1769319972829067 ) ) ;
#42862 = CARTESIAN_POINT ( 'NONE',  ( -181.9156952255813735, 290.0000000000001137, -274.9999999999999432 ) ) ;
#42861 = CARTESIAN_POINT ( 'NONE',  ( -180.7583438952258348, 394.6698570112193920, -274.9999999999999432 ) ) ;
#42863 = CARTESIAN_POINT ( 'NONE',  ( 766.7756240680305382, -326.5328690171411381, -361.5560724626415663 ) ) ;
#42864 = CARTESIAN_POINT ( 'NONE',  ( 797.8594530101008786, -445.5436935675098766, -322.1405469898980982 ) ) ;
#42865 = CARTESIAN_POINT ( 'NONE',  ( 813.5763878283155464, -195.8272453906074304, -351.1614460488615350 ) ) ;
#42866 = FACE_OUTER_BOUND ( 'NONE', #40622, .T. ) ;
#42867 = PLANE ( 'NONE',  #40792 ) ;
#42868 = CARTESIAN_POINT ( 'NONE',  ( 769.0155153010367712, -370.3726999360613377, 362.7791456095907279 ) ) ;
#42869 = CARTESIAN_POINT ( 'NONE',  ( 745.5313806188320314, -327.2817908451525000, 333.7943932421247268 ) ) ;
#42870 = CARTESIAN_POINT ( 'NONE',  ( 748.9653473494365699, -218.6346026584198228, -356.9462024416520762 ) ) ;
#42871 = CARTESIAN_POINT ( 'NONE',  ( -26.63011601220122060, -544.8427095258973623, -369.9999999999999432 ) ) ;
#42872 = CARTESIAN_POINT ( 'NONE',  ( 781.7834795799800531, -10.81642084023869543, -315.0636971347436202 ) ) ;
#42873 = CARTESIAN_POINT ( 'NONE',  ( 811.3240766477731540, -148.3726999360620198, 355.6651683502462902 ) ) ;
#42874 = CARTESIAN_POINT ( 'NONE',  ( 771.2368401574024119, -85.44195992623282621, -374.2805881961240857 ) ) ;
#42875 = CARTESIAN_POINT ( 'NONE',  ( 749.2812353651451076, -126.4527844766019626, 323.2262854647983090 ) ) ;
#42876 = CARTESIAN_POINT ( 'NONE',  ( 787.4397851343537695, -333.7255117493286320, -374.2001403089903988 ) ) ;
#42877 = CARTESIAN_POINT ( 'NONE',  ( -746.4999999999993179, -365.3551492539851893, -18.13243251470705886 ) ) ;
#42878 = FACE_OUTER_BOUND ( 'NONE', #10454, .T. ) ;
#42879 = CARTESIAN_POINT ( 'NONE',  ( 755.3201227861273992, -219.7255117493289447, 345.3687786644892981 ) ) ;
#42880 = CARTESIAN_POINT ( 'NONE',  ( 800.9840315886518738, -4.918154481517067467, 354.1144889064786412 ) ) ;
#42881 = CARTESIAN_POINT ( 'NONE',  ( 812.6845335610512393, -415.9874144716862361, -353.5525998758768651 ) ) ;
#42882 = CARTESIAN_POINT ( 'NONE',  ( 787.5162901302840055, -419.3618753856918033, -305.4481719005792684 ) ) ;
#42883 = CARTESIAN_POINT ( 'NONE',  ( 786.4999999999993179, -513.1383975375929367, -369.9999999999999432 ) ) ;
#42884 = CARTESIAN_POINT ( 'NONE',  ( 788.7631598425961101, -25.44195992623301450, 305.7194118038759143 ) ) ;
#42885 = ORIENTED_EDGE ( 'NONE', *, *, #40778, .T. ) ;
#42886 = CARTESIAN_POINT ( 'NONE',  ( 772.3691319403857278, -191.2601417444143976, -315.8894580844506663 ) ) ;
#42887 = CARTESIAN_POINT ( 'NONE',  ( 774.6312213355099630, -119.3618753856928691, -364.6798772138717482 ) ) ;
#42888 = CARTESIAN_POINT ( 'NONE',  ( 804.6798772138708955, -39.72551174932951312, 334.6312213355107019 ) ) ;
#42889 = CARTESIAN_POINT ( 'NONE',  ( 781.2497674668890113, -204.3510508353233774, -375.3608509340180603 ) ) ;
#42890 = PRESENTATION_STYLE_ASSIGNMENT (( #4107 ) ) ;
#42891 = CARTESIAN_POINT ( 'NONE',  ( 768.8385539511368734, -311.2601417444139429, 306.4236121716840557 ) ) ;
#42892 = CARTESIAN_POINT ( 'NONE',  ( 785.3141322388236176, -141.7255117493291721, 364.4286716492789537 ) ) ;
#42893 = EDGE_LOOP ( 'NONE', ( #11499, #43186, #36715, #26327, #10470, #5674, #20, #24084 ) ) ;
#42894 = CARTESIAN_POINT ( 'NONE',  ( 778.2165204200184689, -334.8164208402376403, 364.9363028652563230 ) ) ;
#42895 = CARTESIAN_POINT ( 'NONE',  ( 748.9653473494363425, -50.63460265842036989, -356.9462024416521331 ) ) ;
#42896 = EDGE_CURVE ( 'NONE', #11829, #38048, #36626, .T. ) ;
#42897 = CARTESIAN_POINT ( 'NONE',  ( 810.7187646348534145, -90.45278447660209054, 356.7737145352016341 ) ) ;
#42898 = CARTESIAN_POINT ( 'NONE',  ( 802.2119215644370342, -438.0090635724247932, -367.5423716828165084 ) ) ;
#42899 = VERTEX_POINT ( 'NONE', #19074 ) ;
#42900 = APPLICATION_PROTOCOL_DEFINITION ( 'draft international standard', 'automotive_design', 1998, #36407 ) ;
#42902 = CARTESIAN_POINT ( 'NONE',  ( 802.9823548866075953, -385.0999726633340856, 330.0799878456151077 ) ) ;
#42901 = CARTESIAN_POINT ( 'NONE',  ( 767.8955696845333705, -48.45278447660219712, 362.1676090361162323 ) ) ;
#42903 = CARTESIAN_POINT ( 'NONE',  ( 759.7806653035534055, -294.9982390220560546, -324.8639956371180801 ) ) ;
#42905 = CARTESIAN_POINT ( 'NONE',  ( 745.1769319972822814, -281.8055962898686175, 346.2694204179732083 ) ) ;
#42904 = CARTESIAN_POINT ( 'NONE',  ( 782.5225473063383106, -382.2709662947829088, 375.2698199232970637 ) ) ;
#42906 = CARTESIAN_POINT ( 'NONE',  ( 761.9338519418445230, -62.53286901714199786, 370.4231160770881957 ) ) ;
#42907 = CARTESIAN_POINT ( 'NONE',  ( 755.5913626894240451, -301.6454272087889308, -346.6156483768012890 ) ) ;
#42908 = CARTESIAN_POINT ( 'NONE',  ( 759.7806653035534055, -294.9982390220560546, -324.8639956371180801 ) ) ;
#42909 = PLANE ( 'NONE',  #14745 ) ;
#42910 = CARTESIAN_POINT ( 'NONE',  ( 805.1927285166397041, -112.8164208402383508, -341.8018195045277707 ) ) ;
#42911 = CARTESIAN_POINT ( 'NONE',  ( 1820.038553321469863, 240.0000000000001990, -201.9999999999999716 ) ) ;
#42912 = ORIENTED_EDGE ( 'NONE', *, *, #19596, .F. ) ;
#42913 = CARTESIAN_POINT ( 'NONE',  ( 801.1904061080336987, -404.0891481129646081, 368.3070685750235498 ) ) ;
#42915 = DIRECTION ( 'NONE',  ( -0.000000000000000000, -0.000000000000000000, 1.000000000000000000 ) ) ;
#42914 = DIRECTION ( 'NONE',  ( 0.000000000000000000, 0.000000000000000000, -1.000000000000000000 ) ) ;
#42916 = CARTESIAN_POINT ( 'NONE',  ( 810.4231160770870019, -72.55451811788049099, -321.9338519418446936 ) ) ;
#42917 = DIRECTION ( 'NONE',  ( 0.000000000000000000, 0.7071067811865474617, 0.7071067811865474617 ) ) ;
#42918 = FACE_BOUND ( 'NONE', #8485, .T. ) ;
#42919 = CARTESIAN_POINT ( 'NONE',  ( 755.5913626894240451, -277.6454272087889308, 346.6156483768012890 ) ) ;
#42920 = CARTESIAN_POINT ( 'NONE',  ( 764.8639956371174549, -152.0891481129655460, 319.7806653035542013 ) ) ;
#42921 = EDGE_LOOP ( 'NONE', ( #26467, #3931, #30563, #22983 ) ) ;
#42922 = CARTESIAN_POINT ( 'NONE',  ( 804.8461984189677878, -50.19088175424420939, -336.9566956441385628 ) ) ;
#42923 = CARTESIAN_POINT ( 'NONE',  ( 751.6929314249750860, -102.9982390220565662, -318.8095938919659034 ) ) ;
#42924 = CARTESIAN_POINT ( 'NONE',  ( 803.8651313633788504, -341.2601417444138292, 332.4468031744301015 ) ) ;
#42925 = FACE_OUTER_BOUND ( 'NONE', #31617, .T. ) ;
#42926 = CARTESIAN_POINT ( 'NONE',  ( 778.7629533639073998, -56.73633629969872771, 375.0009284576466371 ) ) ;
#42927 = AXIS2_PLACEMENT_3D ( 'NONE', #20029, #20494, #34106 ) ;
#42928 = CARTESIAN_POINT ( 'NONE',  ( 787.4397851343537695, -237.7255117493289163, -374.2001403089903988 ) ) ;
#42929 = CARTESIAN_POINT ( 'NONE',  ( 744.7301800767019131, -196.8164208402380950, 337.4774526936615757 ) ) ;
#42930 = CARTESIAN_POINT ( 'NONE',  ( 774.6858677611749044, -105.7255117493293000, 315.5713283507209894 ) ) ;
#42931 = DIRECTION ( 'NONE',  ( 1.000000000000000000, -0.000000000000000000, -0.000000000000000000 ) ) ;
#42932 = CARTESIAN_POINT ( 'NONE',  ( 791.1614460488616487, -323.2601417444138860, -373.5763878283158874 ) ) ;
#42933 = CARTESIAN_POINT ( 'NONE',  ( 749.5768839229115201, -444.5545181178792973, 358.0661480581553064 ) ) ;
#42934 = CARTESIAN_POINT ( 'NONE',  ( 808.3070685750230950, -330.9982390220558273, -361.1904061080339261 ) ) ;
#42935 = CARTESIAN_POINT ( 'NONE',  ( 799.9999999999993179, -365.3551492539851893, -1.867567485292990437 ) ) ;
#42936 = CARTESIAN_POINT ( 'NONE',  ( 776.9566956441375396, -348.8965053807774552, 364.8461984189686405 ) ) ;
#42937 = CARTESIAN_POINT ( 'NONE',  ( 754.9967657858570647, -49.54369356751129772, 365.0032342141425943 ) ) ;
#42938 = CARTESIAN_POINT ( 'NONE',  ( 764.8639956371174549, -416.0891481129645513, -319.7806653035542013 ) ) ;
#42939 = CARTESIAN_POINT ( 'NONE',  ( 800.7704444035546203, -52.16923265350567362, 326.0291762391768771 ) ) ;
#42940 = CARTESIAN_POINT ( 'NONE',  ( 758.0580252608178853, -198.4527844766017495, -328.0187753319985404 ) ) ;
#42941 = CARTESIAN_POINT ( 'NONE',  ( 754.0944755984390895, -87.62377810805102740, -364.1009440267246760 ) ) ;
#42942 = CARTESIAN_POINT ( 'NONE',  ( 761.9338519418445230, -206.5328690171415360, 370.4231160770881957 ) ) ;
#42943 = CARTESIAN_POINT ( 'NONE',  ( 791.9812246680005501, -68.63460265842033436, 361.9419747391813189 ) ) ;
#42944 = VERTEX_POINT ( 'NONE', #25978 ) ;
#42945 = CARTESIAN_POINT ( 'NONE',  ( 779.4709603349208464, -240.3510508353232069, -314.7162404726379918 ) ) ;
#42946 = CARTESIAN_POINT ( 'NONE',  ( 800.2193346964447755, -186.9982390220563104, 355.1360043628815788 ) ) ;
#42947 = CARTESIAN_POINT ( 'NONE',  ( 805.9055244015594326, -27.62377810805120149, -315.8990559732753240 ) ) ;
#42948 = CARTESIAN_POINT ( 'NONE',  ( 771.1735550268780344, -345.1800572038739574, 316.3353852180828198 ) ) ;
#42949 = VECTOR ( 'NONE', #831, 1000.000000000000000 ) ;
#42950 = DIRECTION ( 'NONE',  ( 0.000000000000000000, 0.000000000000000000, 1.000000000000000000 ) ) ;
#42951 = CARTESIAN_POINT ( 'NONE',  ( 919.9999999999993179, 219.9999999999998863, 350.0000000000000000 ) ) ;
#42952 = VERTEX_POINT ( 'NONE', #15817 ) ;
#42953 = CARTESIAN_POINT ( 'NONE',  ( 757.2208543904082489, -64.71468719896019195, 350.9844846989624330 ) ) ;
#42954 = CARTESIAN_POINT ( 'NONE',  ( 811.3240766477731540, -340.3726999360615082, -355.6651683502462902 ) ) ;
#42955 = CARTESIAN_POINT ( 'NONE',  ( 810.7187646348534145, -306.4527844766013800, 356.7737145352016341 ) ) ;
#42956 = CARTESIAN_POINT ( 'NONE',  ( 783.7566961878529810, -0.8965053807785533513, 305.1792804349288417 ) ) ;
#42957 = CARTESIAN_POINT ( 'NONE',  ( 802.9823548866075953, -193.0999726633346256, -330.0799878456151077 ) ) ;
#42958 = CARTESIAN_POINT ( 'NONE',  ( 804.6798772138708955, -183.7255117493290015, -334.6312213355107019 ) ) ;
#42959 = CARTESIAN_POINT ( 'NONE',  ( 758.0580252608178853, -366.4527844766012095, -328.0187753319985404 ) ) ;
#42960 = ORIENTED_EDGE ( 'NONE', *, *, #34333, .F. ) ;
#42961 = CARTESIAN_POINT ( 'NONE',  ( 789.9200121543843807, 22.01258552831228599, -317.0176451133914384 ) ) ;
#42962 = CARTESIAN_POINT ( 'NONE',  ( 812.7932403749906598, -303.1800572038740711, 327.7687537140311633 ) ) ;
#42963 = DIRECTION ( 'NONE',  ( -0.000000000000000000, 1.000000000000000000, -0.000000000000000000 ) ) ;
#42964 = CARTESIAN_POINT ( 'NONE',  ( 799.2566176426618085, -216.0090635724255037, 324.0069404352559559 ) ) ;
#42965 = CARTESIAN_POINT ( 'NONE',  ( 802.7791456095903868, -364.7146871989592114, 329.0155153010375102 ) ) ;
#42966 = DIRECTION ( 'NONE',  ( 0.000000000000000000, -1.000000000000000000, 0.000000000000000000 ) ) ;
#42967 = CARTESIAN_POINT ( 'NONE',  ( 793.9708237608222134, -166.9181544815165523, 319.2295555964448681 ) ) ;
#42968 = CARTESIAN_POINT ( 'NONE',  ( 788.7366044899766848, -59.90732993114762905, 316.5762568750059813 ) ) ;
#42969 = EDGE_CURVE ( 'NONE', #14164, #32232, #43992, .T. ) ;
#42970 = VERTEX_POINT ( 'NONE', #40086 ) ;
#42971 = CARTESIAN_POINT ( 'NONE',  ( 755.8990559732751535, -419.4636090269702891, -365.9055244015606831 ) ) ;
#42972 = CIRCLE ( 'NONE', #11987, 2.749999999999919176 ) ;
#42973 = CARTESIAN_POINT ( 'NONE',  ( 767.6429770376291799, 14.81994279612486309, -306.8695393053162093 ) ) ;
#42974 = CARTESIAN_POINT ( 'NONE',  ( 750.9282345327678740, -256.9181544815163534, 319.8311093483690115 ) ) ;
#42975 = CARTESIAN_POINT ( 'NONE',  ( 760.5453621957607311, -213.0783235625960401, 323.8424801807151425 ) ) ;
#42976 = CARTESIAN_POINT ( 'NONE',  ( 762.1405469898971887, -361.5436935675103882, -357.8594530101015607 ) ) ;
#42977 = CARTESIAN_POINT ( 'NONE',  ( 762.3223304703356007, 16.45630643248849267, -322.3223304703362828 ) ) ;
#42978 = CARTESIAN_POINT ( 'NONE',  ( 805.1927285166397041, 7.183579159761247723, 341.8018195045277707 ) ) ;
#42979 = DIRECTION ( 'NONE',  ( 1.000000000000000000, 4.625929269271485914E-16, 0.000000000000000000 ) ) ;
#42980 = CARTESIAN_POINT ( 'NONE',  ( 775.8780910478218402, -273.2817908451526137, -364.9511171171680530 ) ) ;
#42981 = CARTESIAN_POINT ( 'NONE',  ( 814.9108240113580450, -16.27096629478413092, 337.5031285880265273 ) ) ;
#42982 = CARTESIAN_POINT ( 'NONE',  ( 812.7932403749906598, -111.1800572038747532, 327.7687537140311633 ) ) ;
#42983 = AXIS2_PLACEMENT_3D ( 'NONE', #18350, #17878, #22234 ) ;
#42984 = DIRECTION ( 'NONE',  ( 0.000000000000000000, 0.000000000000000000, 1.000000000000000000 ) ) ;
#42985 = DIRECTION ( 'NONE',  ( 1.000000000000000000, -0.000000000000000000, -0.000000000000000000 ) ) ;
#42986 = SURFACE_STYLE_USAGE ( .BOTH. , #18520 ) ;
#42987 = CARTESIAN_POINT ( 'NONE',  ( 768.9521613784389729, -393.8272453906067199, 373.2346286133773106 ) ) ;
#42988 = DIRECTION ( 'NONE',  ( 0.000000000000000000, 0.000000000000000000, 1.000000000000000000 ) ) ;
#42989 = CARTESIAN_POINT ( 'NONE',  ( 808.3070685750230950, -330.9982390220558273, 361.1904061080339261 ) ) ;
#42990 = CARTESIAN_POINT ( 'NONE',  ( 791.9812246680005501, -332.6346026584195101, -361.9419747391813189 ) ) ;
#42991 = ADVANCED_FACE ( 'NONE', ( #15160 ), #18621, .T. ) ;
#42992 = DIRECTION ( 'NONE',  ( 0.000000000000000000, 0.000000000000000000, -1.000000000000000000 ) ) ;
#42993 = CARTESIAN_POINT ( 'NONE',  ( 794.9819416627830151, -444.9982390220554862, 319.9864689768909898 ) ) ;
#42994 = CARTESIAN_POINT ( 'NONE',  ( 796.9571628226829034, -191.4636090269709996, 321.2382568024804641 ) ) ;
#42995 = CARTESIAN_POINT ( 'NONE',  ( 799.9636004259356241, -70.91815448151683654, -311.2241431872006956 ) ) ;
#42996 = CARTESIAN_POINT ( 'NONE',  ( 759.2295555964440155, -88.16923265350555994, -353.9708237608231229 ) ) ;
#42997 = CARTESIAN_POINT ( 'NONE',  ( 768.8385539511368734, -95.26014174441461080, 306.4236121716840557 ) ) ;
#42998 = CARTESIAN_POINT ( 'NONE',  ( 759.7806653035535192, -438.9982390220554294, 324.8639956371181370 ) ) ;
#42999 = CARTESIAN_POINT ( 'NONE',  ( 758.0580252608178853, -6.452784476602343666, -328.0187753319985404 ) ) ;
#43001 = ORIENTED_EDGE ( 'NONE', *, *, #9484, .F. ) ;
#43000 = CARTESIAN_POINT ( 'NONE',  ( 759.2295555964440155, -112.1692326535054889, -353.9708237608231229 ) ) ;
#43002 = CARTESIAN_POINT ( 'NONE',  ( 768.0187753319979720, -104.6346026584202207, -318.0580252608186242 ) ) ;
#43003 = ADVANCED_FACE ( 'NONE', ( #11907, #40332, #29907, #832, #29251, #14931, #8446, #1054, #22077, #43097, #22749, #11463, #5194, #33162, #33368 ), #7771, .T. ) ;
#43004 = CARTESIAN_POINT ( 'NONE',  ( 783.0433043558608688, -408.8965053807772847, -315.1538015810313027 ) ) ;
#43006 = CARTESIAN_POINT ( 'NONE',  ( 803.6646147819162707, -233.9073299311470464, 348.8264449731211130 ) ) ;
#43005 = CARTESIAN_POINT ( 'NONE',  ( 800.0135310231082713, -278.0891481129651197, 325.0180583372163028 ) ) ;
#43007 = AXIS2_PLACEMENT_3D ( 'NONE', #10535, #7544, #31780 ) ;
#43008 = FACE_OUTER_BOUND ( 'NONE', #20560, .T. ) ;
#43009 = ORIENTED_EDGE ( 'NONE', *, *, #17569, .T. ) ;
#43010 = CARTESIAN_POINT ( 'NONE',  ( 762.3223304703356007, -439.5436935675101040, 322.3223304703362828 ) ) ;
#43011 = ORIENTED_EDGE ( 'NONE', *, *, #3538, .T. ) ;
#43012 = CARTESIAN_POINT ( 'NONE',  ( 751.6929314249750860, -174.9982390220563673, 318.8095938919659034 ) ) ;
#43013 = CARTESIAN_POINT ( 'NONE',  ( 796.9571628226829034, -263.4636090269708006, 321.2382568024804641 ) ) ;
#43014 = ORIENTED_EDGE ( 'NONE', *, *, #32844, .F. ) ;
#43015 = CARTESIAN_POINT ( 'NONE',  ( 766.0291762391763086, -82.91815448151682233, -360.7704444035551319 ) ) ;
#43016 = CARTESIAN_POINT ( 'NONE',  ( 744.8212110874229666, -234.8965053807777963, 336.2046728542121627 ) ) ;
#43017 = CARTESIAN_POINT ( 'NONE',  ( 755.3201227861273992, -243.7255117493288310, -345.3687786644892981 ) ) ;
#43018 = ORIENTED_EDGE ( 'NONE', *, *, #9907, .T. ) ;
#43019 = EDGE_CURVE ( 'NONE', #45067, #8740, #18683, .T. ) ;
#43020 = CARTESIAN_POINT ( 'NONE',  ( 804.4286716492782716, -377.3618753856920875, -345.3141322388244703 ) ) ;
#43021 = CARTESIAN_POINT ( 'NONE',  ( 804.4286716492782716, -41.36187538569314626, -345.3141322388244703 ) ) ;
#43022 = VECTOR ( 'NONE', #32031, 1000.000000000000000 ) ;
#43023 = EDGE_CURVE ( 'NONE', #21713, #23858, #23067, .T. ) ;
#43024 = CARTESIAN_POINT ( 'NONE',  ( 803.2186876482843445, -247.9874144716867761, 350.0220218866286928 ) ) ;
#43025 = CARTESIAN_POINT ( 'NONE',  ( 919.9999999999993179, 219.9999999999998863, 339.9999999999999432 ) ) ;
#43026 = CYLINDRICAL_SURFACE ( 'NONE', #33170, 10.00000000000000888 ) ;
#43027 = CARTESIAN_POINT ( 'NONE',  ( 757.8323909638827445, -26.63460265842045871, -352.1044303154654358 ) ) ;
#43028 = CARTESIAN_POINT ( 'NONE',  ( 799.9999999999993179, 205.0000000000000568, -339.9999999999999432 ) ) ;
#43029 = ORIENTED_EDGE ( 'NONE', *, *, #40568, .F. ) ;
#43030 = CARTESIAN_POINT ( 'NONE',  ( 813.5763878283155464, -315.8272453906070609, -351.1614460488615350 ) ) ;
#43031 = CARTESIAN_POINT ( 'NONE',  ( 760.0363995740630116, -154.9181544815165523, 368.7758568127991907 ) ) ;
#43033 = CARTESIAN_POINT ( 'NONE',  ( 755.0636971347428243, -268.2709662947833067, -341.7834795799807353 ) ) ;
#43032 = CARTESIAN_POINT ( 'NONE',  ( 355.8971257818259915, 290.0000000000001137, -244.9999999999999716 ) ) ;
#43034 =( BOUNDED_SURFACE ( )  B_SPLINE_SURFACE ( 3, 2, ( 
 ( #14487, #7549, #5985, #42414, #14027, #3853, #23532, #28567, #42656, #11018, #10785, #45037, #24861, #35709, #23753, #13168, #27018, #37868, #38978, #21626, #17944, #6215, #25085, #41117, #9470, #26224, #11239, #11701, #43334, #32486, #18183, #15166, #35949, #29257, #21857, #29472, #40090, #43762, #36173, #32259, #25773, #12142, #836, #36392, #25551, #14935, #8014, #22522, #18858, #40339, #42872, #43546, #8227, #11471, #36633, #29018, #4987, #43101, #4315, #39665, #617, #22082, #15393, #4533, #18406, #8452, #39885, #32948, #8691, #18626, #4755, #32712, #1059, #22296, #19080, #1295, #22755, #25312, #11912, #25983, #33169, #1505, #15602, #29686, #36850, #14719, #28794, #39425, #7780, #2414, #19510, #22968, #27144, #44457, #19979, #1720, #34280, #15824, #30832, #20199, #44926, #44696, #12375, #2192, #2652, #23875, #16284, #23190, #13056, #19289, #16514, #30596, #27361, #44001, #12813, #41231, #40765, #37063, #9590, #23650, #37531, #44232, #34055, #5890, #16750, #5416, #8901, #40550, #26452, #9122, #29916, #33608, #12590, #37298, #37761, #41001, #6110, #1960, #16060, #13284, #26894, #5659, #19752, #41456, #26668, #9808, #30143, #33838, #5202, #33375, #30364, #9361, #23430, #10263, #6795, #17667, #24804, #31051, #42135, #41919, #21121, #16975, #97, #31729, #14189, #24340, #27822, #20872, #38924, #34742, #45150, #37995, #17192, #31279, #7276, #38444, #27584, #41689, #34525, #28257, #6348, #13511, #34970, #3344, #6571, #20432, #17437, #38225, #31517, #24113, #7035, #42356, #2883, #45620, #10043, #35204, #13968, #45383, #20650, #28041, #10486, #3102, #3581, #24560, #38676, #10725, #13745, #41599, #26586, #27062, #12972, #2111, #33526, #30508, #5574, #44611, #37210, #44847, #9728, #13430, #5812, #1874, #41157, #27500, #16200, #6026, #40914, #30280, #23351, #37904, #34193, #9956, #12510, #13209, #23572, #26808, #6258, #44373, #20345, #12728, #19666, #9281, #15982, #37453, #30754, #19900, #33759, #23792, #9508, #2563, #30065, #16896, #44146, #24026, #2805, #38145, #27286, #40684, #37677, #30977, #6496, #20117, #33977, #41379, #9038, #34440, #45075, #23108, #2328, #16668, #16427, #10405, #38368, #24947, #14338, #7188, #13887, #3717, #21262, #18032, #20791, #24260, #10184, #41839, #24482, #17116, #34886, #27961, #38588, #35341, #10636, #17804, #6714, #17342, #42514, #42275, #6944, #35115, #478, #42057, #39062, #31428, #3250, #10879, #20574, #7410, #27735, #28416, #17580, #14109, #35562, #42735, #45534, #31871, #3492, #21485, #13654, #32113, #3937, #14583, #31650, #21027, #28183, #25169, #18, #24717, #38835, #31197, #241, #28657, #11099, #39279, #34670, #3029, #45295, #4405, #29563, #29347, #11561, #22166, #33248, #917, #26070, #18495, #25403, #43637, #7633, #40184, #14804, #15483, #4613, #1153, #22613, #29775, #28878, #18946, #36255, #12007, #707, #5073, #36713, #19164, #18709, #8105, #15258, #12235, #15019, #42958, #21711, #29108, #43192, #43852, #32799, #11325, #39525, #35808, #1593, #15692, #7880, #43420, #11787, #21956, #4184, #25858, #36042, #39968, #32573, #33042, #8549, #26314, #25643, #18279, #8313, #32353, #39757, #22377, #36482, #4847, #1380, #44793, #41094, #2749, #19380, #5967, #30447, #33700, #13148, #8984, #27229, #5511, #12455, #37151, #22840, #19607, #37614, #23053, #26534, #16609, #33920, #9449, #36933, #23736, #5287, #20287, #9671, #34380, #34134, #1812, #37395, #37847, #13372, #5749, #12673, #2502, #8772, #20056, #30697, #16844, #33464, #2271, #41321, #30227, #40632, #6195, #30923, #26998, #2050, #23513, #45019, #40420, #16144, #44090, #44318, #16369, #9219, #15919, #30003, #26753, #40856, #23294, #12910, #44549, #19838, #38532, #35061, #42228, #38316, #42457, #192, #20963, #41783, #17757, #28353, #21211, #13595, #2972, #14284, #31137, #7361, #31371, #23967, #10824, #45709, #24659, #3670, #10581, #31605, #28133, #17061, #24896, #31821, #21437, #9893, #17982, #6886, #6663, #6444, #32052, #3435, #17532, #423, #34829, #42009, #35513, #38775, #38089, #45479, #14061, #27444, #39010, #27678, #7133, #20736, #41542, #35292, #3888, #20523, #34617, #45235, #24429, #10133, #24206, #13835, #10353, #3193, #27912, #17282, #36206, #35988, #25596, #36670, #28604, #5030, #21662, #870, #39465, #14973, #11510, #18661, #32751, #39232, #11741, #25118, #4131, #43585, #43144, #4570, #19120, #18897, #26021, #29058, #28828, #11953, #7825, #21904, #18223, #40131, #8264, #4354, #8053, #18444, #42686, #1098, #39706, #32522, #22118, #15212, #29300, #43375, #8495, #35752, #42908, #14528, #32299, #25808, #39921, #22329, #36430, #4794, #32993, #653, #15435, #1331, #22566, #11053, #33209, #29513, #7585, #14754, #11275, #25351, #9163, #6149, #8937, #16097, #41271, #2227, #43802, #19553, #23236, #20239, #5923, #33415, #12858, #12410, #1546, #19791, #26939, #16322, #37342, #26265, #44272, #41039, #33874, #33649, #30181, #29724, #2001, #12184, #5704, #23008, #12629, #23689, #15641, #37800, #8730, #26707, #26490, #40806, #30403, #9400, #23467, #40379, #37566, #22795, #5242, #30643, #20013, #34089, #19332, #2455, #13099, #16558, #15867, #44741, #40591, #37102, #1759, #27183, #9626, #5458, #29956, #44040, #2697, #38482, #3142, #6614, #20689, #35010, #6833, #10085, #14230, #41494, #2923, #34326, #6394, #24158, #41731, #45426, #41962, #17233, #10305, #17012, #24378, #31320, #31770, #31560, #27623, #7079, #10768, #20913, #3386, #28299, #13788, #17479, #45660, #45187, #3621, #21160, #27867, #31089, #24601, #35243, #28080, #20478, #9847, #17709, #38038, #42399, #38268, #30871, #141, #14010, #42176, #10525, #38719, #24845, #38964, #7314, #16794, #44967, #23917, #13323, #27399, #34565, #13549, #34780, #23198, #19760, #36860, #8700, #1728, #12823, #1516, #1306, #8236, #15611, #43771, #30374, #22765, #43555, #11921, #36402, #37307, #16292, #15403, #15833, #33384, #22533, #22305, #5211, #25992, #19299, #40100, #19520, #30151, #33846, #26235, #4765, #29925, #2200, #36643, #26460, #29696, #4998, #12152, #12600, #8910, #44467, #32960, #33618, #44010, #40348, #26678, #19091, #40774, #33180, #8463, #12383, #18868, #40562, #5425, #22977, #37073, #44241, #1970, #16068, #29484, #5669, #9131, #26903, #10272, #20881, #34750, #2424, #38006, #38452, #13978, #6360, #13293, #3111, #9371, #6580, #38234, #17446, #34063, #2891, #17200, #30840, #13066, #45392, #31288, #27593, #34292, #24125, #41699, #6803, #41240, #44705, #30607, #16525, #44935, #37539, #9598, #2663, #27369, #10055, #31060, #20658, #27152, #37769, #13754, #16983, #41464, #9817, #3354, #16760, #27834, #6118, #23658, #41929, #41010, #24348, #20209, #31527, #20443, #45630, #23884, #34533, #23438, #45158, #13520, #5898, #19987, #17677, #31738, #10495, #11417, #36129, #21130, #21576, #7504, #42366, #28050, #25042, #106, #39152, #14199, #39373, #4274, #7971, #333, #42144 ),
 ( #28266, #18366, #35658, #42830, #24569, #25503, #38687, #22038, #43055, #4492, #21805, #35214, #4032, #39616, #1011, #18131, #14436, #35901, #7045, #7727, #25264, #18584, #3589, #32210, #32446, #17895, #10734, #794, #14894, #14673, #21355, #11191, #28749, #32668, #24813, #38933, #7284, #35433, #31962, #3804, #28517, #42613, #10973, #28974, #572, #15779, #18809, #11868, #37015, #36803, #19034, #29641, #40715, #8405, #33558, #25941, #32899, #5369, #15116, #1906, #22250, #22923, #12096, #8643, #30096, #37243, #36348, #26403, #43721, #19463, #8185, #12542, #44178, #26617, #26175, #15561, #22705, #40287, #5159, #29868, #40048, #9071, #16015, #19243, #29428, #23137, #5606, #8856, #1245, #4706, #19700, #15348, #33790, #33125, #11654, #29205, #33330, #12330, #43284, #43951, #1675, #40505, #43501, #25730, #39843, #22474, #36581, #4938, #1461, #27091, #26837, #38397, #9758, #23823, #6747, #9537, #16699, #41870, #2834, #44403, #20147, #37934, #20821, #6524, #34004, #45104, #13003, #2141, #20377, #13461, #16926, #6292, #40946, #44875, #27530, #34474, #34223, #30784, #30309, #2598, #12758, #31006, #23601, #13237, #24291, #16230, #9309, #23379, #27315, #41183, #41408, #41630, #9989, #24058, #37482, #38176, #5843, #19929, #31231, #20603, #34698, #2358, #3057, #13689, #17146, #16457, #45327, #37707, #6056, #30540, #27768, #10214, #44642, #28455, #42308, #3286, #39095, #3750, #7226, #21297, #35597, #7445, #10672, #14842, #42087, #3527, #34922, #6982, #24756, #38871, #277, #42554, #17838, #10916, #17613, #24985, #31905, #32392, #32150, #28214, #7670, #11362, #21520, #3974, #28915, #18068, #513, #39562, #35375, #14374, #42996, #14621, #31463, #28693, #42772, #7917, #39314, #21067, #11132, #49, #17381, #25204, #21748, #35845, #4220, #13920, #18313, #743, #25441, #45568, #27992, #10438, #24513, #38622, #35150, #31682, #14143, #44122, #36076, #12488, #29144, #8348, #1188, #22416, #18982, #26112, #40227, #952, #19194, #32611, #11599, #5318, #4880, #12043, #26565, #26347, #33503, #36519, #36294, #19413, #15296, #29380, #25677, #1851, #15725, #43452, #15514, #11819, #4443, #8586, #33072, #40000, #1411, #22650, #36748, #25887, #15957, #43228, #4652, #21987, #39790, #29594, #43672, #5106, #33281, #1626, #29813, #18749, #43892, #12272, #30041, #40451, #8805, #22872, #40663, #36964, #18529, #15058, #8138, #22202, #32837, #19878, #24005, #27480, #2542, #23329, #45054, #9932, #2785, #40892, #30259, #41578, #12708, #34651, #12950, #5551, #38127, #27268, #6233, #30960, #23770, #13186, #9707, #44351, #6478, #13408, #3010, #37187, #45273, #20094, #33955, #33737, #13632, #31177, #41356, #30733, #17098, #34169, #16646, #37883, #2306, #20555, #27715, #44827, #37432, #9017, #23087, #16877, #9260, #26787, #19645, #5788, #2087, #27036, #16178, #16405, #20323, #34418, #30485, #44590, #41135, #9487, #23549, #37653, #6001, #22310, #24241, #32966, #7800, #21004, #20774, #1311, #4332, #18421, #15410, #3472, #11254, #36408, #43120, #38350, #14093, #32501, #41820, #1075, #27944, #39682, #6924, #10165, #14950, #8030, #11489, #850, #34867, #39443, #22097, #29033, #28167, #25328, #6695, #42886, #3229, #25569, #17563, #21875, #18875, #17319, #31409, #45516, #35965, #35096, #36187, #4547, #18640, #32727, #13869, #15187, #42041, #10387, #25788, #29273, #43350, #24462, #11716, #8241, #39902, #38570, #4770, #31635, #2, #33186, #41018, #23206, #8706, #22984, #36867, #43561, #33625, #44016, #1736, #15841, #30158, #1976, #5218, #9377, #36648, #43777, #29489, #1522, #19306, #33392, #40569, #37079, #12389, #5432, #12159, #19527, #26468, #26909, #26684, #22773, #2206, #40354, #44472, #16298, #16074, #26243, #19766, #30381, #37317, #15619, #5006, #12829, #29703, #23443, #29933, #25997, #37545, #44248, #40781, #5675, #12608, #9137, #33853, #19097, #5903, #19992, #34069, #11928, #2431, #8916, #40106, #8470, #22540, #24131, #38241, #21137, #23891, #31066, #10501, #17207, #13073, #34539, #6587, #35220, #20888, #2671, #13764, #27375, #16531, #34756, #27841, #31294, #20665, #41247, #13526, #41935, #3117, #2899, #45164, #44713, #16990, #27159, #45399, #38014, #27599, #38694, #30615, #7053, #23664, #41707, #41470, #10063, #10280, #24354, #38458, #9603, #6809, #37776, #6125, #45637, #34984, #3361, #20215, #17453, #28057, #31536, #30847, #13985, #9823, #6368, #34299, #42150, #24576, #20450, #16766, #44943, #13299, #7735, #18138, #21582, #35665, #4280, #21813, #25049, #29212, #10741, #17902, #3598, #21365, #39161, #10980, #14679, #11199, #32217, #25272, #31969, #39381, #578, #1020, #800, #42619, #22044, #25736, #35908, #18372, #43292, #28756, #32452, #14900, #4039, #42836, #8191, #7511, #42372, #17685, #28982, #43062, #39849, #11424, #38939, #7290, #31744, #32674, #11660, #24820, #25510, #39624, #340, #113, #7977, #35441, #36136, #3810, #4498, #18590, #22258, #15123, #14205, #28273, #14444, #28524, #8861, #43726, #4948, #26182, #40720, #37021, #44410, #15355, #1915, #26410, #29647, #9078, #19039, #23144, #1466, #8413, #33130, #18817, #15566, #33565, #12103, #22480, #12548, #29874, #5376, #32909, #19710, #1253, #16240, #5614, #30319, #30101, #43507, #33336, #33796, #9317, #1681, #8651, #44187, #4714, #16022, #26623, #12765, #29434, #43959, #37251, #40296, #36590, #2148, #26846, #22928, #22714, #19469, #40955, #36355, #36809, #40053, #25946, #11874, #5164, #19249, #15785, #12337, #40511, #38185, #13469, #24068, #27101, #20156, #45336, #45112, #27323, #37947, #3296, #16707, #41878, #34232, #41192, #13698, #23388, #10222, #30549, #31240, #20385, #16935, #38406, #45579, #44649, #34706, #6301, #27778, #16466, #20830, #6757, #34930, #34483, #13011, #41416, #19937, #37716, #30792, #9765, #6531, #27539, #20611, #9546, #2606, #24300, #41643, #23832, #2842, #17390, #44884, #31475, #13245, #23609, #13927, #37489, #28001, #6066, #42096, #31014, #9998, #5849, #34013, #3064, #17154, #2368, #14849, #3539, #7925, #25451, #21995, #39103, #10924, #3980, #15066, #3756, #17625, #10447, #17845, #284, #32618, #24992, #58, #14151, #38633, #39570, #18538, #31691, #18077, #35605, #24763, #24523, #7453, #28221, #21527, #42316, #21758, #32401, #36084, #28462, #6993, #32157, #4450, #38880, #28700, #31912, #7235, #14384, #28926, #11141, #961, #35160, #35852, #522, #42562, #43004, #21306, #11368, #35383, #10681, #14628, #21076, #42779, #7677, #25211, #39322, #751, #4229, #18321, #29153, #26572, #39797, #23094, #12496, #37194, #36972, #4658, #40237, #40669, #16186, #8594, #15521, #5325, #11607, #8812, #40460, #19652, #36301, #5112, #19420, #33081, #15303, #1860, #33512, #29821, #36531, #26356, #43903, #9024, #43458, #1195, #32847, #12050, #25685, #29601, #8145, #19201, #18989, #22660, #33746, #22208, #2096, #18757, #43679, #22422, #26122, #36757, #1633, #15732, #29386 ),
 ( #33288, #12280, #22880, #1419, #5561, #11825, #25895, #43235, #40006, #15967, #4888, #30048, #44131, #8356, #37892, #12959, #6243, #44834, #27725, #27488, #23558, #3019, #6704, #2793, #20333, #24250, #41367, #34426, #45063, #41142, #45281, #17105, #23779, #44597, #20565, #31187, #24014, #16412, #5798, #13641, #33963, #10172, #34177, #26794, #41827, #16885, #41586, #6485, #13418, #30967, #9942, #19884, #38358, #34659, #20781, #12714, #34875, #9714, #9495, #9268, #3238, #38134, #30267, #44358, #37661, #13195, #40899, #23334, #37438, #2549, #2314, #30492, #27044, #6010, #20103, #16655, #30740, #27275, #28646, #18022, #7400, #42047, #14326, #42724, #35551, #35331, #32099, #28173, #32341, #35795, #10869, #31641, #7623, #18269, #11088, #3480, #38577, #4174, #21014, #42947, #21251, #13875, #697, #3927, #14570, #39267, #468, #21474, #25158, #6931, #14793, #21699, #11315, #45523, #7869, #28403, #42266, #10395, #21947, #24935, #39051, #36033, #24703, #31860, #25392, #28867, #27951, #3708, #39512, #17328, #31417, #17570, #24470, #10626, #35104, #9, #14100, #38825, #7177, #17795, #42503, #231, #29554, #11779, #39958, #18486, #25850, #32563, #33032, #15251, #36472, #22830, #907, #5278, #43184, #8304, #32790, #22368, #4835, #15475, #43629, #15011, #40173, #29099, #11554, #12224, #18938, #1371, #36924, #33241, #26303, #11996, #36247, #40413, #1142, #29339, #25635, #8763, #22603, #43411, #26062, #8537, #39747, #36705, #5063, #19155, #1583, #15683, #29763, #43840, #19372, #8097, #4605, #4395, #22157, #18700, #7330, #11021, #7552, #28569, #21628, #28317, #35711, #14490, #43105, #42874, #38980, #18409, #22085, #18186, #4090, #39668, #25087, #32261, #21861, #619, #3855, #42658, #25554, #21406, #32488, #10788, #17725, #35951, #45677, #838, #7099, #7783, #39201, #14722, #14937, #36175, #21179, #11241, #28796, #4317, #38739, #11474, #29021, #8016, #25315, #388, #39427, #4535, #35481, #35259, #14029, #17946, #32016, #18628, #28098, #3638, #31788, #42194, #10542, #24618, #158, #14249, #42417, #24863, #32715, #29688, #4757, #43764, #36395, #44003, #8903, #12593, #4990, #1061, #12144, #26670, #15395, #5204, #40093, #1297, #22525, #37066, #33377, #40767, #11704, #12377, #22758, #25985, #5419, #29476, #19512, #43548, #18861, #11914, #15170, #8454, #29918, #36635, #32951, #22970, #26227, #1722, #29259, #16062, #43336, #9125, #1963, #23192, #26454, #39887, #40341, #30145, #5662, #8693, #19082, #40555, #25776, #33611, #44235, #37301, #8229, #36853, #22298, #33172, #1509, #15604, #19292, #15826, #13059, #2885, #6351, #17194, #19981, #23432, #9364, #41004, #23652, #16286, #34057, #27146, #37763, #34527, #9811, #20435, #37533, #16517, #45385, #2194, #10265, #30834, #44698, #44459, #24342, #27363, #41458, #38446, #41233, #34282, #13748, #16977, #30367, #6112, #23878, #19754, #24116, #5892, #31053, #30598, #33840, #37998, #45152, #13514, #27587, #12816, #16753, #41691, #10047, #20202, #2655, #26896, #44928, #2417, #38227, #9592, #13286, #41921, #6573, #20652, #34744, #3104, #31282, #27826, #3796, #10966, #25035, #31520, #4022, #17439, #42137, #35892, #35425, #42606, #43047, #11184, #18358, #38927, #21123, #4267, #99, #14191, #10488, #32439, #564, #31731, #325, #28260, #20875, #39145, #21348, #24806, #7278, #7496, #21567, #42359, #787, #13970, #35207, #6797, #24563, #10727, #17887, #31955, #14428, #28508, #35651, #3583, #18123, #32201, #14887, #14666, #28742, #25255, #28965, #42823, #39365, #11408, #7719, #21799, #25495, #17670, #34972, #3346, #45623, #28043, #38679, #7037, #33947, #25723, #15107, #12939, #43275, #20085, #43494, #36120, #23539, #12700, #37423, #16396, #9250, #44344, #40885, #29195, #41124, #30475, #34159, #22243, #26779, #1234, #8178, #29422, #44579, #23319, #2531, #18577, #5780, #30252, #32890, #27026, #36340, #9477, #4699, #11646, #18800, #22031, #15341, #19867, #11861, #39836, #37642, #33118, #2298, #4485, #5992, #32660, #16636, #30724, #44818, #13175, #1003, #36574, #39607, #7964, #4929, #25934, #40041, #8398, #22466, #19026, #1454, #16170, #34855, #3460, #17087, #45044, #31626, #20993, #13858, #20545, #10376, #27934, #24685, #27470, #30949, #16868, #2776, #31166, #23761, #41568, #34641, #45261, #42030, #17309, #24452, #13399, #23993, #17554, #3218, #13622, #41809, #7159, #2998, #24561, #38116, #9921, #14083, #27256, #28158, #34407, #35086, #24232, #20763, #42251, #3692, #6469, #38558, #10156, #10608, #20313, #38803, #21234, #35314, #38340, #27705, #31399, #31844, #6686, #45504, #41347, #6912, #17779, #216, #9696, #37874, #6222, #42483, #43398, #22353, #7383, #7850, #39494, #28631, #14309, #11298, #32079, #25376, #18006, #25618, #36230, #39944, #32325, #28381, #21928, #36457, #39034, #39730, #4377, #7607, #18685, #42709, #32774, #25141, #447, #11073, #10850, #39254, #11536, #21684, #14552, #4591, #36013, #29081, #24920, #11764, #21459, #8289, #29324, #4820, #8078, #35537, #18467, #25831, #33016, #32546, #679, #22141, #3912, #1122, #15234, #18921, #35778, #892, #4155, #18249, #14779, #28851, #42932, #14995, #43169, #30203, #33672, #44523, #1566, #5048, #36688, #22585, #5260, #43609, #15663, #8748, #19352, #16117, #37123, #2022, #19139, #43821, #23263, #23029, #33436, #15891, #26967, #40397, #19812, #12206, #33226, #37364, #1355, #33895, #8520, #9188, #44063, #40609, #16344, #23489, #29743, #12648, #29977, #5725, #40154, #12881, #30424, #41063, #12429, #1780, #8960, #5943, #22814, #26285, #15458, #36906, #26508, #37589, #5479, #19578, #44293, #29535, #9421, #20034, #26728, #40830, #2249, #11976, #26043, #31112, #6172, #45208, #37822, #45451, #10328, #14037, #6417, #34111, #13571, #28105, #16817, #6637, #41518, #2722, #23940, #38504, #34804, #24628, #27646, #13346, #13122, #38748, #41757, #10107, #7107, #9870, #2945, #42202, #3166, #30668, #20499, #24183, #2478, #6856, #20261, #31343, #44990, #16585, #20710, #13811, #17257, #38290, #27202, #27888, #41986, #24402, #34589, #17034, #44765, #20938, #41296, #35033, #38061, #3410, #10549, #9646, #23711, #34353, #17503, #27421, #31581, #45684, #30895, #39438, #166, #18416, #31796, #10797, #4542, #4098, #11249, #11711, #25563, #32722, #7560, #35489, #18636, #14500, #28577, #24870, #1070, #14945, #395, #14729, #42665, #35266, #25323, #35721, #39208, #18194, #21870, #7792, #11028, #15178, #28325, #3864, #21187, #38987, #25094, #32269, #627, #28803, #42881, #35958, #17954, #4325, #32495, #29267, #845, #29028, #39676, #43344, #43115, #11483, #39894, #8023, #22092, #36182, #32025, #3645, #17732, #14257, #42425, #7337, #21413, #12091, #4487, #39609, #36797, #22033, #43946, #22245, #14889, #1669, #36576, #15556, #40282, #33120, #22468, #19028, #7966, #19238, #8636, #12324, #789, #1456, #8400, #43049, #15343, #29636, #4931, #36342, #32892, #28967 ),
 ( #29861, #4701, #32662, #15774, #11648, #25725, #36122, #26398, #26169, #43277, #11863, #39838, #32441, #43715, #1237, #18802, #43496, #22699, #5154, #8180, #40499, #25497, #1005, #18360, #18579, #25936, #40043, #33325, #8850, #22918, #37009, #15109, #11410, #29197, #2828, #2592, #44397, #23817, #27524, #23596, #27085, #45097, #16451, #12998, #20140, #16225, #20372, #37928, #44634, #19693, #41403, #6285, #44870, #37236, #26610, #34467, #9064, #31000, #9304, #1900, #16920, #37702, #16693, #27309, #34217, #9532, #6051, #40710, #13455, #9753, #41624, #33551, #9981, #30535, #30303, #30091, #24051, #41178, #30779, #5363, #12752, #19924, #19458, #13232, #16009, #23373, #44173, #12536, #23132, #5601, #33785, #26832, #2136, #40939, #37477, #5838, #33999, #2352, #3521, #17374, #17140, #28687, #43, #14136, #42765, #45560, #6975, #32143, #38865, #34692, #10430, #28208, #11126, #42546, #24284, #35368, #3280, #38170, #10666, #3743, #7219, #42302, #31224, #35144, #17831, #24749, #24507, #21060, #20597, #38615, #3050, #21291, #13913, #17606, #14614, #6519, #45321, #13682, #31675, #31458, #31899, #271, #14368, #28448, #27761, #10910, #41863, #10208, #21511, #24978, #39089, #38391, #7438, #3967, #35591, #6740, #18062, #27986, #42081, #20815, #507, #34914, #5049, #19353, #33227, #39308, #29978, #40399, #43822, #12207, #26509, #44065, #1567, #5727, #32385, #40155, #25195, #43610, #15664, #29745, #36907, #33438, #8749, #1781, #8521, #15892, #22815, #23264, #23030, #19140, #44294, #2250, #12430, #40610, #19813, #5261, #8961, #37125, #36690, #40832, #12649, #5480, #22586, #16118, #26729, #19579, #11977, #737, #9189, #29536, #33896, #26286, #21741, #37365, #33674, #2024, #30204, #16345, #30425, #44525, #14836, #7663, #35838, #4214, #18307, #26045, #6419, #17505, #6174, #5944, #12882, #20262, #2723, #35034, #13347, #2479, #16586, #41064, #41987, #20939, #20035, #20501, #38062, #27203, #26968, #9871, #30669, #23941, #44766, #24185, #34805, #38505, #30896, #9423, #34590, #6857, #41297, #31113, #34354, #9647, #16819, #17258, #13572, #3411, #37590, #38291, #2946, #44991, #31344, #23712, #45452, #37823, #13124, #27422, #23490, #41519, #10108, #17035, #45209, #3167, #27647, #41758, #34112, #10329, #6638, #31583, #27890, #20711, #13812, #24403, #24629, #3646, #17733, #38749, #10550, #21188, #45685, #35268, #14038, #28106, #7108, #42203, #19630, #33270, #15503, #2073, #37175, #30027, #36736, #26555, #44112, #40880, #43659, #1399, #33062, #18968, #1616, #39988, #12030, #5094, #15715, #12476, #33489, #40653, #29583, #40210, #33724, #19403, #29800, #12257, #23314, #19184, #16165, #8573, #26098, #30247, #43439, #44339, #4867, #5533, #40441, #36954, #12694, #19861, #22638, #9006, #26337, #26774, #36503, #9243, #37417, #15945, #23076, #5774, #33941, #1835, #2293, #43878, #16391, #11807, #25876, #8336, #22400, #8793, #22861, #5307, #20987, #38108, #6464, #35081, #37869, #45038, #24448, #31159, #27020, #2771, #20542, #3454, #34848, #16630, #27699, #41341, #30470, #2993, #41803, #45256, #34636, #9472, #27464, #10152, #17081, #16863, #13393, #12933, #30944, #41119, #13616, #6216, #41562, #6907, #44573, #23534, #37636, #9916, #9691, #23987, #24227, #38335, #6681, #5987, #20757, #20079, #34154, #13854, #3212, #17303, #2525, #31392, #42026, #45497, #44813, #27931, #23755, #20308, #30717, #10372, #38552, #34400, #13170, #27250, #31623, #21681, #32073, #35533, #3907, #18245, #35772, #39029, #43165, #24680, #31841, #17550, #35311, #7379, #24916, #28626, #25137, #14547, #39251, #211, #7603, #42706, #14991, #14776, #10843, #36010, #39726, #4151, #32320, #11531, #11070, #674, #28847, #28376, #32542, #4373, #42928, #14305, #7846, #18462, #11293, #3688, #38797, #889, #21231, #25614, #21455, #14079, #29078, #42478, #21923, #18002, #17775, #25372, #39330, #39487, #8074, #22137, #36225, #28154, #42246, #10604, #7154, #33668, #1117, #30198, #19572, #44288, #44057, #11761, #1562, #2017, #23257, #15660, #22582, #12425, #18680, #15886, #1775, #26724, #43394, #12202, #26504, #40151, #22348, #8956, #40605, #36903, #43605, #33431, #5256, #16113, #4814, #8284, #39940, #25827, #8515, #15231, #18917, #11971, #36684, #19348, #40393, #29973, #36451, #1352, #23025, #26281, #5044, #19135, #12644, #26038, #37118, #15455, #33012, #5476, #4589, #40825, #29531, #9183, #29737, #43816, #32771, #29318, #33223, #8744, #22811, #41748, #30419, #34796, #6631, #3159, #20255, #37816, #30889, #41981, #30660, #44516, #37358, #44759, #27195, #13805, #6165, #26960, #41058, #19807, #20704, #45444, #12876, #44983, #16810, #5938, #5719, #34346, #9415, #2715, #23483, #2939, #13564, #17250, #9640, #33890, #13338, #31337, #20028, #9862, #13116, #34105, #41288, #10101, #38053, #27883, #16338, #17026, #27415, #23704, #24176, #10322, #41512, #37584, #2471, #2243, #16578, #23934, #6411, #20493, #34582, #31103, #45202, #27640, #38284, #35483, #28099, #35713, #621, #4319, #42419, #24395, #21408, #18411, #7100, #42660, #31790, #38740, #14251, #28798, #25089, #32490, #3403, #4092, #14492, #17727, #42876, #21181, #11243, #35261, #42195, #3640, #6849, #160, #21630, #28319, #10543, #14724, #17948, #39203, #20929, #7785, #35027, #840, #39429, #14939, #18188, #31575, #3857, #21863, #43107, #32018, #10790, #32263, #38497, #25317, #35953, #29023, #17497, #390, #45678, #24865, #24619, #14030, #38982, #11023, #7332, #7554, #28571, #8905, #11706, #15172, #1063, #32717, #15397, #8018, #25778, #18863, #29478, #26229, #1511, #12146, #29261, #8231, #33379, #33174, #43550, #25987, #37068, #4759, #29920, #22300, #43338, #1724, #11476, #44005, #18630, #19294, #8456, #4992, #26456, #33613, #39889, #22760, #40095, #15828, #4537, #22972, #40557, #5421, #22527, #11916, #19084, #16064, #32953, #36397, #25556, #1299, #36637, #15606, #19514, #1965, #30147, #29690, #43766, #40343, #39670, #8695, #36855, #22087, #5206, #12379, #36177, #44700, #33842, #2196, #26672, #27589, #6575, #37303, #37765, #23654, #12818, #44237, #41235, #16288, #9594, #30369, #9813, #20437, #24118, #16519, #12595, #6114, #38229, #26898, #16755, #5894, #41006, #34059, #2887, #44930, #20654, #23194, #23880, #34284, #37535, #16979, #9366, #31055, #23434, #44461, #19983, #40769, #2419, #41460, #30600, #13061, #34529, #20204, #13288, #9127, #41693, #5664, #34746, #13516, #3106, #38000, #19756, #2658, #10050, #17196, #30836, #27148, #6354, #27365, #45154, #28510, #7721, #24344, #38929, #7498, #21125, #3348, #35653, #25037, #17889, #24565, #14430, #31957, #28744, #31522, #34974, #20877, #6799, #35209, #27828, #45625, #38681, #3585, #327, #21350, #42608, #17441, #28045, #21569, #7280, #17672, #101, #11186, #7039, #4024, #42139, #13972, #18125, #31284, #32203, #38448, #39147, #28262, #24808, #566, #21801, #10490, #10968, #14193, #14668 ),
 ( #42825, #25257, #35427, #31733, #39367, #35894, #4269, #42361, #10729, #45387, #3798, #13750, #41923, #10267, #13156, #1654, #26379, #20064, #43928, #33309, #29844, #18780, #30703, #2510, #37853, #11628, #20294, #40264, #8381, #8164, #34386, #36779, #5135, #2756, #36554, #43699, #6202, #12307, #25706, #1439, #19222, #29175, #44799, #15324, #40481, #40027, #43258, #15756, #22901, #37621, #27235, #22227, #26148, #41327, #39818, #15540, #12072, #36323, #8618, #4684, #32870, #4912, #22683, #1217, #29406, #43478, #11846, #25917, #22450, #19009, #33101, #20972, #35068, #41549, #14068, #27451, #6451, #199, #45485, #6893, #7368, #21219, #28364, #3199, #31145, #14291, #10140, #24215, #20530, #42465, #10591, #41790, #10360, #38323, #30931, #3442, #31380, #34836, #17290, #17538, #31612, #6669, #10831, #23974, #38096, #20744, #13378, #45242, #13841, #27920, #45715, #28140, #42235, #34624, #13603, #38783, #38541, #42015, #24436, #24903, #24667, #35300, #27686, #2981, #7140, #16851, #3677, #17068, #17764, #31829, #39018, #21444, #35520, #45025, #9902, #32531, #8271, #42694, #1339, #18906, #15443, #878, #4362, #43154, #8504, #42916, #11059, #3896, #11282, #39476, #26028, #18452, #39239, #7592, #32061, #33000, #11960, #25126, #11520, #29066, #18232, #17988, #14981, #21668, #25604, #35760, #15220, #25816, #29520, #21911, #432, #39714, #43594, #32307, #22126, #25359, #662, #7834, #22336, #4578, #40139, #28612, #29308, #8064, #35998, #36438, #14763, #4802, #28836, #4139, #36214, #14535, #18670, #1106, #32759, #43381, #39928, #11749, #22572, #33214, #20019, #1551, #16566, #5928, #30649, #30410, #43807, #33656, #34095, #9631, #2007, #8945, #44505, #5035, #2233, #33880, #13106, #29729, #44278, #12864, #26496, #8735, #41047, #26947, #23245, #29963, #19796, #37348, #2462, #5247, #40384, #26271, #12191, #9405, #22801, #44747, #40596, #15649, #27187, #9168, #16328, #23473, #5709, #40813, #37573, #19337, #41278, #36675, #19127, #33422, #1764, #16104, #15874, #44047, #12415, #12635, #26714, #23013, #37108, #5466, #19561, #30188, #20244, #41738, #45434, #28307, #28087, #9853, #20921, #34571, #23695, #41971, #35017, #24385, #13797, #2703, #20696, #3395, #10313, #10091, #38274, #6156, #24167, #34335, #27874, #45194, #34787, #148, #37807, #14238, #30878, #6621, #2931, #3150, #17241, #38489, #6841, #16799, #17488, #44974, #13328, #7088, #31327, #31567, #42405, #42183, #35250, #45667, #38044, #21169, #17018, #31095, #27405, #3628, #14019, #13556, #10533, #27629, #41502, #24609, #38726, #17715, #31778, #23923, #6402, #20484, #36385, #17936, #25078, #10776, #28558, #610, #18175, #21847, #18400, #39417, #32480, #39192, #830, #25305, #8220, #8009, #4076, #29249, #32941, #29012, #14929, #4747, #35940, #43095, #25544, #21618, #25767, #43326, #4308, #7542, #1052, #11694, #4527, #42649, #376, #32005, #14711, #7321, #35700, #32251, #28787, #39657, #11461, #22075, #14478, #42865, #32706, #36166, #11232, #7769, #18851, #18619, #39879, #15158, #11011, #22289, #24853, #1287, #15386, #29465, #38971, #21397, #35471, #3845, #19072, #9111, #26443, #2182, #36624, #40990, #12801, #9350, #40542, #43990, #37053, #2402, #36842, #4979, #43538, #5192, #33366, #19970, #12367, #33160, #1497, #25976, #26883, #5880, #15595, #5405, #22957, #12133, #11905, #8892, #29677, #19501, #43755, #23180, #19742, #23420, #15815, #40084, #33598, #37521, #26215, #16051, #19279, #40330, #1711, #16274, #44221, #34045, #22514, #37288, #1949, #29905, #30353, #8683, #44445, #22747, #30133, #12579, #8444, #26656, #40752, #5648, #33829, #16503, #30822, #27352, #44685, #20419, #13043, #2873, #34514, #16964, #23865, #27133, #16739, #31041, #30583, #41446, #44916, #41222, #9579, #23639, #37750, #6099, #2642, #20189, #34269, #13274, #9797, #37982, #6337, #12720, #19427, #9274, #26801, #23564, #26362, #29827, #22666, #44137, #2101, #30745, #30500, #12286, #23341, #36978, #26128, #44365, #37444, #40904, #16191, #5119, #23101, #5804, #19890, #12502, #40676, #8600, #26578, #36763, #30272, #1866, #37200, #2554, #40243, #16661, #33294, #9030, #5331, #5566, #19658, #33968, #2320, #19207, #16418, #1639, #15740, #9500, #33751, #44602, #44839, #12964, #37667, #27050, #40466, #6017, #33517, #15972, #43909, #20108, #41148, #30054, #34184, #8818, #22887, #17333, #27730, #31192, #45288, #13880, #31422, #34664, #38831, #20339, #27493, #13202, #30972, #3024, #20569, #24255, #20786, #41832, #34880, #41593, #3245, #10178, #10632, #10400, #6490, #31646, #35336, #45528, #27956, #7181, #38363, #42052, #24476, #24021, #28179, #14, #6709, #9948, #3485, #14105, #6938, #45069, #34432, #42271, #16891, #21256, #17110, #9720, #24709, #38583, #21019, #35109, #17575, #3713, #17800, #2799, #31866, #27280, #41373, #23785, #37899, #6249, #38139, #13424, #13646, #7875, #21952, #4840, #7629, #14799, #39963, #912, #18275, #15015, #36037, #29104, #3933, #42730, #22161, #4400, #4180, #28873, #25854, #39274, #18704, #11094, #18028, #36251, #237, #32795, #7406, #8100, #42954, #39519, #15254, #22372, #21480, #11557, #11321, #4608, #39057, #43415, #29343, #11783, #25399, #703, #18491, #18942, #21707, #35558, #14333, #35802, #32348, #36477, #32567, #32106, #474, #28411, #8309, #42509, #14577, #43187, #25638, #28652, #10875, #39750, #25165, #1147, #24941, #44313, #9211, #12904, #5282, #33036, #29997, #26990, #15687, #5505, #8766, #1587, #22834, #37388, #33695, #41090, #12001, #12667, #23047, #26308, #5744, #29768, #19831, #43846, #5067, #12228, #15479, #36928, #30222, #19376, #19159, #23286, #26529, #2043, #29558, #16363, #43633, #9443, #2266, #23507, #26748, #40178, #44084, #30443, #5962, #12449, #33459, #40849, #1375, #33914, #44544, #37609, #26066, #40628, #8541, #1805, #33244, #22608, #36709, #19599, #15911, #16136, #8979, #37146, #20281, #23730, #9665, #41316, #23961, #16604, #34373, #27438, #20729, #37843, #16839, #42001, #10126, #38082, #34608, #45700, #13365, #38524, #30916, #6190, #10344, #20052, #6876, #27222, #27905, #17053, #13589, #35053, #42220, #2743, #31363, #2966, #24419, #13143, #17523, #3426, #31597, #31131, #20517, #27671, #24648, #41537, #45011, #34130, #9888, #6439, #10571, #45228, #24200, #38307, #2498, #14053, #28123, #6655, #34822, #3185, #17273, #30688, #45470, #13828, #20955, #38765, #44789, #29047, #32741, #25109, #7123, #4118, #1087, #35504, #25340, #14517, #21428, #42679, #11500, #7812, #15200, #31812, #18433, #42898, #414, #25582, #3879, #39696, #17971, #24887, #32043, #35283, #28595, #4342, #11043, #39001, #43133, #643, #21891, #3660, #36198, #17748, #29287, #22108, #43364, #860, #14274, #18213, #4561, #25799, #32287, #39223, #14963, #21202, #32512, #8043, #11729, #181, #14744, #18652, #7576, #7351, #28344, #42444, #39456, #21652, #35978, #10814, #35739, #28818, #11265 ),
 ( #33405, #19321, #8484, #39912, #36880, #11942, #5230, #43574, #5447, #16087, #19780, #12173, #8254, #1749, #33865, #22554, #12400, #1534, #36659, #29714, #44262, #40581, #2218, #18886, #19542, #29944, #33197, #12620, #5019, #26698, #19110, #26010, #15631, #22320, #43791, #37092, #26254, #40119, #30171, #15856, #8927, #36420, #23225, #4784, #16312, #9153, #30394, #33637, #1321, #44028, #37330, #12843, #26479, #40367, #1990, #32981, #40795, #5692, #44487, #15424, #22997, #29502, #8719, #22785, #31308, #20680, #13539, #20229, #10076, #27613, #25007, #27173, #30632, #16547, #2445, #30863, #23457, #41261, #34317, #44957, #41722, #17003, #24147, #44727, #23679, #3133, #2913, #13314, #41485, #7467, #2686, #45416, #37790, #13090, #17222, #26927, #13777, #34081, #34770, #23908, #20465, #41952, #3993, #9617, #38256, #9839, #27856, #20004, #39118, #10293, #21539, #38029, #27390, #6139, #16783, #35621, #41030, #18091, #6384, #32173, #34554, #31080, #536, #9389, #45178, #6602, #37556, #5914, #7691, #12063, #29613, #26137, #43248, #15077, #8155, #19214, #7938, #21771, #14641, #22005, #4460, #36771, #29164, #4242, #18332, #42795, #43690, #22674, #35865, #22218, #39808, #28938, #28714, #11619, #32412, #25697, #761, #25908, #36543, #40252, #32631, #11155, #36311, #8609, #43015, #32857, #36095, #11380, #18549, #19001, #15315, #5126, #39337, #40017, #4673, #974, #33093, #25462, #1430, #39581, #14862, #18771, #25225, #1207, #11837, #29397, #43469, #4902, #8369, #22438, #15532, #33301, #43916, #27285, #16667, #41378, #41156, #8825, #44372, #44846, #20344, #12727, #19665, #9507, #15747, #12971, #44610, #23791, #40473, #9280, #23571, #37209, #19433, #6025, #37676, #33976, #40683, #30507, #2327, #13208, #1873, #5338, #36985, #22893, #5573, #12295, #15980, #9037, #33758, #16426, #37452, #27060, #33525, #44145, #20116, #23349, #2110, #16199, #9727, #23107, #34192, #29835, #37903, #30064, #30279, #26585, #26807, #40913, #5811, #19899, #26371, #2562, #12509, #30752, #6257, #1646, #24481, #24946, #38834, #240, #20790, #3028, #31870, #27734, #41838, #38144, #14337, #28182, #13653, #27960, #10183, #2804, #38587, #3249, #6713, #34885, #35114, #6943, #24259, #28415, #41598, #17115, #34438, #6495, #38367, #17341, #45533, #42056, #31427, #10404, #31196, #21026, #13886, #42513, #31649, #3491, #7187, #10878, #17579, #17, #39061, #14108, #42274, #10635, #45294, #3716, #21261, #24716, #35340, #17803, #7409, #16895, #20573, #9955, #30976, #34669, #45074, #13429, #27499, #24025, #39756, #18708, #43419, #36254, #25642, #22165, #11098, #22376, #11786, #1379, #3936, #12006, #32572, #706, #477, #26069, #29107, #43191, #40183, #28877, #36041, #15482, #4612, #18031, #39524, #11560, #21484, #25857, #7632, #32798, #32352, #35561, #8104, #1152, #15257, #29346, #14582, #18494, #39967, #8312, #7879, #4404, #32112, #21955, #28656, #36481, #42957, #916, #43636, #42734, #25168, #15018, #14803, #39278, #21710, #4846, #18945, #35807, #11324, #33041, #29562, #4183, #18278, #25402, #30226, #13147, #12909, #40419, #5748, #19379, #8548, #26752, #19837, #9218, #44317, #33247, #5510, #33919, #40855, #26533, #23052, #36712, #40631, #5072, #12672, #30002, #19606, #30696, #22612, #44792, #15691, #8983, #33463, #37150, #33699, #23293, #37394, #1592, #2270, #19163, #43851, #37613, #2049, #16368, #27228, #26997, #20055, #16143, #22839, #5966, #1811, #15918, #12234, #34133, #30446, #44089, #44548, #12454, #29774, #41093, #9448, #23512, #2501, #16608, #26313, #8771, #36932, #5286, #9892, #41320, #13371, #31136, #2971, #6662, #3192, #24205, #17281, #23966, #31370, #10132, #38774, #38531, #34616, #14060, #17756, #13834, #45478, #35291, #20735, #27911, #10352, #6443, #10580, #28132, #34828, #38088, #31604, #42227, #35060, #27443, #16843, #24658, #45018, #21210, #45234, #37846, #7132, #42008, #6885, #17531, #24428, #20962, #3434, #30922, #3669, #31820, #191, #13594, #9670, #38315, #14283, #20522, #23735, #17060, #27677, #41782, #6194, #20286, #34379, #2748, #41541, #18443, #21661, #32750, #42685, #1097, #39231, #422, #25117, #10823, #7584, #25595, #11052, #14527, #4569, #21903, #43143, #24895, #11740, #39009, #8263, #43374, #22328, #22117, #35512, #25350, #25807, #1330, #39464, #652, #36205, #42456, #39705, #8052, #4793, #21436, #35987, #18660, #18222, #28603, #15211, #29299, #14972, #35751, #11509, #29057, #39920, #4130, #32051, #17981, #3887, #32298, #7360, #14753, #28827, #42907, #36429, #32521, #18896, #11274, #7824, #32992, #4353, #869, #28352, #41038, #8729, #33873, #26264, #33208, #37341, #15434, #2226, #22565, #23235, #12409, #8936, #30402, #37565, #36669, #26706, #44039, #19790, #8494, #12857, #44496, #26938, #26489, #15866, #23007, #20012, #22794, #5029, #29512, #36889, #5241, #5922, #29955, #19119, #1545, #43584, #9399, #23466, #15640, #37101, #40590, #29723, #11952, #5457, #43801, #19552, #12183, #40805, #5703, #34088, #26020, #33648, #2000, #33414, #1758, #16096, #30180, #19331, #40130, #40378, #44271, #12628, #9162, #16321, #9846, #13548, #10084, #31088, #24157, #30870, #38267, #17011, #45659, #45425, #41493, #20912, #24600, #20688, #6613, #42175, #27622, #34779, #17232, #13322, #17478, #35009, #41730, #16793, #38481, #3385, #41961, #34325, #23688, #31559, #6148, #28079, #6393, #44740, #14009, #3141, #13787, #24377, #31319, #27866, #10304, #37799, #10524, #6832, #38718, #30642, #7078, #21159, #27398, #27182, #2454, #16557, #13098, #41270, #23916, #45186, #9625, #20238, #2696, #20477, #44966, #38037, #34564, #2922, #32472, #368, #35242, #7761, #821, #35931, #25295, #14229, #32242, #14921, #21838, #7534, #4068, #17708, #21608, #31769, #11224, #11003, #602, #11686, #3620, #25759, #42398, #35691, #14469, #18166, #14703, #39407, #4301, #28298, #29002, #140, #24844, #18611, #28779, #18392, #39871, #39648, #1043, #42857, #3836, #32696, #28548, #42642, #38963, #15150, #43086, #25070, #11452, #39184, #25535, #17926, #7313, #8001, #22067, #36157, #10767, #29239, #21390, #43317, #4519, #8212, #35463, #31996, #19270, #19731, #40981, #33358, #40321, #16042, #36376, #33589, #19491, #44434, #15378, #29896, #44212, #12124, #40074, #26646, #30124, #8883, #15587, #5396, #22948, #33819, #22506, #25968, #11896, #43530, #26207, #18843, #36615, #29670, #8674, #37045, #12357, #1939, #8436, #19063, #12571, #43981, #22739, #36832, #2172, #43745, #40743, #33152, #4970, #9100, #22281, #23169, #29457, #37279, #1701, #15806, #5637, #12789, #1489, #16264, #5184, #30342, #26434, #26871, #4739, #32933, #40534, #1278, #2864, #13948, #2633, #2392, #9340, #16730, #44907, #31497, #9789, #44676, #13033, #37512, #38427, #17419, #16491, #16955, #34505, #23630, #23410, #6328, #27123, #20409, #41214, #20632, #31262, #34951, #27344, #5871, #31033, #3322, #37739, #27563 ),
 ( #20853, #37971, #23855, #45132, #28023, #30813, #30573, #19961, #13266, #41437, #45601, #13490, #9570, #6091, #34035, #6777, #20179, #34258, #41668, #10025, #24091, #38206, #6554, #34725, #3084, #17175, #45364, #13726, #27803, #41898, #10244, #24323, #22014, #24788, #14650, #3777, #10705, #31936, #772, #42806, #4469, #21105, #7701, #32185, #35406, #14872, #38905, #28946, #7258, #14172, #21329, #24543, #17868, #39347, #306, #28242, #18341, #35631, #11165, #38656, #25474, #7014, #36105, #11390, #18560, #35876, #3563, #39127, #39592, #15089, #7479, #14408, #4251, #10467, #21781, #32422, #32642, #35187, #4003, #43027, #28489, #42337, #7947, #984, #28726, #42587, #25237, #42117, #17651, #10947, #81, #31712, #25019, #21548, #18103, #546, #39380, #22257, #4713, #21363, #10979, #39159, #22711, #30316, #33563, #1913, #16021, #8412, #44185, #4944, #36808, #26180, #40294, #37249, #19708, #6064, #6756, #41640, #38184, #13926, #21075, #20153, #28000, #17389, #6530, #13244, #34929, #45576, #38405, #30791, #34230, #31472, #2605, #24522, #2841, #41191, #42095, #17153, #41877, #20829, #13696, #3063, #45334, #16705, #10446, #3294, #38632, #27100, #35158, #9996, #37943, #23608, #3537, #20610, #34705, #17622, #6300, #13468, #6991, #27774, #9545, #16934, #31239, #44648, #13010, #44883, #10221, #9764, #37715, #24299, #27322, #41415, #20383, #34482, #24066, #31013, #45111, #27538, #519, #14150, #3979, #28220, #7676, #7451, #42778, #8144, #57, #22207, #38878, #18074, #10923, #32156, #28699, #35851, #4227, #10679, #28924, #42315, #21304, #15064, #14627, #21755, #36300, #36082, #43234, #11139, #283, #29151, #24991, #39101, #35380, #11605, #25448, #21526, #25209, #35604, #24762, #18320, #39321, #32400, #750, #14848, #43002, #11367, #25684, #7234, #14382, #31690, #3755, #39569, #7923, #21994, #4449, #18537, #32617, #28461, #959, #39796, #4657, #17844, #31911, #42560, #40897, #36970, #40457, #26792, #29819, #26353, #33509, #29599, #18755, #23092, #30264, #19199, #33079, #16183, #12048, #26120, #22421, #44356, #12493, #43677, #12278, #40234, #32843, #22878, #33286, #36755, #1631, #19418, #1857, #8591, #1194, #25894, #1416, #15301, #36526, #22657, #15730, #43900, #8810, #15965, #44128, #15519, #26570, #9022, #43457, #37192, #5558, #2094, #11824, #40005, #8355, #4885, #35046, #3421, #17516, #31807, #42438, #25057, #123, #20896, #42627, #7519, #349, #38465, #27849, #39169, #24362, #32226, #10509, #3126, #35673, #24828, #3820, #28532, #21373, #10751, #7298, #41946, #21593, #10989, #586, #34764, #42844, #17693, #45646, #31302, #11208, #14213, #28282, #25280, #13995, #21145, #14688, #35449, #17215, #24585, #42382, #6595, #4049, #6818, #17910, #17461, #20673, #38948, #31978, #14454, #18147, #45409, #31754, #28764, #13771, #38702, #34994, #3370, #7062, #30442, #38081, #23729, #45010, #6875, #9442, #2497, #30687, #20280, #41315, #34372, #2965, #17052, #31130, #37842, #45227, #16838, #10125, #45469, #3184, #24003, #16644, #3227, #38125, #35786, #21001, #25149, #28392, #10860, #32334, #39503, #35094, #7616, #224, #687, #10385, #28859, #42940, #11307, #24928, #17787, #39042, #45514, #10618, #14091, #13867, #21242, #3700, #7860, #31852, #7391, #3920, #27942, #25385, #42039, #18015, #32087, #29544, #1130, #18476, #15466, #22149, #43620, #8087, #15672, #36914, #12436, #18930, #32555, #11986, #26515, #15243, #22593, #25840, #29332, #39952, #5268, #29753, #8967, #29089, #43830, #8528, #33025, #19360, #26053, #33446, #12213, #36237, #899, #11544, #25627, #39737, #4598, #12891, #3596, #41074, #27311, #9065, #41625, #23133, #38171, #27525, #6520, #6287, #19696, #9533, #9982, #31225, #23597, #30536, #20373, #26612, #23818, #9754, #34693, #5602, #20141, #34469, #2353, #30304, #16921, #2829, #44871, #5839, #41404, #13233, #24053, #12753, #16226, #2137, #33786, #16453, #37237, #26833, #19925, #44635, #37929, #2593, #31001, #44399, #9305, #45099, #34219, #12999, #27087, #20598, #34000, #13456, #23375, #3051, #17141, #16694, #12537, #40940, #40711, #37478, #41179, #37703, #6052, #30780, #24508, #24285, #35839, #7220, #21292, #4215, #6976, #14137, #39310, #272, #41865, #17607, #35369, #18308, #3968, #31459, #42548, #10431, #45322, #17832, #10911, #14369, #3745, #38392, #42303, #24979, #31900, #31677, #28209, #27762, #44, #10209, #28449, #21061, #10667, #21742, #13683, #6741, #20816, #24750, #38616, #38866, #39090, #7439, #21513, #34915, #35592, #3281, #17375, #28688, #18063, #32144, #45561, #508, #11127, #14616, #13915, #42766, #35145, #3522, #27987, #25196, #7664, #42082, #25884, #39785, #738, #36515, #1183, #4648, #18743, #33069, #4876, #8134, #12267, #39557, #947, #32387, #4437, #22197, #36289, #43448, #39996, #15292, #8345, #15050, #22411, #29376, #29808, #29591, #25672, #5103, #8802, #18979, #1408, #26344, #11815, #15511, #43668, #43221, #1623, #19191, #12040, #29139, #22646, #33277, #26107, #18524, #7912, #15722, #36071, #40447, #32832, #28909, #43888, #40223, #8582, #36745, #11594, #22869, #36961, #5314, #14837, #42990, #11355, #25435, #21982, #32605, #13405, #30482, #27032, #34166, #30256, #34414, #37880, #12946, #33734, #9703, #20320, #13182, #5546, #40660, #6228, #23084, #45050, #23324, #15954, #2782, #37649, #16642, #41353, #2537, #23546, #20091, #9013, #16874, #23767, #27477, #1847, #9927, #44585, #44348, #44119, #24000, #41131, #9483, #38122, #26784, #33952, #41575, #30730, #30037, #37428, #5998, #19410, #30956, #19640, #44824, #12704, #33497, #27264, #12484, #26562, #37182, #2083, #16402, #16175, #40889, #5785, #2303, #9256, #19874, #34648, #28164, #27940, #17560, #28636, #20552, #42715, #13628, #38566, #31406, #6920, #3468, #10615, #24692, #31173, #3698, #17094, #41816, #35543, #35092, #42257, #11079, #10857, #18013, #20999, #20770, #3918, #45511, #13865, #10162, #32085, #222, #42037, #5370, #10383, #3006, #38810, #31632, #24459, #14089, #7166, #21240, #35320, #456, #27712, #34863, #6475, #24238, #17785, #31850, #14316, #28388, #42491, #45269, #14560, #38347, #25147, #21465, #6692, #24926, #3225, #39040, #17315, #7389, #25625, #898, #11770, #7614, #43404, #29330, #11984, #18257, #22147, #39950, #32553, #28857, #22359, #25838, #32781, #36021, #15241, #1128, #1362, #11305, #42938, #14785, #32331, #15001, #21691, #25383, #4384, #29088, #8295, #4597, #36464, #39500, #7858, #4826, #36236, #43175, #11543, #29543, #18474, #18928, #21936, #39736, #33024, #39259, #15465, #8085, #43618, #18692, #26052, #40163, #35784, #8527, #4163, #685, #39191, #27873, #32250, #4075, #609, #17714, #35249, #28306, #39416, #28086, #41970, #34786, #42182, #24608, #11231, #3627, #24384, #38488, #17240, #18174, #42864, #10312, #42404, #14237, #3394, #3149, #31777, #6840, #147, #20920, #375, #11010, #14710, #7087, #31326, #10775 ) ),
 .UNSPECIFIED., .T., .F., .T. ) 
 B_SPLINE_SURFACE_WITH_KNOTS ( ( 4, 3, 4 ),
 ( 3, 2, 2, 2, 2, 2, 2, 2, 2, 2, 2, 2, 2, 2, 2, 2, 2, 2, 2, 2, 2, 2, 2, 2, 2, 2, 2, 2, 2, 2, 2, 2, 2, 2, 2, 2, 2, 2, 2, 2, 2, 2, 2, 2, 2, 2, 2, 2, 2, 2, 2, 2, 2, 2, 2, 2, 2, 2, 2, 2, 2, 2, 2, 2, 2, 2, 2, 2, 2, 2, 2, 2, 2, 2, 2, 2, 2, 2, 2, 2, 2, 2, 2, 2, 2, 2, 2, 2, 2, 2, 2, 2, 2, 2, 2, 2, 2, 2, 2, 2, 2, 2, 2, 2, 2, 2, 2, 2, 2, 2, 2, 2, 2, 2, 2, 2, 2, 2, 2, 2, 2, 2, 2, 2, 2, 2, 2, 2, 2, 2, 2, 2, 2, 2, 2, 2, 2, 2, 2, 2, 2, 2, 2, 2, 2, 2, 2, 2, 2, 2, 2, 2, 2, 2, 2, 2, 2, 2, 2, 2, 2, 2, 2, 2, 2, 2, 2, 2, 2, 2, 2, 2, 2, 2, 2, 2, 2, 2, 2, 2, 2, 2, 2, 2, 2, 2, 2, 2, 2, 2, 2, 2, 2, 2, 2, 2, 2, 2, 2, 2, 2, 2, 2, 2, 2, 2, 2, 2, 2, 2, 2, 2, 2, 2, 2, 2, 2, 2, 2, 2, 2, 2, 2, 2, 2, 2, 2, 2, 2, 2, 2, 2, 2, 2, 2, 2, 2, 2, 2, 2, 2, 2, 2, 2, 2, 2, 2, 2, 2, 2, 2, 2, 2, 2, 2, 2, 2, 2, 2, 2, 2, 2, 2, 2, 2, 2, 2, 2, 2, 2, 2, 2, 2, 2, 2, 2, 2, 2, 2, 2, 2, 2, 2, 2, 2, 2, 2, 2, 2, 2, 2, 2, 2, 2, 2, 2, 2, 2, 2, 2, 2, 2, 2, 2, 2, 2, 2, 2, 2, 2, 2, 2, 2, 2, 2, 2, 2, 2, 2, 2, 2, 2, 2, 2, 2, 2, 2, 2, 2, 2, 2, 2, 2, 2, 2, 2, 2, 2, 2, 2, 2, 2, 2, 2, 2, 2, 2, 2, 2, 2, 2, 2, 2, 2, 2, 2, 2, 2, 2, 2, 2, 2, 2, 2, 2, 2, 2, 2, 2, 2, 2, 2, 2, 2, 2, 2, 2, 2, 2, 2, 2, 2, 2, 2, 2, 2, 2, 2, 2, 2, 2, 2, 2, 2, 2, 2, 2, 2, 2, 2, 2, 2, 2, 2, 2, 2, 2, 2, 2, 2, 2, 2, 2, 2, 2, 2, 2, 2, 2, 2, 2, 2, 2, 2, 2, 2, 2, 2, 2, 2, 2, 3 ),
 ( 0.000000000000000000, 0.5000000000000000000, 1.000000000000000000 ),
 ( 0.000000000000000000, 0.002272727272727272617, 0.004545454545454545234, 0.006818181818181817851, 0.009090909090909090468, 0.01136363636363636395, 0.01363636363636363570, 0.01590909090909090745, 0.01818181818181818094, 0.02045454545454545442, 0.02272727272727272790, 0.02500000000000000139, 0.02727272727272727140, 0.02954545454545454489, 0.03181818181818181490, 0.03409090909090908839, 0.03636363636363636187, 0.03863636363636363535, 0.04090909090909090884, 0.04318181818181818232, 0.04545454545454545581, 0.04772727272727272929, 0.05000000000000000278, 0.05227272727272726932, 0.05454545454545454281, 0.05681818181818181629, 0.05909090909090908977, 0.06136363636363636326, 0.06363636363636362980, 0.06590909090909090329, 0.06818181818181817677, 0.07045454545454545026, 0.07272727272727272374, 0.07499999999999999722, 0.07727272727272727071, 0.07954545454545454419, 0.08181818181818181768, 0.08409090909090909116, 0.08636363636363636465, 0.08863636363636363813, 0.09090909090909091161, 0.09318181818181818510, 0.09545454545454545858, 0.09772727272727273207, 0.1000000000000000056, 0.1022727272727272790, 0.1045454545454545386, 0.1068181818181818121, 0.1090909090909090856, 0.1113636363636363591, 0.1136363636363636326, 0.1159090909090909061, 0.1181818181818181795, 0.1204545454545454530, 0.1227272727272727265, 0.1250000000000000000, 0.1272727272727272596, 0.1295454545454545470, 0.1318181818181818066, 0.1340909090909090939, 0.1363636363636363535, 0.1386363636363636409, 0.1409090909090909005, 0.1431818181818181879, 0.1454545454545454475, 0.1477272727272727348, 0.1499999999999999944, 0.1522727272727272818, 0.1545454545454545414, 0.1568181818181818288, 0.1590909090909090884, 0.1613636363636363757, 0.1636363636363636354, 0.1659090909090909227, 0.1681818181818181823, 0.1704545454545454419, 0.1727272727272727293, 0.1749999999999999889, 0.1772727272727272763, 0.1795454545454545359, 0.1818181818181818232, 0.1840909090909090828, 0.1863636363636363702, 0.1886363636363636298, 0.1909090909090909172, 0.1931818181818181768, 0.1954545454545454641, 0.1977272727272727237, 0.2000000000000000111, 0.2022727272727272707, 0.2045454545454545581, 0.2068181818181818177, 0.2090909090909090773, 0.2113636363636363646, 0.2136363636363636243, 0.2159090909090909116, 0.2181818181818181712, 0.2204545454545454586, 0.2227272727272727182, 0.2250000000000000056, 0.2272727272727272652, 0.2295454545454545525, 0.2318181818181818121, 0.2340909090909090995, 0.2363636363636363591, 0.2386363636363636465, 0.2409090909090909061, 0.2431818181818181934, 0.2454545454545454530, 0.2477272727272727404, 0.2500000000000000000, 0.2522727272727272596, 0.2545454545454545192, 0.2568181818181818343, 0.2590909090909090939, 0.2613636363636363535, 0.2636363636363636131, 0.2659090909090909283, 0.2681818181818181879, 0.2704545454545454475, 0.2727272727272727071, 0.2750000000000000222, 0.2772727272727272818, 0.2795454545454545414, 0.2818181818181818010, 0.2840909090909091161, 0.2863636363636363757, 0.2886363636363636354, 0.2909090909090908950, 0.2931818181818181546, 0.2954545454545454697, 0.2977272727272727293, 0.2999999999999999889, 0.3022727272727272485, 0.3045454545454545636, 0.3068181818181818232, 0.3090909090909090828, 0.3113636363636363424, 0.3136363636363636576, 0.3159090909090909172, 0.3181818181818181768, 0.3204545454545454364, 0.3227272727272727515, 0.3250000000000000111, 0.3272727272727272707, 0.3295454545454545303, 0.3318181818181818454, 0.3340909090909091050, 0.3363636363636363646, 0.3386363636363636243, 0.3409090909090908839, 0.3431818181818181990, 0.3454545454545454586, 0.3477272727272727182, 0.3499999999999999778, 0.3522727272727272929, 0.3545454545454545525, 0.3568181818181818121, 0.3590909090909090717, 0.3613636363636363869, 0.3636363636363636465, 0.3659090909090909061, 0.3681818181818181657, 0.3704545454545454808, 0.3727272727272727404, 0.3750000000000000000, 0.3772727272727272596, 0.3795454545454545192, 0.3818181818181818343, 0.3840909090909090939, 0.3863636363636363535, 0.3886363636363636131, 0.3909090909090909283, 0.3931818181818181879, 0.3954545454545454475, 0.3977272727272727071, 0.4000000000000000222, 0.4022727272727272818, 0.4045454545454545414, 0.4068181818181818010, 0.4090909090909091161, 0.4113636363636363757, 0.4136363636363636354, 0.4159090909090908950, 0.4181818181818181546, 0.4204545454545454697, 0.4227272727272727293, 0.4249999999999999889, 0.4272727272727272485, 0.4295454545454545636, 0.4318181818181818232, 0.4340909090909090828, 0.4363636363636363424, 0.4386363636363636576, 0.4409090909090909172, 0.4431818181818181768, 0.4454545454545454364, 0.4477272727272727515, 0.4500000000000000111, 0.4522727272727272707, 0.4545454545454545303, 0.4568181818181818454, 0.4590909090909091050, 0.4613636363636363646, 0.4636363636363636243, 0.4659090909090908839, 0.4681818181818181990, 0.4704545454545454586, 0.4727272727272727182, 0.4749999999999999778, 0.4772727272727272929, 0.4795454545454545525, 0.4818181818181818121, 0.4840909090909090717, 0.4863636363636363869, 0.4886363636363636465, 0.4909090909090909061, 0.4931818181818181657, 0.4954545454545454808, 0.4977272727272727404, 0.5000000000000000000, 0.5022727272727273151, 0.5045454545454545192, 0.5068181818181818343, 0.5090909090909090384, 0.5113636363636363535, 0.5136363636363636687, 0.5159090909090908728, 0.5181818181818181879, 0.5204545454545455030, 0.5227272727272727071, 0.5250000000000000222, 0.5272727272727272263, 0.5295454545454545414, 0.5318181818181818565, 0.5340909090909090606, 0.5363636363636363757, 0.5386363636363636909, 0.5409090909090908950, 0.5431818181818182101, 0.5454545454545454142, 0.5477272727272727293, 0.5500000000000000444, 0.5522727272727272485, 0.5545454545454545636, 0.5568181818181817677, 0.5590909090909090828, 0.5613636363636363980, 0.5636363636363636020, 0.5659090909090909172, 0.5681818181818182323, 0.5704545454545454364, 0.5727272727272727515, 0.5749999999999999556, 0.5772727272727272707, 0.5795454545454545858, 0.5818181818181817899, 0.5840909090909091050, 0.5863636363636363091, 0.5886363636363636243, 0.5909090909090909394, 0.5931818181818181435, 0.5954545454545454586, 0.5977272727272727737, 0.5999999999999999778, 0.6022727272727272929, 0.6045454545454544970, 0.6068181818181818121, 0.6090909090909091272, 0.6113636363636363313, 0.6136363636363636465, 0.6159090909090909616, 0.6181818181818181657, 0.6204545454545454808, 0.6227272727272726849, 0.6250000000000000000, 0.6272727272727273151, 0.6295454545454545192, 0.6318181818181818343, 0.6340909090909090384, 0.6363636363636363535, 0.6386363636363636687, 0.6409090909090908728, 0.6431818181818181879, 0.6454545454545455030, 0.6477272727272727071, 0.6500000000000000222, 0.6522727272727272263, 0.6545454545454545414, 0.6568181818181818565, 0.6590909090909090606, 0.6613636363636363757, 0.6636363636363636909, 0.6659090909090908950, 0.6681818181818182101, 0.6704545454545454142, 0.6727272727272727293, 0.6750000000000000444, 0.6772727272727272485, 0.6795454545454545636, 0.6818181818181817677, 0.6840909090909090828, 0.6863636363636363980, 0.6886363636363636020, 0.6909090909090909172, 0.6931818181818182323, 0.6954545454545454364, 0.6977272727272727515, 0.6999999999999999556, 0.7022727272727272707, 0.7045454545454545858, 0.7068181818181817899, 0.7090909090909091050, 0.7113636363636363091, 0.7136363636363636243, 0.7159090909090909394, 0.7181818181818181435, 0.7204545454545454586, 0.7227272727272727737, 0.7249999999999999778, 0.7272727272727272929, 0.7295454545454544970, 0.7318181818181818121, 0.7340909090909091272, 0.7363636363636363313, 0.7386363636363636465, 0.7409090909090909616, 0.7431818181818181657, 0.7454545454545454808, 0.7477272727272726849, 0.7500000000000000000, 0.7522727272727273151, 0.7545454545454545192, 0.7568181818181818343, 0.7590909090909090384, 0.7613636363636363535, 0.7636363636363636687, 0.7659090909090908728, 0.7681818181818181879, 0.7704545454545455030, 0.7727272727272727071, 0.7750000000000000222, 0.7772727272727272263, 0.7795454545454545414, 0.7818181818181818565, 0.7840909090909090606, 0.7863636363636363757, 0.7886363636363636909, 0.7909090909090908950, 0.7931818181818182101, 0.7954545454545454142, 0.7977272727272727293, 0.8000000000000000444, 0.8022727272727272485, 0.8045454545454545636, 0.8068181818181817677, 0.8090909090909090828, 0.8113636363636363980, 0.8136363636363636020, 0.8159090909090909172, 0.8181818181818182323, 0.8204545454545454364, 0.8227272727272727515, 0.8249999999999999556, 0.8272727272727272707, 0.8295454545454545858, 0.8318181818181817899, 0.8340909090909091050, 0.8363636363636363091, 0.8386363636363636243, 0.8409090909090909394, 0.8431818181818181435, 0.8454545454545454586, 0.8477272727272727737, 0.8499999999999999778, 0.8522727272727272929, 0.8545454545454544970, 0.8568181818181818121, 0.8590909090909091272, 0.8613636363636363313, 0.8636363636363636465, 0.8659090909090909616, 0.8681818181818181657, 0.8704545454545454808, 0.8727272727272726849, 0.8750000000000000000, 0.8772727272727273151, 0.8795454545454545192, 0.8818181818181818343, 0.8840909090909090384, 0.8863636363636363535, 0.8886363636363636687, 0.8909090909090908728, 0.8931818181818181879, 0.8954545454545455030, 0.8977272727272727071, 0.9000000000000000222, 0.9022727272727272263, 0.9045454545454545414, 0.9068181818181818565, 0.9090909090909090606, 0.9113636363636363757, 0.9136363636363636909, 0.9159090909090908950, 0.9181818181818182101, 0.9204545454545454142, 0.9227272727272727293, 0.9250000000000000444, 0.9272727272727272485, 0.9295454545454545636, 0.9318181818181817677, 0.9340909090909090828, 0.9363636363636363980, 0.9386363636363636020, 0.9409090909090909172, 0.9431818181818182323, 0.9454545454545454364, 0.9477272727272727515, 0.9499999999999999556, 0.9522727272727272707, 0.9545454545454545858, 0.9568181818181817899, 0.9590909090909091050, 0.9613636363636363091, 0.9636363636363636243, 0.9659090909090909394, 0.9681818181818181435, 0.9704545454545454586, 0.9727272727272727737, 0.9749999999999999778, 0.9772727272727272929, 0.9781254700864303597 ),
 .UNSPECIFIED. ) 
 GEOMETRIC_REPRESENTATION_ITEM ( )  RATIONAL_B_SPLINE_SURFACE ( (
 ( 1.000000000000000000, 0.9898214418809326842, 1.000000000000000000, 0.9898214418809326842, 1.000000000000000000, 0.9898214418809326842, 1.000000000000000000, 0.9898214418809326842, 1.000000000000000000, 0.9898214418809326842, 1.000000000000000000, 0.9898214418809326842, 1.000000000000000000, 0.9898214418809326842, 1.000000000000000000, 0.9898214418809326842, 1.000000000000000000, 0.9898214418809326842, 1.000000000000000000, 0.9898214418809326842, 1.000000000000000000, 0.9898214418809326842, 1.000000000000000000, 0.9898214418809326842, 1.000000000000000000, 0.9898214418809326842, 1.000000000000000000, 0.9898214418809326842, 1.000000000000000000, 0.9898214418809326842, 1.000000000000000000, 0.9898214418809326842, 1.000000000000000000, 0.9898214418809326842, 1.000000000000000000, 0.9898214418809326842, 1.000000000000000000, 0.9898214418809326842, 1.000000000000000000, 0.9898214418809326842, 1.000000000000000000, 0.9898214418809326842, 1.000000000000000000, 0.9898214418809326842, 1.000000000000000000, 0.9898214418809326842, 1.000000000000000000, 0.9898214418809326842, 1.000000000000000000, 0.9898214418809326842, 1.000000000000000000, 0.9898214418809326842, 1.000000000000000000, 0.9898214418809326842, 1.000000000000000000, 0.9898214418809326842, 1.000000000000000000, 0.9898214418809326842, 1.000000000000000000, 0.9898214418809326842, 1.000000000000000000, 0.9898214418809326842, 1.000000000000000000, 0.9898214418809326842, 1.000000000000000000, 0.9898214418809326842, 1.000000000000000000, 0.9898214418809326842, 1.000000000000000000, 0.9898214418809326842, 1.000000000000000000, 0.9898214418809326842, 1.000000000000000000, 0.9898214418809326842, 1.000000000000000000, 0.9898214418809326842, 1.000000000000000000, 0.9898214418809326842, 1.000000000000000000, 0.9898214418809326842, 1.000000000000000000, 0.9898214418809326842, 1.000000000000000000, 0.9898214418809326842, 1.000000000000000000, 0.9898214418809326842, 1.000000000000000000, 0.9898214418809326842, 1.000000000000000000, 0.9898214418809326842, 1.000000000000000000, 0.9898214418809326842, 1.000000000000000000, 0.9898214418809326842, 1.000000000000000000, 0.9898214418809326842, 1.000000000000000000, 0.9898214418809326842, 1.000000000000000000, 0.9898214418809326842, 1.000000000000000000, 0.9898214418809326842, 1.000000000000000000, 0.9898214418809326842, 1.000000000000000000, 0.9898214418809326842, 1.000000000000000000, 0.9898214418809326842, 1.000000000000000000, 0.9898214418809326842, 1.000000000000000000, 0.9898214418809326842, 1.000000000000000000, 0.9898214418809326842, 1.000000000000000000, 0.9898214418809326842, 1.000000000000000000, 0.9898214418809326842, 1.000000000000000000, 0.9898214418809326842, 1.000000000000000000, 0.9898214418809326842, 1.000000000000000000, 0.9898214418809326842, 1.000000000000000000, 0.9898214418809326842, 1.000000000000000000, 0.9898214418809326842, 1.000000000000000000, 0.9898214418809326842, 1.000000000000000000, 0.9898214418809326842, 1.000000000000000000, 0.9898214418809326842, 1.000000000000000000, 0.9898214418809326842, 1.000000000000000000, 0.9898214418809326842, 1.000000000000000000, 0.9898214418809326842, 1.000000000000000000, 0.9898214418809326842, 1.000000000000000000, 0.9898214418809326842, 1.000000000000000000, 0.9898214418809326842, 1.000000000000000000, 0.9898214418809326842, 1.000000000000000000, 0.9898214418809326842, 1.000000000000000000, 0.9898214418809326842, 1.000000000000000000, 0.9898214418809326842, 1.000000000000000000, 0.9898214418809326842, 1.000000000000000000, 0.9898214418809326842, 1.000000000000000000, 0.9898214418809326842, 1.000000000000000000, 0.9898214418809326842, 1.000000000000000000, 0.9898214418809326842, 1.000000000000000000, 0.9898214418809326842, 1.000000000000000000, 0.9898214418809326842, 1.000000000000000000, 0.9898214418809326842, 1.000000000000000000, 0.9898214418809326842, 1.000000000000000000, 0.9898214418809326842, 1.000000000000000000, 0.9898214418809326842, 1.000000000000000000, 0.9898214418809326842, 1.000000000000000000, 0.9898214418809326842, 1.000000000000000000, 0.9898214418809326842, 1.000000000000000000, 0.9898214418809326842, 1.000000000000000000, 0.9898214418809326842, 1.000000000000000000, 0.9898214418809326842, 1.000000000000000000, 0.9898214418809326842, 1.000000000000000000, 0.9898214418809326842, 1.000000000000000000, 0.9898214418809326842, 1.000000000000000000, 0.9898214418809326842, 1.000000000000000000, 0.9898214418809326842, 1.000000000000000000, 0.9898214418809326842, 1.000000000000000000, 0.9898214418809326842, 1.000000000000000000, 0.9898214418809326842, 1.000000000000000000, 0.9898214418809326842, 1.000000000000000000, 0.9898214418809326842, 1.000000000000000000, 0.9898214418809326842, 1.000000000000000000, 0.9898214418809326842, 1.000000000000000000, 0.9898214418809326842, 1.000000000000000000, 0.9898214418809326842, 1.000000000000000000, 0.9898214418809326842, 1.000000000000000000, 0.9898214418809326842, 1.000000000000000000, 0.9898214418809326842, 1.000000000000000000, 0.9898214418809326842, 1.000000000000000000, 0.9898214418809326842, 1.000000000000000000, 0.9898214418809326842, 1.000000000000000000, 0.9898214418809326842, 1.000000000000000000, 0.9898214418809326842, 1.000000000000000000, 0.9898214418809326842, 1.000000000000000000, 0.9898214418809326842, 1.000000000000000000, 0.9898214418809326842, 1.000000000000000000, 0.9898214418809326842, 1.000000000000000000, 0.9898214418809326842, 1.000000000000000000, 0.9898214418809326842, 1.000000000000000000, 0.9898214418809326842, 1.000000000000000000, 0.9898214418809326842, 1.000000000000000000, 0.9898214418809326842, 1.000000000000000000, 0.9898214418809326842, 1.000000000000000000, 0.9898214418809326842, 1.000000000000000000, 0.9898214418809326842, 1.000000000000000000, 0.9898214418809326842, 1.000000000000000000, 0.9898214418809326842, 1.000000000000000000, 0.9898214418809326842, 1.000000000000000000, 0.9898214418809326842, 1.000000000000000000, 0.9898214418809326842, 1.000000000000000000, 0.9898214418809326842, 1.000000000000000000, 0.9898214418809326842, 1.000000000000000000, 0.9898214418809326842, 1.000000000000000000, 0.9898214418809326842, 1.000000000000000000, 0.9898214418809326842, 1.000000000000000000, 0.9898214418809326842, 1.000000000000000000, 0.9898214418809326842, 1.000000000000000000, 0.9898214418809326842, 1.000000000000000000, 0.9898214418809326842, 1.000000000000000000, 0.9898214418809326842, 1.000000000000000000, 0.9898214418809326842, 1.000000000000000000, 0.9898214418809326842, 1.000000000000000000, 0.9898214418809326842, 1.000000000000000000, 0.9898214418809326842, 1.000000000000000000, 0.9898214418809326842, 1.000000000000000000, 0.9898214418809326842, 1.000000000000000000, 0.9898214418809326842, 1.000000000000000000, 0.9898214418809326842, 1.000000000000000000, 0.9898214418809326842, 1.000000000000000000, 0.9898214418809326842, 1.000000000000000000, 0.9898214418809326842, 1.000000000000000000, 0.9898214418809326842, 1.000000000000000000, 0.9898214418809326842, 1.000000000000000000, 0.9898214418809326842, 1.000000000000000000, 0.9898214418809326842, 1.000000000000000000, 0.9898214418809326842, 1.000000000000000000, 0.9898214418809326842, 1.000000000000000000, 0.9898214418809326842, 1.000000000000000000, 0.9898214418809326842, 1.000000000000000000, 0.9898214418809326842, 1.000000000000000000, 0.9898214418809326842, 1.000000000000000000, 0.9898214418809326842, 1.000000000000000000, 0.9898214418809326842, 1.000000000000000000, 0.9898214418809326842, 1.000000000000000000, 0.9898214418809326842, 1.000000000000000000, 0.9898214418809326842, 1.000000000000000000, 0.9898214418809326842, 1.000000000000000000, 0.9898214418809326842, 1.000000000000000000, 0.9898214418809326842, 1.000000000000000000, 0.9898214418809326842, 1.000000000000000000, 0.9898214418809326842, 1.000000000000000000, 0.9898214418809326842, 1.000000000000000000, 0.9898214418809326842, 1.000000000000000000, 0.9898214418809326842, 1.000000000000000000, 0.9898214418809326842, 1.000000000000000000, 0.9898214418809326842, 1.000000000000000000, 0.9898214418809326842, 1.000000000000000000, 0.9898214418809326842, 1.000000000000000000, 0.9898214418809326842, 1.000000000000000000, 0.9898214418809326842, 1.000000000000000000, 0.9898214418809326842, 1.000000000000000000, 0.9898214418809326842, 1.000000000000000000, 0.9898214418809326842, 1.000000000000000000, 0.9898214418809326842, 1.000000000000000000, 0.9898214418809326842, 1.000000000000000000, 0.9898214418809326842, 1.000000000000000000, 0.9898214418809326842, 1.000000000000000000, 0.9898214418809326842, 1.000000000000000000, 0.9898214418809326842, 1.000000000000000000, 0.9898214418809326842, 1.000000000000000000, 0.9898214418809326842, 1.000000000000000000, 0.9898214418809326842, 1.000000000000000000, 0.9898214418809326842, 1.000000000000000000, 0.9898214418809326842, 1.000000000000000000, 0.9898214418809326842, 1.000000000000000000, 0.9898214418809326842, 1.000000000000000000, 0.9898214418809326842, 1.000000000000000000, 0.9898214418809326842, 1.000000000000000000, 0.9898214418809326842, 1.000000000000000000, 0.9898214418809326842, 1.000000000000000000, 0.9898214418809326842, 1.000000000000000000, 0.9898214418809326842, 1.000000000000000000, 0.9898214418809326842, 1.000000000000000000, 0.9898214418809326842, 1.000000000000000000, 0.9898214418809326842, 1.000000000000000000, 0.9898214418809326842, 1.000000000000000000, 0.9898214418809326842, 1.000000000000000000, 0.9898214418809326842, 1.000000000000000000, 0.9898214418809326842, 1.000000000000000000, 0.9898214418809326842, 1.000000000000000000, 0.9898214418809326842, 1.000000000000000000, 0.9898214418809326842, 1.000000000000000000, 0.9898214418809326842, 1.000000000000000000, 0.9898214418809326842, 1.000000000000000000, 0.9898214418809326842, 1.000000000000000000, 0.9898214418809326842, 1.000000000000000000, 0.9898214418809326842, 1.000000000000000000, 0.9898214418809326842, 1.000000000000000000, 0.9898214418809326842, 1.000000000000000000, 0.9898214418809326842, 1.000000000000000000, 0.9898214418809326842, 1.000000000000000000, 0.9898214418809326842, 1.000000000000000000, 0.9898214418809326842, 1.000000000000000000, 0.9898214418809326842, 1.000000000000000000, 0.9898214418809326842, 1.000000000000000000, 0.9898214418809326842, 1.000000000000000000, 0.9898214418809326842, 1.000000000000000000, 0.9898214418809326842, 1.000000000000000000, 0.9898214418809326842, 1.000000000000000000, 0.9898214418809326842, 1.000000000000000000, 0.9898214418809326842, 1.000000000000000000, 0.9898214418809326842, 1.000000000000000000, 0.9898214418809326842, 1.000000000000000000, 0.9898214418809326842, 1.000000000000000000, 0.9898214418809326842, 1.000000000000000000, 0.9898214418809326842, 1.000000000000000000, 0.9898214418809326842, 1.000000000000000000, 0.9898214418809326842, 1.000000000000000000, 0.9898214418809326842, 1.000000000000000000, 0.9898214418809326842, 1.000000000000000000, 0.9898214418809326842, 1.000000000000000000, 0.9898214418809326842, 1.000000000000000000, 0.9898214418809326842, 1.000000000000000000, 0.9898214418809326842, 1.000000000000000000, 0.9898214418809326842, 1.000000000000000000, 0.9898214418809326842, 1.000000000000000000, 0.9898214418809326842, 1.000000000000000000, 0.9898214418809326842, 1.000000000000000000, 0.9898214418809326842, 1.000000000000000000, 0.9898214418809326842, 1.000000000000000000, 0.9898214418809326842, 1.000000000000000000, 0.9898214418809326842, 1.000000000000000000, 0.9898214418809326842, 1.000000000000000000, 0.9898214418809326842, 1.000000000000000000, 0.9898214418809326842, 1.000000000000000000, 0.9898214418809326842, 1.000000000000000000, 0.9898214418809326842, 1.000000000000000000, 0.9898214418809326842, 1.000000000000000000, 0.9898214418809326842, 1.000000000000000000, 0.9898214418809326842, 1.000000000000000000, 0.9898214418809326842, 1.000000000000000000, 0.9898214418809326842, 1.000000000000000000, 0.9898214418809326842, 1.000000000000000000, 0.9898214418809326842, 1.000000000000000000, 0.9898214418809326842, 1.000000000000000000, 0.9898214418809326842, 1.000000000000000000, 0.9898214418809326842, 1.000000000000000000, 0.9898214418809326842, 1.000000000000000000, 0.9898214418809326842, 1.000000000000000000, 0.9898214418809326842, 1.000000000000000000, 0.9898214418809326842, 1.000000000000000000, 0.9898214418809326842, 1.000000000000000000, 0.9898214418809326842, 1.000000000000000000, 0.9898214418809326842, 1.000000000000000000, 0.9898214418809326842, 1.000000000000000000, 0.9898214418809326842, 1.000000000000000000, 0.9898214418809326842, 1.000000000000000000, 0.9898214418809326842, 1.000000000000000000, 0.9898214418809326842, 1.000000000000000000, 0.9898214418809326842, 1.000000000000000000, 0.9898214418809326842, 1.000000000000000000, 0.9898214418809326842, 1.000000000000000000, 0.9898214418809326842, 1.000000000000000000, 0.9898214418809326842, 1.000000000000000000, 0.9898214418809326842, 1.000000000000000000, 0.9898214418809326842, 1.000000000000000000, 0.9898214418809326842, 1.000000000000000000, 0.9898214418809326842, 1.000000000000000000, 0.9898214418809326842, 1.000000000000000000, 0.9898214418809326842, 1.000000000000000000, 0.9898214418809326842, 1.000000000000000000, 0.9898214418809326842, 1.000000000000000000, 0.9898214418809326842, 1.000000000000000000, 0.9898214418809326842, 1.000000000000000000, 0.9898214418809326842, 1.000000000000000000, 0.9898214418809326842, 1.000000000000000000, 0.9898214418809326842, 1.000000000000000000, 0.9898214418809326842, 1.000000000000000000, 0.9898214418809326842, 1.000000000000000000, 0.9898214418809326842, 1.000000000000000000, 0.9898214418809326842, 1.000000000000000000, 0.9898214418809326842, 1.000000000000000000, 0.9898214418809326842, 1.000000000000000000, 0.9898214418809326842, 1.000000000000000000, 0.9898214418809326842, 1.000000000000000000, 0.9898214418809326842, 1.000000000000000000, 0.9898214418809326842, 1.000000000000000000, 0.9898214418809326842, 1.000000000000000000, 0.9898214418809326842, 1.000000000000000000, 0.9898214418809326842, 1.000000000000000000, 0.9898214418809326842, 1.000000000000000000, 0.9898214418809326842, 1.000000000000000000, 0.9898214418809326842, 1.000000000000000000, 0.9898214418809326842, 1.000000000000000000, 0.9898214418809326842, 1.000000000000000000, 0.9898214418809326842, 1.000000000000000000, 0.9898214418809326842, 1.000000000000000000, 0.9898214418809326842, 1.000000000000000000, 0.9898214418809326842, 1.000000000000000000, 0.9898214418809326842, 1.000000000000000000, 0.9898214418809326842, 1.000000000000000000, 0.9898214418809326842, 1.000000000000000000, 0.9898214418809326842, 1.000000000000000000, 0.9898214418809326842, 1.000000000000000000, 0.9898214418809326842, 1.000000000000000000, 0.9898214418809326842, 1.000000000000000000, 0.9898214418809326842, 1.000000000000000000, 0.9898214418809326842, 1.000000000000000000, 0.9898214418809326842, 1.000000000000000000, 0.9898214418809326842, 1.000000000000000000, 0.9898214418809326842, 1.000000000000000000, 0.9898214418809326842, 1.000000000000000000, 0.9898214418809326842, 1.000000000000000000, 0.9898214418809326842, 1.000000000000000000, 0.9898214418809326842, 1.000000000000000000, 0.9898214418809326842, 1.000000000000000000, 0.9898214418809326842, 1.000000000000000000, 0.9898214418809326842, 1.000000000000000000, 0.9898214418809326842, 1.000000000000000000, 0.9898214418809326842, 1.000000000000000000, 0.9898214418809326842, 1.000000000000000000, 0.9898214418809326842, 1.000000000000000000, 0.9898214418809326842, 1.000000000000000000, 0.9898214418809326842, 1.000000000000000000, 0.9898214418809326842, 1.000000000000000000, 0.9898214418809326842, 1.000000000000000000, 0.9898214418809326842, 1.000000000000000000, 0.9898214418809326842, 1.000000000000000000, 0.9898214418809326842, 1.000000000000000000, 0.9898214418809326842, 1.000000000000000000, 0.9898214418809326842, 1.000000000000000000, 0.9898214418809326842, 1.000000000000000000, 0.9898214418809326842, 1.000000000000000000, 0.9898214418809326842, 1.000000000000000000, 0.9898214418809326842, 1.000000000000000000, 0.9898214418809326842, 1.000000000000000000, 0.9898214418809326842, 1.000000000000000000, 0.9898214418809326842, 1.000000000000000000, 0.9898214418809326842, 1.000000000000000000, 0.9898214418809326842, 1.000000000000000000, 0.9898214418809326842, 1.000000000000000000, 0.9898214418809326842, 1.000000000000000000, 0.9898214418809326842, 1.000000000000000000, 0.9898214418809326842, 1.000000000000000000, 0.9898214418809326842, 1.000000000000000000, 0.9898214418809326842, 1.000000000000000000, 0.9898214418809326842, 1.000000000000000000, 0.9898214418809326842, 1.000000000000000000, 0.9898214418809326842, 1.000000000000000000, 0.9898214418809326842, 1.000000000000000000, 0.9898214418809326842, 1.000000000000000000, 0.9898214418809326842, 1.000000000000000000, 0.9898214418809326842, 1.000000000000000000, 0.9898214418809326842, 1.000000000000000000, 0.9898214418809326842, 1.000000000000000000, 0.9898214418809326842, 1.000000000000000000, 0.9898214418809326842, 1.000000000000000000, 0.9898214418809326842, 1.000000000000000000, 0.9898214418809326842, 1.000000000000000000, 0.9898214418809326842, 1.000000000000000000, 0.9898214418809326842, 1.000000000000000000, 0.9898214418809326842, 1.000000000000000000, 0.9898214418809326842, 1.000000000000000000, 0.9898214418809326842, 1.000000000000000000, 0.9898214418809326842, 1.000000000000000000, 0.9898214418809326842, 1.000000000000000000, 0.9898214418809326842, 1.000000000000000000, 0.9898214418809326842, 1.000000000000000000, 0.9898214418809326842, 1.000000000000000000, 0.9898214418809326842, 1.000000000000000000, 0.9898214418809326842, 1.000000000000000000, 0.9898214418809326842, 1.000000000000000000, 0.9898214418809326842, 1.000000000000000000, 0.9898214418809326842, 1.000000000000000000, 0.9898214418809326842, 1.000000000000000000, 0.9898214418809326842, 1.000000000000000000, 0.9898214418809326842, 1.000000000000000000, 0.9898214418809326842, 1.000000000000000000, 0.9898214418809326842, 1.000000000000000000, 0.9898214418809326842, 1.000000000000000000, 0.9898214418809326842, 1.000000000000000000, 0.9898214418809326842, 1.000000000000000000, 0.9898214418809326842, 1.000000000000000000, 0.9898214418809326842, 1.000000000000000000, 0.9898214418809326842, 1.000000000000000000, 0.9898214418809326842, 1.000000000000000000, 0.9898214418809326842, 1.000000000000000000, 0.9898214418809326842, 1.000000000000000000, 0.9898214418809326842, 1.000000000000000000, 0.9898214418809326842, 1.000000000000000000, 0.9898214418809326842, 1.000000000000000000, 0.9898214418809326842, 1.000000000000000000, 0.9898214418809326842, 1.000000000000000000, 0.9898214418809326842, 1.000000000000000000, 0.9898214418809326842, 1.000000000000000000, 0.9898214418809326842, 1.000000000000000000, 0.9898214418809326842, 1.000000000000000000, 0.9898214418809326842, 1.000000000000000000, 0.9898214418809326842, 1.000000000000000000, 0.9898214418809326842, 1.000000000000000000, 0.9898214418809326842, 1.000000000000000000, 0.9898214418809326842, 1.000000000000000000, 0.9898214418809326842, 1.000000000000000000, 0.9898214418809326842, 1.000000000000000000, 0.9898214418809326842, 1.000000000000000000, 0.9898214418809326842, 1.000000000000000000, 0.9898214418809326842, 1.000000000000000000, 0.9961809353924466759, 0.9952277490961531914),
 ( 0.3333333333333333703, 0.3299404806269776169, 0.3333333333333333703, 0.3299404806269776169, 0.3333333333333333703, 0.3299404806269776169, 0.3333333333333333703, 0.3299404806269776169, 0.3333333333333333703, 0.3299404806269776169, 0.3333333333333333703, 0.3299404806269776169, 0.3333333333333333703, 0.3299404806269776169, 0.3333333333333333703, 0.3299404806269776169, 0.3333333333333333703, 0.3299404806269776169, 0.3333333333333333703, 0.3299404806269776169, 0.3333333333333333703, 0.3299404806269776169, 0.3333333333333333703, 0.3299404806269776169, 0.3333333333333333703, 0.3299404806269776169, 0.3333333333333333703, 0.3299404806269776169, 0.3333333333333333703, 0.3299404806269776169, 0.3333333333333333703, 0.3299404806269776169, 0.3333333333333333703, 0.3299404806269776169, 0.3333333333333333703, 0.3299404806269776169, 0.3333333333333333703, 0.3299404806269776169, 0.3333333333333333703, 0.3299404806269776169, 0.3333333333333333703, 0.3299404806269776169, 0.3333333333333333703, 0.3299404806269776169, 0.3333333333333333703, 0.3299404806269776169, 0.3333333333333333703, 0.3299404806269776169, 0.3333333333333333703, 0.3299404806269776169, 0.3333333333333333703, 0.3299404806269776169, 0.3333333333333333703, 0.3299404806269776169, 0.3333333333333333703, 0.3299404806269776169, 0.3333333333333333703, 0.3299404806269776169, 0.3333333333333333703, 0.3299404806269776169, 0.3333333333333333703, 0.3299404806269776169, 0.3333333333333333703, 0.3299404806269776169, 0.3333333333333333703, 0.3299404806269776169, 0.3333333333333333703, 0.3299404806269776169, 0.3333333333333333703, 0.3299404806269776169, 0.3333333333333333703, 0.3299404806269776169, 0.3333333333333333703, 0.3299404806269776169, 0.3333333333333333703, 0.3299404806269776169, 0.3333333333333333703, 0.3299404806269776169, 0.3333333333333333703, 0.3299404806269776169, 0.3333333333333333703, 0.3299404806269776169, 0.3333333333333333703, 0.3299404806269776169, 0.3333333333333333703, 0.3299404806269776169, 0.3333333333333333703, 0.3299404806269776169, 0.3333333333333333703, 0.3299404806269776169, 0.3333333333333333703, 0.3299404806269776169, 0.3333333333333333703, 0.3299404806269776169, 0.3333333333333333703, 0.3299404806269776169, 0.3333333333333333703, 0.3299404806269776169, 0.3333333333333333703, 0.3299404806269776169, 0.3333333333333333703, 0.3299404806269776169, 0.3333333333333333703, 0.3299404806269776169, 0.3333333333333333703, 0.3299404806269776169, 0.3333333333333333703, 0.3299404806269776169, 0.3333333333333333703, 0.3299404806269776169, 0.3333333333333333703, 0.3299404806269776169, 0.3333333333333333703, 0.3299404806269776169, 0.3333333333333333703, 0.3299404806269776169, 0.3333333333333333703, 0.3299404806269776169, 0.3333333333333333703, 0.3299404806269776169, 0.3333333333333333703, 0.3299404806269776169, 0.3333333333333333703, 0.3299404806269776169, 0.3333333333333333703, 0.3299404806269776169, 0.3333333333333333703, 0.3299404806269776169, 0.3333333333333333703, 0.3299404806269776169, 0.3333333333333333703, 0.3299404806269776169, 0.3333333333333333703, 0.3299404806269776169, 0.3333333333333333703, 0.3299404806269776169, 0.3333333333333333703, 0.3299404806269776169, 0.3333333333333333703, 0.3299404806269776169, 0.3333333333333333703, 0.3299404806269776169, 0.3333333333333333703, 0.3299404806269776169, 0.3333333333333333703, 0.3299404806269776169, 0.3333333333333333703, 0.3299404806269776169, 0.3333333333333333703, 0.3299404806269776169, 0.3333333333333333703, 0.3299404806269776169, 0.3333333333333333703, 0.3299404806269776169, 0.3333333333333333703, 0.3299404806269776169, 0.3333333333333333703, 0.3299404806269776169, 0.3333333333333333703, 0.3299404806269776169, 0.3333333333333333703, 0.3299404806269776169, 0.3333333333333333703, 0.3299404806269776169, 0.3333333333333333703, 0.3299404806269776169, 0.3333333333333333703, 0.3299404806269776169, 0.3333333333333333703, 0.3299404806269776169, 0.3333333333333333703, 0.3299404806269776169, 0.3333333333333333703, 0.3299404806269776169, 0.3333333333333333703, 0.3299404806269776169, 0.3333333333333333703, 0.3299404806269776169, 0.3333333333333333703, 0.3299404806269776169, 0.3333333333333333703, 0.3299404806269776169, 0.3333333333333333703, 0.3299404806269776169, 0.3333333333333333703, 0.3299404806269776169, 0.3333333333333333703, 0.3299404806269776169, 0.3333333333333333703, 0.3299404806269776169, 0.3333333333333333703, 0.3299404806269776169, 0.3333333333333333703, 0.3299404806269776169, 0.3333333333333333703, 0.3299404806269776169, 0.3333333333333333703, 0.3299404806269776169, 0.3333333333333333703, 0.3299404806269776169, 0.3333333333333333703, 0.3299404806269776169, 0.3333333333333333703, 0.3299404806269776169, 0.3333333333333333703, 0.3299404806269776169, 0.3333333333333333703, 0.3299404806269776169, 0.3333333333333333703, 0.3299404806269776169, 0.3333333333333333703, 0.3299404806269776169, 0.3333333333333333703, 0.3299404806269776169, 0.3333333333333333703, 0.3299404806269776169, 0.3333333333333333703, 0.3299404806269776169, 0.3333333333333333703, 0.3299404806269776169, 0.3333333333333333703, 0.3299404806269776169, 0.3333333333333333703, 0.3299404806269776169, 0.3333333333333333703, 0.3299404806269776169, 0.3333333333333333703, 0.3299404806269776169, 0.3333333333333333703, 0.3299404806269776169, 0.3333333333333333703, 0.3299404806269776169, 0.3333333333333333703, 0.3299404806269776169, 0.3333333333333333703, 0.3299404806269776169, 0.3333333333333333703, 0.3299404806269776169, 0.3333333333333333703, 0.3299404806269776169, 0.3333333333333333703, 0.3299404806269776169, 0.3333333333333333703, 0.3299404806269776169, 0.3333333333333333703, 0.3299404806269776169, 0.3333333333333333703, 0.3299404806269776169, 0.3333333333333333703, 0.3299404806269776169, 0.3333333333333333703, 0.3299404806269776169, 0.3333333333333333703, 0.3299404806269776169, 0.3333333333333333703, 0.3299404806269776169, 0.3333333333333333703, 0.3299404806269776169, 0.3333333333333333703, 0.3299404806269776169, 0.3333333333333333703, 0.3299404806269776169, 0.3333333333333333703, 0.3299404806269776169, 0.3333333333333333703, 0.3299404806269776169, 0.3333333333333333703, 0.3299404806269776169, 0.3333333333333333703, 0.3299404806269776169, 0.3333333333333333703, 0.3299404806269776169, 0.3333333333333333703, 0.3299404806269776169, 0.3333333333333333703, 0.3299404806269776169, 0.3333333333333333703, 0.3299404806269776169, 0.3333333333333333703, 0.3299404806269776169, 0.3333333333333333703, 0.3299404806269776169, 0.3333333333333333703, 0.3299404806269776169, 0.3333333333333333703, 0.3299404806269776169, 0.3333333333333333703, 0.3299404806269776169, 0.3333333333333333703, 0.3299404806269776169, 0.3333333333333333703, 0.3299404806269776169, 0.3333333333333333703, 0.3299404806269776169, 0.3333333333333333703, 0.3299404806269776169, 0.3333333333333333703, 0.3299404806269776169, 0.3333333333333333703, 0.3299404806269776169, 0.3333333333333333703, 0.3299404806269776169, 0.3333333333333333703, 0.3299404806269776169, 0.3333333333333333703, 0.3299404806269776169, 0.3333333333333333703, 0.3299404806269776169, 0.3333333333333333703, 0.3299404806269776169, 0.3333333333333333703, 0.3299404806269776169, 0.3333333333333333703, 0.3299404806269776169, 0.3333333333333333703, 0.3299404806269776169, 0.3333333333333333703, 0.3299404806269776169, 0.3333333333333333703, 0.3299404806269776169, 0.3333333333333333703, 0.3299404806269776169, 0.3333333333333333703, 0.3299404806269776169, 0.3333333333333333703, 0.3299404806269776169, 0.3333333333333333703, 0.3299404806269776169, 0.3333333333333333703, 0.3299404806269776169, 0.3333333333333333703, 0.3299404806269776169, 0.3333333333333333703, 0.3299404806269776169, 0.3333333333333333703, 0.3299404806269776169, 0.3333333333333333703, 0.3299404806269776169, 0.3333333333333333703, 0.3299404806269776169, 0.3333333333333333703, 0.3299404806269776169, 0.3333333333333333703, 0.3299404806269776169, 0.3333333333333333703, 0.3299404806269776169, 0.3333333333333333703, 0.3299404806269776169, 0.3333333333333333703, 0.3299404806269776169, 0.3333333333333333703, 0.3299404806269776169, 0.3333333333333333703, 0.3299404806269776169, 0.3333333333333333703, 0.3299404806269776169, 0.3333333333333333703, 0.3299404806269776169, 0.3333333333333333703, 0.3299404806269776169, 0.3333333333333333703, 0.3299404806269776169, 0.3333333333333333703, 0.3299404806269776169, 0.3333333333333333703, 0.3299404806269776169, 0.3333333333333333703, 0.3299404806269776169, 0.3333333333333333703, 0.3299404806269776169, 0.3333333333333333703, 0.3299404806269776169, 0.3333333333333333703, 0.3299404806269776169, 0.3333333333333333703, 0.3299404806269776169, 0.3333333333333333703, 0.3299404806269776169, 0.3333333333333333703, 0.3299404806269776169, 0.3333333333333333703, 0.3299404806269776169, 0.3333333333333333703, 0.3299404806269776169, 0.3333333333333333703, 0.3299404806269776169, 0.3333333333333333703, 0.3299404806269776169, 0.3333333333333333703, 0.3299404806269776169, 0.3333333333333333703, 0.3299404806269776169, 0.3333333333333333703, 0.3299404806269776169, 0.3333333333333333703, 0.3299404806269776169, 0.3333333333333333703, 0.3299404806269776169, 0.3333333333333333703, 0.3299404806269776169, 0.3333333333333333703, 0.3299404806269776169, 0.3333333333333333703, 0.3299404806269776169, 0.3333333333333333703, 0.3299404806269776169, 0.3333333333333333703, 0.3299404806269776169, 0.3333333333333333703, 0.3299404806269776169, 0.3333333333333333703, 0.3299404806269776169, 0.3333333333333333703, 0.3299404806269776169, 0.3333333333333333703, 0.3299404806269776169, 0.3333333333333333703, 0.3299404806269776169, 0.3333333333333333703, 0.3299404806269776169, 0.3333333333333333703, 0.3299404806269776169, 0.3333333333333333703, 0.3299404806269776169, 0.3333333333333333703, 0.3299404806269776169, 0.3333333333333333703, 0.3299404806269776169, 0.3333333333333333703, 0.3299404806269776169, 0.3333333333333333703, 0.3299404806269776169, 0.3333333333333333703, 0.3299404806269776169, 0.3333333333333333703, 0.3299404806269776169, 0.3333333333333333703, 0.3299404806269776169, 0.3333333333333333703, 0.3299404806269776169, 0.3333333333333333703, 0.3299404806269776169, 0.3333333333333333703, 0.3299404806269776169, 0.3333333333333333703, 0.3299404806269776169, 0.3333333333333333703, 0.3299404806269776169, 0.3333333333333333703, 0.3299404806269776169, 0.3333333333333333703, 0.3299404806269776169, 0.3333333333333333703, 0.3299404806269776169, 0.3333333333333333703, 0.3299404806269776169, 0.3333333333333333703, 0.3299404806269776169, 0.3333333333333333703, 0.3299404806269776169, 0.3333333333333333703, 0.3299404806269776169, 0.3333333333333333703, 0.3299404806269776169, 0.3333333333333333703, 0.3299404806269776169, 0.3333333333333333703, 0.3299404806269776169, 0.3333333333333333703, 0.3299404806269776169, 0.3333333333333333703, 0.3299404806269776169, 0.3333333333333333703, 0.3299404806269776169, 0.3333333333333333703, 0.3299404806269776169, 0.3333333333333333703, 0.3299404806269776169, 0.3333333333333333703, 0.3299404806269776169, 0.3333333333333333703, 0.3299404806269776169, 0.3333333333333333703, 0.3299404806269776169, 0.3333333333333333703, 0.3299404806269776169, 0.3333333333333333703, 0.3299404806269776169, 0.3333333333333333703, 0.3299404806269776169, 0.3333333333333333703, 0.3299404806269776169, 0.3333333333333333703, 0.3299404806269776169, 0.3333333333333333703, 0.3299404806269776169, 0.3333333333333333703, 0.3299404806269776169, 0.3333333333333333703, 0.3299404806269776169, 0.3333333333333333703, 0.3299404806269776169, 0.3333333333333333703, 0.3299404806269776169, 0.3333333333333333703, 0.3299404806269776169, 0.3333333333333333703, 0.3299404806269776169, 0.3333333333333333703, 0.3299404806269776169, 0.3333333333333333703, 0.3299404806269776169, 0.3333333333333333703, 0.3299404806269776169, 0.3333333333333333703, 0.3299404806269776169, 0.3333333333333333703, 0.3299404806269776169, 0.3333333333333333703, 0.3299404806269776169, 0.3333333333333333703, 0.3299404806269776169, 0.3333333333333333703, 0.3299404806269776169, 0.3333333333333333703, 0.3299404806269776169, 0.3333333333333333703, 0.3299404806269776169, 0.3333333333333333703, 0.3299404806269776169, 0.3333333333333333703, 0.3299404806269776169, 0.3333333333333333703, 0.3299404806269776169, 0.3333333333333333703, 0.3299404806269776169, 0.3333333333333333703, 0.3299404806269776169, 0.3333333333333333703, 0.3299404806269776169, 0.3333333333333333703, 0.3299404806269776169, 0.3333333333333333703, 0.3299404806269776169, 0.3333333333333333703, 0.3299404806269776169, 0.3333333333333333703, 0.3299404806269776169, 0.3333333333333333703, 0.3299404806269776169, 0.3333333333333333703, 0.3299404806269776169, 0.3333333333333333703, 0.3299404806269776169, 0.3333333333333333703, 0.3299404806269776169, 0.3333333333333333703, 0.3299404806269776169, 0.3333333333333333703, 0.3299404806269776169, 0.3333333333333333703, 0.3299404806269776169, 0.3333333333333333703, 0.3299404806269776169, 0.3333333333333333703, 0.3299404806269776169, 0.3333333333333333703, 0.3299404806269776169, 0.3333333333333333703, 0.3299404806269776169, 0.3333333333333333703, 0.3299404806269776169, 0.3333333333333333703, 0.3299404806269776169, 0.3333333333333333703, 0.3299404806269776169, 0.3333333333333333703, 0.3299404806269776169, 0.3333333333333333703, 0.3299404806269776169, 0.3333333333333333703, 0.3299404806269776169, 0.3333333333333333703, 0.3299404806269776169, 0.3333333333333333703, 0.3299404806269776169, 0.3333333333333333703, 0.3299404806269776169, 0.3333333333333333703, 0.3299404806269776169, 0.3333333333333333703, 0.3299404806269776169, 0.3333333333333333703, 0.3299404806269776169, 0.3333333333333333703, 0.3299404806269776169, 0.3333333333333333703, 0.3299404806269776169, 0.3333333333333333703, 0.3299404806269776169, 0.3333333333333333703, 0.3299404806269776169, 0.3333333333333333703, 0.3299404806269776169, 0.3333333333333333703, 0.3299404806269776169, 0.3333333333333333703, 0.3299404806269776169, 0.3333333333333333703, 0.3299404806269776169, 0.3333333333333333703, 0.3299404806269776169, 0.3333333333333333703, 0.3299404806269776169, 0.3333333333333333703, 0.3299404806269776169, 0.3333333333333333703, 0.3299404806269776169, 0.3333333333333333703, 0.3299404806269776169, 0.3333333333333333703, 0.3299404806269776169, 0.3333333333333333703, 0.3299404806269776169, 0.3333333333333333703, 0.3299404806269776169, 0.3333333333333333703, 0.3299404806269776169, 0.3333333333333333703, 0.3299404806269776169, 0.3333333333333333703, 0.3299404806269776169, 0.3333333333333333703, 0.3299404806269776169, 0.3333333333333333703, 0.3299404806269776169, 0.3333333333333333703, 0.3299404806269776169, 0.3333333333333333703, 0.3299404806269776169, 0.3333333333333333703, 0.3299404806269776169, 0.3333333333333333703, 0.3299404806269776169, 0.3333333333333333703, 0.3299404806269776169, 0.3333333333333333703, 0.3299404806269776169, 0.3333333333333333703, 0.3299404806269776169, 0.3333333333333333703, 0.3299404806269776169, 0.3333333333333333703, 0.3299404806269776169, 0.3333333333333333703, 0.3299404806269776169, 0.3333333333333333703, 0.3299404806269776169, 0.3333333333333333703, 0.3299404806269776169, 0.3333333333333333703, 0.3299404806269776169, 0.3333333333333333703, 0.3299404806269776169, 0.3333333333333333703, 0.3299404806269776169, 0.3333333333333333703, 0.3299404806269776169, 0.3333333333333333703, 0.3299404806269776169, 0.3333333333333333703, 0.3299404806269776169, 0.3333333333333333703, 0.3299404806269776169, 0.3333333333333333703, 0.3299404806269776169, 0.3333333333333333703, 0.3299404806269776169, 0.3333333333333333703, 0.3299404806269776169, 0.3333333333333333703, 0.3299404806269776169, 0.3333333333333333703, 0.3299404806269776169, 0.3333333333333333703, 0.3299404806269776169, 0.3333333333333333703, 0.3299404806269776169, 0.3333333333333333703, 0.3299404806269776169, 0.3333333333333333703, 0.3299404806269776169, 0.3333333333333333703, 0.3299404806269776169, 0.3333333333333333703, 0.3299404806269776169, 0.3333333333333333703, 0.3299404806269776169, 0.3333333333333333703, 0.3299404806269776169, 0.3333333333333333703, 0.3299404806269776169, 0.3333333333333333703, 0.3299404806269776169, 0.3333333333333333703, 0.3299404806269776169, 0.3333333333333333703, 0.3299404806269776169, 0.3333333333333333703, 0.3299404806269776169, 0.3333333333333333703, 0.3299404806269776169, 0.3333333333333333703, 0.3299404806269776169, 0.3333333333333333703, 0.3299404806269776169, 0.3333333333333333703, 0.3299404806269776169, 0.3333333333333333703, 0.3299404806269776169, 0.3333333333333333703, 0.3299404806269776169, 0.3333333333333333703, 0.3299404806269776169, 0.3333333333333333703, 0.3299404806269776169, 0.3333333333333333703, 0.3299404806269776169, 0.3333333333333333703, 0.3299404806269776169, 0.3333333333333333703, 0.3299404806269776169, 0.3333333333333333703, 0.3299404806269776169, 0.3333333333333333703, 0.3299404806269776169, 0.3333333333333333703, 0.3299404806269776169, 0.3333333333333333703, 0.3299404806269776169, 0.3333333333333333703, 0.3299404806269776169, 0.3333333333333333703, 0.3299404806269776169, 0.3333333333333333703, 0.3299404806269776169, 0.3333333333333333703, 0.3299404806269776169, 0.3333333333333333703, 0.3299404806269776169, 0.3333333333333333703, 0.3299404806269776169, 0.3333333333333333703, 0.3299404806269776169, 0.3333333333333333703, 0.3299404806269776169, 0.3333333333333333703, 0.3299404806269776169, 0.3333333333333333703, 0.3299404806269776169, 0.3333333333333333703, 0.3299404806269776169, 0.3333333333333333703, 0.3299404806269776169, 0.3333333333333333703, 0.3299404806269776169, 0.3333333333333333703, 0.3299404806269776169, 0.3333333333333333703, 0.3299404806269776169, 0.3333333333333333703, 0.3299404806269776169, 0.3333333333333333703, 0.3299404806269776169, 0.3333333333333333703, 0.3299404806269776169, 0.3333333333333333703, 0.3299404806269776169, 0.3333333333333333703, 0.3299404806269776169, 0.3333333333333333703, 0.3299404806269776169, 0.3333333333333333703, 0.3299404806269776169, 0.3333333333333333703, 0.3299404806269776169, 0.3333333333333333703, 0.3299404806269776169, 0.3333333333333333703, 0.3299404806269776169, 0.3333333333333333703, 0.3299404806269776169, 0.3333333333333333703, 0.3299404806269776169, 0.3333333333333333703, 0.3299404806269776169, 0.3333333333333333703, 0.3299404806269776169, 0.3333333333333333703, 0.3299404806269776169, 0.3333333333333333703, 0.3299404806269776169, 0.3333333333333333703, 0.3299404806269776169, 0.3333333333333333703, 0.3299404806269776169, 0.3333333333333333703, 0.3299404806269776169, 0.3333333333333333703, 0.3299404806269776169, 0.3333333333333333703, 0.3299404806269776169, 0.3333333333333333703, 0.3299404806269776169, 0.3333333333333333703, 0.3299404806269776169, 0.3333333333333333703, 0.3299404806269776169, 0.3333333333333333703, 0.3299404806269776169, 0.3333333333333333703, 0.3299404806269776169, 0.3333333333333333703, 0.3299404806269776169, 0.3333333333333333703, 0.3299404806269776169, 0.3333333333333333703, 0.3299404806269776169, 0.3333333333333333703, 0.3299404806269776169, 0.3333333333333333703, 0.3299404806269776169, 0.3333333333333333703, 0.3299404806269776169, 0.3333333333333333703, 0.3299404806269776169, 0.3333333333333333703, 0.3299404806269776169, 0.3333333333333333703, 0.3299404806269776169, 0.3333333333333333703, 0.3299404806269776169, 0.3333333333333333703, 0.3299404806269776169, 0.3333333333333333703, 0.3299404806269776169, 0.3333333333333333703, 0.3299404806269776169, 0.3333333333333333703, 0.3299404806269776169, 0.3333333333333333703, 0.3299404806269776169, 0.3333333333333333703, 0.3299404806269776169, 0.3333333333333333703, 0.3299404806269776169, 0.3333333333333333703, 0.3299404806269776169, 0.3333333333333333703, 0.3299404806269776169, 0.3333333333333333703, 0.3320603117974822438, 0.3317425830320511193),
 ( 0.3333333333333333703, 0.3299404806269776169, 0.3333333333333333703, 0.3299404806269776169, 0.3333333333333333703, 0.3299404806269776169, 0.3333333333333333703, 0.3299404806269776169, 0.3333333333333333703, 0.3299404806269776169, 0.3333333333333333703, 0.3299404806269776169, 0.3333333333333333703, 0.3299404806269776169, 0.3333333333333333703, 0.3299404806269776169, 0.3333333333333333703, 0.3299404806269776169, 0.3333333333333333703, 0.3299404806269776169, 0.3333333333333333703, 0.3299404806269776169, 0.3333333333333333703, 0.3299404806269776169, 0.3333333333333333703, 0.3299404806269776169, 0.3333333333333333703, 0.3299404806269776169, 0.3333333333333333703, 0.3299404806269776169, 0.3333333333333333703, 0.3299404806269776169, 0.3333333333333333703, 0.3299404806269776169, 0.3333333333333333703, 0.3299404806269776169, 0.3333333333333333703, 0.3299404806269776169, 0.3333333333333333703, 0.3299404806269776169, 0.3333333333333333703, 0.3299404806269776169, 0.3333333333333333703, 0.3299404806269776169, 0.3333333333333333703, 0.3299404806269776169, 0.3333333333333333703, 0.3299404806269776169, 0.3333333333333333703, 0.3299404806269776169, 0.3333333333333333703, 0.3299404806269776169, 0.3333333333333333703, 0.3299404806269776169, 0.3333333333333333703, 0.3299404806269776169, 0.3333333333333333703, 0.3299404806269776169, 0.3333333333333333703, 0.3299404806269776169, 0.3333333333333333703, 0.3299404806269776169, 0.3333333333333333703, 0.3299404806269776169, 0.3333333333333333703, 0.3299404806269776169, 0.3333333333333333703, 0.3299404806269776169, 0.3333333333333333703, 0.3299404806269776169, 0.3333333333333333703, 0.3299404806269776169, 0.3333333333333333703, 0.3299404806269776169, 0.3333333333333333703, 0.3299404806269776169, 0.3333333333333333703, 0.3299404806269776169, 0.3333333333333333703, 0.3299404806269776169, 0.3333333333333333703, 0.3299404806269776169, 0.3333333333333333703, 0.3299404806269776169, 0.3333333333333333703, 0.3299404806269776169, 0.3333333333333333703, 0.3299404806269776169, 0.3333333333333333703, 0.3299404806269776169, 0.3333333333333333703, 0.3299404806269776169, 0.3333333333333333703, 0.3299404806269776169, 0.3333333333333333703, 0.3299404806269776169, 0.3333333333333333703, 0.3299404806269776169, 0.3333333333333333703, 0.3299404806269776169, 0.3333333333333333703, 0.3299404806269776169, 0.3333333333333333703, 0.3299404806269776169, 0.3333333333333333703, 0.3299404806269776169, 0.3333333333333333703, 0.3299404806269776169, 0.3333333333333333703, 0.3299404806269776169, 0.3333333333333333703, 0.3299404806269776169, 0.3333333333333333703, 0.3299404806269776169, 0.3333333333333333703, 0.3299404806269776169, 0.3333333333333333703, 0.3299404806269776169, 0.3333333333333333703, 0.3299404806269776169, 0.3333333333333333703, 0.3299404806269776169, 0.3333333333333333703, 0.3299404806269776169, 0.3333333333333333703, 0.3299404806269776169, 0.3333333333333333703, 0.3299404806269776169, 0.3333333333333333703, 0.3299404806269776169, 0.3333333333333333703, 0.3299404806269776169, 0.3333333333333333703, 0.3299404806269776169, 0.3333333333333333703, 0.3299404806269776169, 0.3333333333333333703, 0.3299404806269776169, 0.3333333333333333703, 0.3299404806269776169, 0.3333333333333333703, 0.3299404806269776169, 0.3333333333333333703, 0.3299404806269776169, 0.3333333333333333703, 0.3299404806269776169, 0.3333333333333333703, 0.3299404806269776169, 0.3333333333333333703, 0.3299404806269776169, 0.3333333333333333703, 0.3299404806269776169, 0.3333333333333333703, 0.3299404806269776169, 0.3333333333333333703, 0.3299404806269776169, 0.3333333333333333703, 0.3299404806269776169, 0.3333333333333333703, 0.3299404806269776169, 0.3333333333333333703, 0.3299404806269776169, 0.3333333333333333703, 0.3299404806269776169, 0.3333333333333333703, 0.3299404806269776169, 0.3333333333333333703, 0.3299404806269776169, 0.3333333333333333703, 0.3299404806269776169, 0.3333333333333333703, 0.3299404806269776169, 0.3333333333333333703, 0.3299404806269776169, 0.3333333333333333703, 0.3299404806269776169, 0.3333333333333333703, 0.3299404806269776169, 0.3333333333333333703, 0.3299404806269776169, 0.3333333333333333703, 0.3299404806269776169, 0.3333333333333333703, 0.3299404806269776169, 0.3333333333333333703, 0.3299404806269776169, 0.3333333333333333703, 0.3299404806269776169, 0.3333333333333333703, 0.3299404806269776169, 0.3333333333333333703, 0.3299404806269776169, 0.3333333333333333703, 0.3299404806269776169, 0.3333333333333333703, 0.3299404806269776169, 0.3333333333333333703, 0.3299404806269776169, 0.3333333333333333703, 0.3299404806269776169, 0.3333333333333333703, 0.3299404806269776169, 0.3333333333333333703, 0.3299404806269776169, 0.3333333333333333703, 0.3299404806269776169, 0.3333333333333333703, 0.3299404806269776169, 0.3333333333333333703, 0.3299404806269776169, 0.3333333333333333703, 0.3299404806269776169, 0.3333333333333333703, 0.3299404806269776169, 0.3333333333333333703, 0.3299404806269776169, 0.3333333333333333703, 0.3299404806269776169, 0.3333333333333333703, 0.3299404806269776169, 0.3333333333333333703, 0.3299404806269776169, 0.3333333333333333703, 0.3299404806269776169, 0.3333333333333333703, 0.3299404806269776169, 0.3333333333333333703, 0.3299404806269776169, 0.3333333333333333703, 0.3299404806269776169, 0.3333333333333333703, 0.3299404806269776169, 0.3333333333333333703, 0.3299404806269776169, 0.3333333333333333703, 0.3299404806269776169, 0.3333333333333333703, 0.3299404806269776169, 0.3333333333333333703, 0.3299404806269776169, 0.3333333333333333703, 0.3299404806269776169, 0.3333333333333333703, 0.3299404806269776169, 0.3333333333333333703, 0.3299404806269776169, 0.3333333333333333703, 0.3299404806269776169, 0.3333333333333333703, 0.3299404806269776169, 0.3333333333333333703, 0.3299404806269776169, 0.3333333333333333703, 0.3299404806269776169, 0.3333333333333333703, 0.3299404806269776169, 0.3333333333333333703, 0.3299404806269776169, 0.3333333333333333703, 0.3299404806269776169, 0.3333333333333333703, 0.3299404806269776169, 0.3333333333333333703, 0.3299404806269776169, 0.3333333333333333703, 0.3299404806269776169, 0.3333333333333333703, 0.3299404806269776169, 0.3333333333333333703, 0.3299404806269776169, 0.3333333333333333703, 0.3299404806269776169, 0.3333333333333333703, 0.3299404806269776169, 0.3333333333333333703, 0.3299404806269776169, 0.3333333333333333703, 0.3299404806269776169, 0.3333333333333333703, 0.3299404806269776169, 0.3333333333333333703, 0.3299404806269776169, 0.3333333333333333703, 0.3299404806269776169, 0.3333333333333333703, 0.3299404806269776169, 0.3333333333333333703, 0.3299404806269776169, 0.3333333333333333703, 0.3299404806269776169, 0.3333333333333333703, 0.3299404806269776169, 0.3333333333333333703, 0.3299404806269776169, 0.3333333333333333703, 0.3299404806269776169, 0.3333333333333333703, 0.3299404806269776169, 0.3333333333333333703, 0.3299404806269776169, 0.3333333333333333703, 0.3299404806269776169, 0.3333333333333333703, 0.3299404806269776169, 0.3333333333333333703, 0.3299404806269776169, 0.3333333333333333703, 0.3299404806269776169, 0.3333333333333333703, 0.3299404806269776169, 0.3333333333333333703, 0.3299404806269776169, 0.3333333333333333703, 0.3299404806269776169, 0.3333333333333333703, 0.3299404806269776169, 0.3333333333333333703, 0.3299404806269776169, 0.3333333333333333703, 0.3299404806269776169, 0.3333333333333333703, 0.3299404806269776169, 0.3333333333333333703, 0.3299404806269776169, 0.3333333333333333703, 0.3299404806269776169, 0.3333333333333333703, 0.3299404806269776169, 0.3333333333333333703, 0.3299404806269776169, 0.3333333333333333703, 0.3299404806269776169, 0.3333333333333333703, 0.3299404806269776169, 0.3333333333333333703, 0.3299404806269776169, 0.3333333333333333703, 0.3299404806269776169, 0.3333333333333333703, 0.3299404806269776169, 0.3333333333333333703, 0.3299404806269776169, 0.3333333333333333703, 0.3299404806269776169, 0.3333333333333333703, 0.3299404806269776169, 0.3333333333333333703, 0.3299404806269776169, 0.3333333333333333703, 0.3299404806269776169, 0.3333333333333333703, 0.3299404806269776169, 0.3333333333333333703, 0.3299404806269776169, 0.3333333333333333703, 0.3299404806269776169, 0.3333333333333333703, 0.3299404806269776169, 0.3333333333333333703, 0.3299404806269776169, 0.3333333333333333703, 0.3299404806269776169, 0.3333333333333333703, 0.3299404806269776169, 0.3333333333333333703, 0.3299404806269776169, 0.3333333333333333703, 0.3299404806269776169, 0.3333333333333333703, 0.3299404806269776169, 0.3333333333333333703, 0.3299404806269776169, 0.3333333333333333703, 0.3299404806269776169, 0.3333333333333333703, 0.3299404806269776169, 0.3333333333333333703, 0.3299404806269776169, 0.3333333333333333703, 0.3299404806269776169, 0.3333333333333333703, 0.3299404806269776169, 0.3333333333333333703, 0.3299404806269776169, 0.3333333333333333703, 0.3299404806269776169, 0.3333333333333333703, 0.3299404806269776169, 0.3333333333333333703, 0.3299404806269776169, 0.3333333333333333703, 0.3299404806269776169, 0.3333333333333333703, 0.3299404806269776169, 0.3333333333333333703, 0.3299404806269776169, 0.3333333333333333703, 0.3299404806269776169, 0.3333333333333333703, 0.3299404806269776169, 0.3333333333333333703, 0.3299404806269776169, 0.3333333333333333703, 0.3299404806269776169, 0.3333333333333333703, 0.3299404806269776169, 0.3333333333333333703, 0.3299404806269776169, 0.3333333333333333703, 0.3299404806269776169, 0.3333333333333333703, 0.3299404806269776169, 0.3333333333333333703, 0.3299404806269776169, 0.3333333333333333703, 0.3299404806269776169, 0.3333333333333333703, 0.3299404806269776169, 0.3333333333333333703, 0.3299404806269776169, 0.3333333333333333703, 0.3299404806269776169, 0.3333333333333333703, 0.3299404806269776169, 0.3333333333333333703, 0.3299404806269776169, 0.3333333333333333703, 0.3299404806269776169, 0.3333333333333333703, 0.3299404806269776169, 0.3333333333333333703, 0.3299404806269776169, 0.3333333333333333703, 0.3299404806269776169, 0.3333333333333333703, 0.3299404806269776169, 0.3333333333333333703, 0.3299404806269776169, 0.3333333333333333703, 0.3299404806269776169, 0.3333333333333333703, 0.3299404806269776169, 0.3333333333333333703, 0.3299404806269776169, 0.3333333333333333703, 0.3299404806269776169, 0.3333333333333333703, 0.3299404806269776169, 0.3333333333333333703, 0.3299404806269776169, 0.3333333333333333703, 0.3299404806269776169, 0.3333333333333333703, 0.3299404806269776169, 0.3333333333333333703, 0.3299404806269776169, 0.3333333333333333703, 0.3299404806269776169, 0.3333333333333333703, 0.3299404806269776169, 0.3333333333333333703, 0.3299404806269776169, 0.3333333333333333703, 0.3299404806269776169, 0.3333333333333333703, 0.3299404806269776169, 0.3333333333333333703, 0.3299404806269776169, 0.3333333333333333703, 0.3299404806269776169, 0.3333333333333333703, 0.3299404806269776169, 0.3333333333333333703, 0.3299404806269776169, 0.3333333333333333703, 0.3299404806269776169, 0.3333333333333333703, 0.3299404806269776169, 0.3333333333333333703, 0.3299404806269776169, 0.3333333333333333703, 0.3299404806269776169, 0.3333333333333333703, 0.3299404806269776169, 0.3333333333333333703, 0.3299404806269776169, 0.3333333333333333703, 0.3299404806269776169, 0.3333333333333333703, 0.3299404806269776169, 0.3333333333333333703, 0.3299404806269776169, 0.3333333333333333703, 0.3299404806269776169, 0.3333333333333333703, 0.3299404806269776169, 0.3333333333333333703, 0.3299404806269776169, 0.3333333333333333703, 0.3299404806269776169, 0.3333333333333333703, 0.3299404806269776169, 0.3333333333333333703, 0.3299404806269776169, 0.3333333333333333703, 0.3299404806269776169, 0.3333333333333333703, 0.3299404806269776169, 0.3333333333333333703, 0.3299404806269776169, 0.3333333333333333703, 0.3299404806269776169, 0.3333333333333333703, 0.3299404806269776169, 0.3333333333333333703, 0.3299404806269776169, 0.3333333333333333703, 0.3299404806269776169, 0.3333333333333333703, 0.3299404806269776169, 0.3333333333333333703, 0.3299404806269776169, 0.3333333333333333703, 0.3299404806269776169, 0.3333333333333333703, 0.3299404806269776169, 0.3333333333333333703, 0.3299404806269776169, 0.3333333333333333703, 0.3299404806269776169, 0.3333333333333333703, 0.3299404806269776169, 0.3333333333333333703, 0.3299404806269776169, 0.3333333333333333703, 0.3299404806269776169, 0.3333333333333333703, 0.3299404806269776169, 0.3333333333333333703, 0.3299404806269776169, 0.3333333333333333703, 0.3299404806269776169, 0.3333333333333333703, 0.3299404806269776169, 0.3333333333333333703, 0.3299404806269776169, 0.3333333333333333703, 0.3299404806269776169, 0.3333333333333333703, 0.3299404806269776169, 0.3333333333333333703, 0.3299404806269776169, 0.3333333333333333703, 0.3299404806269776169, 0.3333333333333333703, 0.3299404806269776169, 0.3333333333333333703, 0.3299404806269776169, 0.3333333333333333703, 0.3299404806269776169, 0.3333333333333333703, 0.3299404806269776169, 0.3333333333333333703, 0.3299404806269776169, 0.3333333333333333703, 0.3299404806269776169, 0.3333333333333333703, 0.3299404806269776169, 0.3333333333333333703, 0.3299404806269776169, 0.3333333333333333703, 0.3299404806269776169, 0.3333333333333333703, 0.3299404806269776169, 0.3333333333333333703, 0.3299404806269776169, 0.3333333333333333703, 0.3299404806269776169, 0.3333333333333333703, 0.3299404806269776169, 0.3333333333333333703, 0.3299404806269776169, 0.3333333333333333703, 0.3299404806269776169, 0.3333333333333333703, 0.3299404806269776169, 0.3333333333333333703, 0.3299404806269776169, 0.3333333333333333703, 0.3299404806269776169, 0.3333333333333333703, 0.3299404806269776169, 0.3333333333333333703, 0.3299404806269776169, 0.3333333333333333703, 0.3299404806269776169, 0.3333333333333333703, 0.3299404806269776169, 0.3333333333333333703, 0.3299404806269776169, 0.3333333333333333703, 0.3299404806269776169, 0.3333333333333333703, 0.3299404806269776169, 0.3333333333333333703, 0.3299404806269776169, 0.3333333333333333703, 0.3299404806269776169, 0.3333333333333333703, 0.3299404806269776169, 0.3333333333333333703, 0.3299404806269776169, 0.3333333333333333703, 0.3299404806269776169, 0.3333333333333333703, 0.3299404806269776169, 0.3333333333333333703, 0.3299404806269776169, 0.3333333333333333703, 0.3299404806269776169, 0.3333333333333333703, 0.3299404806269776169, 0.3333333333333333703, 0.3299404806269776169, 0.3333333333333333703, 0.3299404806269776169, 0.3333333333333333703, 0.3299404806269776169, 0.3333333333333333703, 0.3299404806269776169, 0.3333333333333333703, 0.3299404806269776169, 0.3333333333333333703, 0.3299404806269776169, 0.3333333333333333703, 0.3299404806269776169, 0.3333333333333333703, 0.3299404806269776169, 0.3333333333333333703, 0.3299404806269776169, 0.3333333333333333703, 0.3299404806269776169, 0.3333333333333333703, 0.3299404806269776169, 0.3333333333333333703, 0.3299404806269776169, 0.3333333333333333703, 0.3299404806269776169, 0.3333333333333333703, 0.3299404806269776169, 0.3333333333333333703, 0.3299404806269776169, 0.3333333333333333703, 0.3299404806269776169, 0.3333333333333333703, 0.3299404806269776169, 0.3333333333333333703, 0.3299404806269776169, 0.3333333333333333703, 0.3299404806269776169, 0.3333333333333333703, 0.3299404806269776169, 0.3333333333333333703, 0.3299404806269776169, 0.3333333333333333703, 0.3299404806269776169, 0.3333333333333333703, 0.3299404806269776169, 0.3333333333333333703, 0.3299404806269776169, 0.3333333333333333703, 0.3299404806269776169, 0.3333333333333333703, 0.3299404806269776169, 0.3333333333333333703, 0.3299404806269776169, 0.3333333333333333703, 0.3299404806269776169, 0.3333333333333333703, 0.3299404806269776169, 0.3333333333333333703, 0.3299404806269776169, 0.3333333333333333703, 0.3299404806269776169, 0.3333333333333333703, 0.3299404806269776169, 0.3333333333333333703, 0.3299404806269776169, 0.3333333333333333703, 0.3299404806269776169, 0.3333333333333333703, 0.3299404806269776169, 0.3333333333333333703, 0.3299404806269776169, 0.3333333333333333703, 0.3299404806269776169, 0.3333333333333333703, 0.3299404806269776169, 0.3333333333333333703, 0.3299404806269776169, 0.3333333333333333703, 0.3299404806269776169, 0.3333333333333333703, 0.3299404806269776169, 0.3333333333333333703, 0.3299404806269776169, 0.3333333333333333703, 0.3299404806269776169, 0.3333333333333333703, 0.3299404806269776169, 0.3333333333333333703, 0.3299404806269776169, 0.3333333333333333703, 0.3299404806269776169, 0.3333333333333333703, 0.3299404806269776169, 0.3333333333333333703, 0.3299404806269776169, 0.3333333333333333703, 0.3299404806269776169, 0.3333333333333333703, 0.3299404806269776169, 0.3333333333333333703, 0.3299404806269776169, 0.3333333333333333703, 0.3299404806269776169, 0.3333333333333333703, 0.3299404806269776169, 0.3333333333333333703, 0.3299404806269776169, 0.3333333333333333703, 0.3299404806269776169, 0.3333333333333333703, 0.3299404806269776169, 0.3333333333333333703, 0.3299404806269776169, 0.3333333333333333703, 0.3299404806269776169, 0.3333333333333333703, 0.3299404806269776169, 0.3333333333333333703, 0.3299404806269776169, 0.3333333333333333703, 0.3299404806269776169, 0.3333333333333333703, 0.3299404806269776169, 0.3333333333333333703, 0.3299404806269776169, 0.3333333333333333703, 0.3299404806269776169, 0.3333333333333333703, 0.3299404806269776169, 0.3333333333333333703, 0.3299404806269776169, 0.3333333333333333703, 0.3299404806269776169, 0.3333333333333333703, 0.3299404806269776169, 0.3333333333333333703, 0.3299404806269776169, 0.3333333333333333703, 0.3299404806269776169, 0.3333333333333333703, 0.3299404806269776169, 0.3333333333333333703, 0.3299404806269776169, 0.3333333333333333703, 0.3299404806269776169, 0.3333333333333333703, 0.3299404806269776169, 0.3333333333333333703, 0.3299404806269776169, 0.3333333333333333703, 0.3299404806269776169, 0.3333333333333333703, 0.3299404806269776169, 0.3333333333333333703, 0.3299404806269776169, 0.3333333333333333703, 0.3299404806269776169, 0.3333333333333333703, 0.3299404806269776169, 0.3333333333333333703, 0.3299404806269776169, 0.3333333333333333703, 0.3299404806269776169, 0.3333333333333333703, 0.3299404806269776169, 0.3333333333333333703, 0.3299404806269776169, 0.3333333333333333703, 0.3299404806269776169, 0.3333333333333333703, 0.3299404806269776169, 0.3333333333333333703, 0.3299404806269776169, 0.3333333333333333703, 0.3299404806269776169, 0.3333333333333333703, 0.3299404806269776169, 0.3333333333333333703, 0.3299404806269776169, 0.3333333333333333703, 0.3299404806269776169, 0.3333333333333333703, 0.3299404806269776169, 0.3333333333333333703, 0.3299404806269776169, 0.3333333333333333703, 0.3299404806269776169, 0.3333333333333333703, 0.3299404806269776169, 0.3333333333333333703, 0.3299404806269776169, 0.3333333333333333703, 0.3299404806269776169, 0.3333333333333333703, 0.3299404806269776169, 0.3333333333333333703, 0.3299404806269776169, 0.3333333333333333703, 0.3299404806269776169, 0.3333333333333333703, 0.3299404806269776169, 0.3333333333333333703, 0.3299404806269776169, 0.3333333333333333703, 0.3299404806269776169, 0.3333333333333333703, 0.3299404806269776169, 0.3333333333333333703, 0.3299404806269776169, 0.3333333333333333703, 0.3299404806269776169, 0.3333333333333333703, 0.3299404806269776169, 0.3333333333333333703, 0.3299404806269776169, 0.3333333333333333703, 0.3299404806269776169, 0.3333333333333333703, 0.3299404806269776169, 0.3333333333333333703, 0.3299404806269776169, 0.3333333333333333703, 0.3299404806269776169, 0.3333333333333333703, 0.3299404806269776169, 0.3333333333333333703, 0.3299404806269776169, 0.3333333333333333703, 0.3299404806269776169, 0.3333333333333333703, 0.3299404806269776169, 0.3333333333333333703, 0.3299404806269776169, 0.3333333333333333703, 0.3299404806269776169, 0.3333333333333333703, 0.3299404806269776169, 0.3333333333333333703, 0.3320603117974822438, 0.3317425830320511193),
 ( 1.000000000000000000, 0.9898214418809326842, 1.000000000000000000, 0.9898214418809326842, 1.000000000000000000, 0.9898214418809326842, 1.000000000000000000, 0.9898214418809326842, 1.000000000000000000, 0.9898214418809326842, 1.000000000000000000, 0.9898214418809326842, 1.000000000000000000, 0.9898214418809326842, 1.000000000000000000, 0.9898214418809326842, 1.000000000000000000, 0.9898214418809326842, 1.000000000000000000, 0.9898214418809326842, 1.000000000000000000, 0.9898214418809326842, 1.000000000000000000, 0.9898214418809326842, 1.000000000000000000, 0.9898214418809326842, 1.000000000000000000, 0.9898214418809326842, 1.000000000000000000, 0.9898214418809326842, 1.000000000000000000, 0.9898214418809326842, 1.000000000000000000, 0.9898214418809326842, 1.000000000000000000, 0.9898214418809326842, 1.000000000000000000, 0.9898214418809326842, 1.000000000000000000, 0.9898214418809326842, 1.000000000000000000, 0.9898214418809326842, 1.000000000000000000, 0.9898214418809326842, 1.000000000000000000, 0.9898214418809326842, 1.000000000000000000, 0.9898214418809326842, 1.000000000000000000, 0.9898214418809326842, 1.000000000000000000, 0.9898214418809326842, 1.000000000000000000, 0.9898214418809326842, 1.000000000000000000, 0.9898214418809326842, 1.000000000000000000, 0.9898214418809326842, 1.000000000000000000, 0.9898214418809326842, 1.000000000000000000, 0.9898214418809326842, 1.000000000000000000, 0.9898214418809326842, 1.000000000000000000, 0.9898214418809326842, 1.000000000000000000, 0.9898214418809326842, 1.000000000000000000, 0.9898214418809326842, 1.000000000000000000, 0.9898214418809326842, 1.000000000000000000, 0.9898214418809326842, 1.000000000000000000, 0.9898214418809326842, 1.000000000000000000, 0.9898214418809326842, 1.000000000000000000, 0.9898214418809326842, 1.000000000000000000, 0.9898214418809326842, 1.000000000000000000, 0.9898214418809326842, 1.000000000000000000, 0.9898214418809326842, 1.000000000000000000, 0.9898214418809326842, 1.000000000000000000, 0.9898214418809326842, 1.000000000000000000, 0.9898214418809326842, 1.000000000000000000, 0.9898214418809326842, 1.000000000000000000, 0.9898214418809326842, 1.000000000000000000, 0.9898214418809326842, 1.000000000000000000, 0.9898214418809326842, 1.000000000000000000, 0.9898214418809326842, 1.000000000000000000, 0.9898214418809326842, 1.000000000000000000, 0.9898214418809326842, 1.000000000000000000, 0.9898214418809326842, 1.000000000000000000, 0.9898214418809326842, 1.000000000000000000, 0.9898214418809326842, 1.000000000000000000, 0.9898214418809326842, 1.000000000000000000, 0.9898214418809326842, 1.000000000000000000, 0.9898214418809326842, 1.000000000000000000, 0.9898214418809326842, 1.000000000000000000, 0.9898214418809326842, 1.000000000000000000, 0.9898214418809326842, 1.000000000000000000, 0.9898214418809326842, 1.000000000000000000, 0.9898214418809326842, 1.000000000000000000, 0.9898214418809326842, 1.000000000000000000, 0.9898214418809326842, 1.000000000000000000, 0.9898214418809326842, 1.000000000000000000, 0.9898214418809326842, 1.000000000000000000, 0.9898214418809326842, 1.000000000000000000, 0.9898214418809326842, 1.000000000000000000, 0.9898214418809326842, 1.000000000000000000, 0.9898214418809326842, 1.000000000000000000, 0.9898214418809326842, 1.000000000000000000, 0.9898214418809326842, 1.000000000000000000, 0.9898214418809326842, 1.000000000000000000, 0.9898214418809326842, 1.000000000000000000, 0.9898214418809326842, 1.000000000000000000, 0.9898214418809326842, 1.000000000000000000, 0.9898214418809326842, 1.000000000000000000, 0.9898214418809326842, 1.000000000000000000, 0.9898214418809326842, 1.000000000000000000, 0.9898214418809326842, 1.000000000000000000, 0.9898214418809326842, 1.000000000000000000, 0.9898214418809326842, 1.000000000000000000, 0.9898214418809326842, 1.000000000000000000, 0.9898214418809326842, 1.000000000000000000, 0.9898214418809326842, 1.000000000000000000, 0.9898214418809326842, 1.000000000000000000, 0.9898214418809326842, 1.000000000000000000, 0.9898214418809326842, 1.000000000000000000, 0.9898214418809326842, 1.000000000000000000, 0.9898214418809326842, 1.000000000000000000, 0.9898214418809326842, 1.000000000000000000, 0.9898214418809326842, 1.000000000000000000, 0.9898214418809326842, 1.000000000000000000, 0.9898214418809326842, 1.000000000000000000, 0.9898214418809326842, 1.000000000000000000, 0.9898214418809326842, 1.000000000000000000, 0.9898214418809326842, 1.000000000000000000, 0.9898214418809326842, 1.000000000000000000, 0.9898214418809326842, 1.000000000000000000, 0.9898214418809326842, 1.000000000000000000, 0.9898214418809326842, 1.000000000000000000, 0.9898214418809326842, 1.000000000000000000, 0.9898214418809326842, 1.000000000000000000, 0.9898214418809326842, 1.000000000000000000, 0.9898214418809326842, 1.000000000000000000, 0.9898214418809326842, 1.000000000000000000, 0.9898214418809326842, 1.000000000000000000, 0.9898214418809326842, 1.000000000000000000, 0.9898214418809326842, 1.000000000000000000, 0.9898214418809326842, 1.000000000000000000, 0.9898214418809326842, 1.000000000000000000, 0.9898214418809326842, 1.000000000000000000, 0.9898214418809326842, 1.000000000000000000, 0.9898214418809326842, 1.000000000000000000, 0.9898214418809326842, 1.000000000000000000, 0.9898214418809326842, 1.000000000000000000, 0.9898214418809326842, 1.000000000000000000, 0.9898214418809326842, 1.000000000000000000, 0.9898214418809326842, 1.000000000000000000, 0.9898214418809326842, 1.000000000000000000, 0.9898214418809326842, 1.000000000000000000, 0.9898214418809326842, 1.000000000000000000, 0.9898214418809326842, 1.000000000000000000, 0.9898214418809326842, 1.000000000000000000, 0.9898214418809326842, 1.000000000000000000, 0.9898214418809326842, 1.000000000000000000, 0.9898214418809326842, 1.000000000000000000, 0.9898214418809326842, 1.000000000000000000, 0.9898214418809326842, 1.000000000000000000, 0.9898214418809326842, 1.000000000000000000, 0.9898214418809326842, 1.000000000000000000, 0.9898214418809326842, 1.000000000000000000, 0.9898214418809326842, 1.000000000000000000, 0.9898214418809326842, 1.000000000000000000, 0.9898214418809326842, 1.000000000000000000, 0.9898214418809326842, 1.000000000000000000, 0.9898214418809326842, 1.000000000000000000, 0.9898214418809326842, 1.000000000000000000, 0.9898214418809326842, 1.000000000000000000, 0.9898214418809326842, 1.000000000000000000, 0.9898214418809326842, 1.000000000000000000, 0.9898214418809326842, 1.000000000000000000, 0.9898214418809326842, 1.000000000000000000, 0.9898214418809326842, 1.000000000000000000, 0.9898214418809326842, 1.000000000000000000, 0.9898214418809326842, 1.000000000000000000, 0.9898214418809326842, 1.000000000000000000, 0.9898214418809326842, 1.000000000000000000, 0.9898214418809326842, 1.000000000000000000, 0.9898214418809326842, 1.000000000000000000, 0.9898214418809326842, 1.000000000000000000, 0.9898214418809326842, 1.000000000000000000, 0.9898214418809326842, 1.000000000000000000, 0.9898214418809326842, 1.000000000000000000, 0.9898214418809326842, 1.000000000000000000, 0.9898214418809326842, 1.000000000000000000, 0.9898214418809326842, 1.000000000000000000, 0.9898214418809326842, 1.000000000000000000, 0.9898214418809326842, 1.000000000000000000, 0.9898214418809326842, 1.000000000000000000, 0.9898214418809326842, 1.000000000000000000, 0.9898214418809326842, 1.000000000000000000, 0.9898214418809326842, 1.000000000000000000, 0.9898214418809326842, 1.000000000000000000, 0.9898214418809326842, 1.000000000000000000, 0.9898214418809326842, 1.000000000000000000, 0.9898214418809326842, 1.000000000000000000, 0.9898214418809326842, 1.000000000000000000, 0.9898214418809326842, 1.000000000000000000, 0.9898214418809326842, 1.000000000000000000, 0.9898214418809326842, 1.000000000000000000, 0.9898214418809326842, 1.000000000000000000, 0.9898214418809326842, 1.000000000000000000, 0.9898214418809326842, 1.000000000000000000, 0.9898214418809326842, 1.000000000000000000, 0.9898214418809326842, 1.000000000000000000, 0.9898214418809326842, 1.000000000000000000, 0.9898214418809326842, 1.000000000000000000, 0.9898214418809326842, 1.000000000000000000, 0.9898214418809326842, 1.000000000000000000, 0.9898214418809326842, 1.000000000000000000, 0.9898214418809326842, 1.000000000000000000, 0.9898214418809326842, 1.000000000000000000, 0.9898214418809326842, 1.000000000000000000, 0.9898214418809326842, 1.000000000000000000, 0.9898214418809326842, 1.000000000000000000, 0.9898214418809326842, 1.000000000000000000, 0.9898214418809326842, 1.000000000000000000, 0.9898214418809326842, 1.000000000000000000, 0.9898214418809326842, 1.000000000000000000, 0.9898214418809326842, 1.000000000000000000, 0.9898214418809326842, 1.000000000000000000, 0.9898214418809326842, 1.000000000000000000, 0.9898214418809326842, 1.000000000000000000, 0.9898214418809326842, 1.000000000000000000, 0.9898214418809326842, 1.000000000000000000, 0.9898214418809326842, 1.000000000000000000, 0.9898214418809326842, 1.000000000000000000, 0.9898214418809326842, 1.000000000000000000, 0.9898214418809326842, 1.000000000000000000, 0.9898214418809326842, 1.000000000000000000, 0.9898214418809326842, 1.000000000000000000, 0.9898214418809326842, 1.000000000000000000, 0.9898214418809326842, 1.000000000000000000, 0.9898214418809326842, 1.000000000000000000, 0.9898214418809326842, 1.000000000000000000, 0.9898214418809326842, 1.000000000000000000, 0.9898214418809326842, 1.000000000000000000, 0.9898214418809326842, 1.000000000000000000, 0.9898214418809326842, 1.000000000000000000, 0.9898214418809326842, 1.000000000000000000, 0.9898214418809326842, 1.000000000000000000, 0.9898214418809326842, 1.000000000000000000, 0.9898214418809326842, 1.000000000000000000, 0.9898214418809326842, 1.000000000000000000, 0.9898214418809326842, 1.000000000000000000, 0.9898214418809326842, 1.000000000000000000, 0.9898214418809326842, 1.000000000000000000, 0.9898214418809326842, 1.000000000000000000, 0.9898214418809326842, 1.000000000000000000, 0.9898214418809326842, 1.000000000000000000, 0.9898214418809326842, 1.000000000000000000, 0.9898214418809326842, 1.000000000000000000, 0.9898214418809326842, 1.000000000000000000, 0.9898214418809326842, 1.000000000000000000, 0.9898214418809326842, 1.000000000000000000, 0.9898214418809326842, 1.000000000000000000, 0.9898214418809326842, 1.000000000000000000, 0.9898214418809326842, 1.000000000000000000, 0.9898214418809326842, 1.000000000000000000, 0.9898214418809326842, 1.000000000000000000, 0.9898214418809326842, 1.000000000000000000, 0.9898214418809326842, 1.000000000000000000, 0.9898214418809326842, 1.000000000000000000, 0.9898214418809326842, 1.000000000000000000, 0.9898214418809326842, 1.000000000000000000, 0.9898214418809326842, 1.000000000000000000, 0.9898214418809326842, 1.000000000000000000, 0.9898214418809326842, 1.000000000000000000, 0.9898214418809326842, 1.000000000000000000, 0.9898214418809326842, 1.000000000000000000, 0.9898214418809326842, 1.000000000000000000, 0.9898214418809326842, 1.000000000000000000, 0.9898214418809326842, 1.000000000000000000, 0.9898214418809326842, 1.000000000000000000, 0.9898214418809326842, 1.000000000000000000, 0.9898214418809326842, 1.000000000000000000, 0.9898214418809326842, 1.000000000000000000, 0.9898214418809326842, 1.000000000000000000, 0.9898214418809326842, 1.000000000000000000, 0.9898214418809326842, 1.000000000000000000, 0.9898214418809326842, 1.000000000000000000, 0.9898214418809326842, 1.000000000000000000, 0.9898214418809326842, 1.000000000000000000, 0.9898214418809326842, 1.000000000000000000, 0.9898214418809326842, 1.000000000000000000, 0.9898214418809326842, 1.000000000000000000, 0.9898214418809326842, 1.000000000000000000, 0.9898214418809326842, 1.000000000000000000, 0.9898214418809326842, 1.000000000000000000, 0.9898214418809326842, 1.000000000000000000, 0.9898214418809326842, 1.000000000000000000, 0.9898214418809326842, 1.000000000000000000, 0.9898214418809326842, 1.000000000000000000, 0.9898214418809326842, 1.000000000000000000, 0.9898214418809326842, 1.000000000000000000, 0.9898214418809326842, 1.000000000000000000, 0.9898214418809326842, 1.000000000000000000, 0.9898214418809326842, 1.000000000000000000, 0.9898214418809326842, 1.000000000000000000, 0.9898214418809326842, 1.000000000000000000, 0.9898214418809326842, 1.000000000000000000, 0.9898214418809326842, 1.000000000000000000, 0.9898214418809326842, 1.000000000000000000, 0.9898214418809326842, 1.000000000000000000, 0.9898214418809326842, 1.000000000000000000, 0.9898214418809326842, 1.000000000000000000, 0.9898214418809326842, 1.000000000000000000, 0.9898214418809326842, 1.000000000000000000, 0.9898214418809326842, 1.000000000000000000, 0.9898214418809326842, 1.000000000000000000, 0.9898214418809326842, 1.000000000000000000, 0.9898214418809326842, 1.000000000000000000, 0.9898214418809326842, 1.000000000000000000, 0.9898214418809326842, 1.000000000000000000, 0.9898214418809326842, 1.000000000000000000, 0.9898214418809326842, 1.000000000000000000, 0.9898214418809326842, 1.000000000000000000, 0.9898214418809326842, 1.000000000000000000, 0.9898214418809326842, 1.000000000000000000, 0.9898214418809326842, 1.000000000000000000, 0.9898214418809326842, 1.000000000000000000, 0.9898214418809326842, 1.000000000000000000, 0.9898214418809326842, 1.000000000000000000, 0.9898214418809326842, 1.000000000000000000, 0.9898214418809326842, 1.000000000000000000, 0.9898214418809326842, 1.000000000000000000, 0.9898214418809326842, 1.000000000000000000, 0.9898214418809326842, 1.000000000000000000, 0.9898214418809326842, 1.000000000000000000, 0.9898214418809326842, 1.000000000000000000, 0.9898214418809326842, 1.000000000000000000, 0.9898214418809326842, 1.000000000000000000, 0.9898214418809326842, 1.000000000000000000, 0.9898214418809326842, 1.000000000000000000, 0.9898214418809326842, 1.000000000000000000, 0.9898214418809326842, 1.000000000000000000, 0.9898214418809326842, 1.000000000000000000, 0.9898214418809326842, 1.000000000000000000, 0.9898214418809326842, 1.000000000000000000, 0.9898214418809326842, 1.000000000000000000, 0.9898214418809326842, 1.000000000000000000, 0.9898214418809326842, 1.000000000000000000, 0.9898214418809326842, 1.000000000000000000, 0.9898214418809326842, 1.000000000000000000, 0.9898214418809326842, 1.000000000000000000, 0.9898214418809326842, 1.000000000000000000, 0.9898214418809326842, 1.000000000000000000, 0.9898214418809326842, 1.000000000000000000, 0.9898214418809326842, 1.000000000000000000, 0.9898214418809326842, 1.000000000000000000, 0.9898214418809326842, 1.000000000000000000, 0.9898214418809326842, 1.000000000000000000, 0.9898214418809326842, 1.000000000000000000, 0.9898214418809326842, 1.000000000000000000, 0.9898214418809326842, 1.000000000000000000, 0.9898214418809326842, 1.000000000000000000, 0.9898214418809326842, 1.000000000000000000, 0.9898214418809326842, 1.000000000000000000, 0.9898214418809326842, 1.000000000000000000, 0.9898214418809326842, 1.000000000000000000, 0.9898214418809326842, 1.000000000000000000, 0.9898214418809326842, 1.000000000000000000, 0.9898214418809326842, 1.000000000000000000, 0.9898214418809326842, 1.000000000000000000, 0.9898214418809326842, 1.000000000000000000, 0.9898214418809326842, 1.000000000000000000, 0.9898214418809326842, 1.000000000000000000, 0.9898214418809326842, 1.000000000000000000, 0.9898214418809326842, 1.000000000000000000, 0.9898214418809326842, 1.000000000000000000, 0.9898214418809326842, 1.000000000000000000, 0.9898214418809326842, 1.000000000000000000, 0.9898214418809326842, 1.000000000000000000, 0.9898214418809326842, 1.000000000000000000, 0.9898214418809326842, 1.000000000000000000, 0.9898214418809326842, 1.000000000000000000, 0.9898214418809326842, 1.000000000000000000, 0.9898214418809326842, 1.000000000000000000, 0.9898214418809326842, 1.000000000000000000, 0.9898214418809326842, 1.000000000000000000, 0.9898214418809326842, 1.000000000000000000, 0.9898214418809326842, 1.000000000000000000, 0.9898214418809326842, 1.000000000000000000, 0.9898214418809326842, 1.000000000000000000, 0.9898214418809326842, 1.000000000000000000, 0.9898214418809326842, 1.000000000000000000, 0.9898214418809326842, 1.000000000000000000, 0.9898214418809326842, 1.000000000000000000, 0.9898214418809326842, 1.000000000000000000, 0.9898214418809326842, 1.000000000000000000, 0.9898214418809326842, 1.000000000000000000, 0.9898214418809326842, 1.000000000000000000, 0.9898214418809326842, 1.000000000000000000, 0.9898214418809326842, 1.000000000000000000, 0.9898214418809326842, 1.000000000000000000, 0.9898214418809326842, 1.000000000000000000, 0.9898214418809326842, 1.000000000000000000, 0.9898214418809326842, 1.000000000000000000, 0.9898214418809326842, 1.000000000000000000, 0.9898214418809326842, 1.000000000000000000, 0.9898214418809326842, 1.000000000000000000, 0.9898214418809326842, 1.000000000000000000, 0.9898214418809326842, 1.000000000000000000, 0.9898214418809326842, 1.000000000000000000, 0.9898214418809326842, 1.000000000000000000, 0.9898214418809326842, 1.000000000000000000, 0.9898214418809326842, 1.000000000000000000, 0.9898214418809326842, 1.000000000000000000, 0.9898214418809326842, 1.000000000000000000, 0.9898214418809326842, 1.000000000000000000, 0.9898214418809326842, 1.000000000000000000, 0.9898214418809326842, 1.000000000000000000, 0.9898214418809326842, 1.000000000000000000, 0.9898214418809326842, 1.000000000000000000, 0.9898214418809326842, 1.000000000000000000, 0.9898214418809326842, 1.000000000000000000, 0.9898214418809326842, 1.000000000000000000, 0.9898214418809326842, 1.000000000000000000, 0.9898214418809326842, 1.000000000000000000, 0.9898214418809326842, 1.000000000000000000, 0.9898214418809326842, 1.000000000000000000, 0.9898214418809326842, 1.000000000000000000, 0.9898214418809326842, 1.000000000000000000, 0.9898214418809326842, 1.000000000000000000, 0.9898214418809326842, 1.000000000000000000, 0.9898214418809326842, 1.000000000000000000, 0.9898214418809326842, 1.000000000000000000, 0.9898214418809326842, 1.000000000000000000, 0.9898214418809326842, 1.000000000000000000, 0.9898214418809326842, 1.000000000000000000, 0.9898214418809326842, 1.000000000000000000, 0.9898214418809326842, 1.000000000000000000, 0.9898214418809326842, 1.000000000000000000, 0.9898214418809326842, 1.000000000000000000, 0.9898214418809326842, 1.000000000000000000, 0.9898214418809326842, 1.000000000000000000, 0.9898214418809326842, 1.000000000000000000, 0.9898214418809326842, 1.000000000000000000, 0.9898214418809326842, 1.000000000000000000, 0.9898214418809326842, 1.000000000000000000, 0.9898214418809326842, 1.000000000000000000, 0.9898214418809326842, 1.000000000000000000, 0.9898214418809326842, 1.000000000000000000, 0.9898214418809326842, 1.000000000000000000, 0.9898214418809326842, 1.000000000000000000, 0.9898214418809326842, 1.000000000000000000, 0.9898214418809326842, 1.000000000000000000, 0.9898214418809326842, 1.000000000000000000, 0.9898214418809326842, 1.000000000000000000, 0.9898214418809326842, 1.000000000000000000, 0.9898214418809326842, 1.000000000000000000, 0.9898214418809326842, 1.000000000000000000, 0.9898214418809326842, 1.000000000000000000, 0.9898214418809326842, 1.000000000000000000, 0.9898214418809326842, 1.000000000000000000, 0.9898214418809326842, 1.000000000000000000, 0.9898214418809326842, 1.000000000000000000, 0.9961809353924466759, 0.9952277490961531914),
 ( 0.3333333333333333703, 0.3299404806269776169, 0.3333333333333333703, 0.3299404806269776169, 0.3333333333333333703, 0.3299404806269776169, 0.3333333333333333703, 0.3299404806269776169, 0.3333333333333333703, 0.3299404806269776169, 0.3333333333333333703, 0.3299404806269776169, 0.3333333333333333703, 0.3299404806269776169, 0.3333333333333333703, 0.3299404806269776169, 0.3333333333333333703, 0.3299404806269776169, 0.3333333333333333703, 0.3299404806269776169, 0.3333333333333333703, 0.3299404806269776169, 0.3333333333333333703, 0.3299404806269776169, 0.3333333333333333703, 0.3299404806269776169, 0.3333333333333333703, 0.3299404806269776169, 0.3333333333333333703, 0.3299404806269776169, 0.3333333333333333703, 0.3299404806269776169, 0.3333333333333333703, 0.3299404806269776169, 0.3333333333333333703, 0.3299404806269776169, 0.3333333333333333703, 0.3299404806269776169, 0.3333333333333333703, 0.3299404806269776169, 0.3333333333333333703, 0.3299404806269776169, 0.3333333333333333703, 0.3299404806269776169, 0.3333333333333333703, 0.3299404806269776169, 0.3333333333333333703, 0.3299404806269776169, 0.3333333333333333703, 0.3299404806269776169, 0.3333333333333333703, 0.3299404806269776169, 0.3333333333333333703, 0.3299404806269776169, 0.3333333333333333703, 0.3299404806269776169, 0.3333333333333333703, 0.3299404806269776169, 0.3333333333333333703, 0.3299404806269776169, 0.3333333333333333703, 0.3299404806269776169, 0.3333333333333333703, 0.3299404806269776169, 0.3333333333333333703, 0.3299404806269776169, 0.3333333333333333703, 0.3299404806269776169, 0.3333333333333333703, 0.3299404806269776169, 0.3333333333333333703, 0.3299404806269776169, 0.3333333333333333703, 0.3299404806269776169, 0.3333333333333333703, 0.3299404806269776169, 0.3333333333333333703, 0.3299404806269776169, 0.3333333333333333703, 0.3299404806269776169, 0.3333333333333333703, 0.3299404806269776169, 0.3333333333333333703, 0.3299404806269776169, 0.3333333333333333703, 0.3299404806269776169, 0.3333333333333333703, 0.3299404806269776169, 0.3333333333333333703, 0.3299404806269776169, 0.3333333333333333703, 0.3299404806269776169, 0.3333333333333333703, 0.3299404806269776169, 0.3333333333333333703, 0.3299404806269776169, 0.3333333333333333703, 0.3299404806269776169, 0.3333333333333333703, 0.3299404806269776169, 0.3333333333333333703, 0.3299404806269776169, 0.3333333333333333703, 0.3299404806269776169, 0.3333333333333333703, 0.3299404806269776169, 0.3333333333333333703, 0.3299404806269776169, 0.3333333333333333703, 0.3299404806269776169, 0.3333333333333333703, 0.3299404806269776169, 0.3333333333333333703, 0.3299404806269776169, 0.3333333333333333703, 0.3299404806269776169, 0.3333333333333333703, 0.3299404806269776169, 0.3333333333333333703, 0.3299404806269776169, 0.3333333333333333703, 0.3299404806269776169, 0.3333333333333333703, 0.3299404806269776169, 0.3333333333333333703, 0.3299404806269776169, 0.3333333333333333703, 0.3299404806269776169, 0.3333333333333333703, 0.3299404806269776169, 0.3333333333333333703, 0.3299404806269776169, 0.3333333333333333703, 0.3299404806269776169, 0.3333333333333333703, 0.3299404806269776169, 0.3333333333333333703, 0.3299404806269776169, 0.3333333333333333703, 0.3299404806269776169, 0.3333333333333333703, 0.3299404806269776169, 0.3333333333333333703, 0.3299404806269776169, 0.3333333333333333703, 0.3299404806269776169, 0.3333333333333333703, 0.3299404806269776169, 0.3333333333333333703, 0.3299404806269776169, 0.3333333333333333703, 0.3299404806269776169, 0.3333333333333333703, 0.3299404806269776169, 0.3333333333333333703, 0.3299404806269776169, 0.3333333333333333703, 0.3299404806269776169, 0.3333333333333333703, 0.3299404806269776169, 0.3333333333333333703, 0.3299404806269776169, 0.3333333333333333703, 0.3299404806269776169, 0.3333333333333333703, 0.3299404806269776169, 0.3333333333333333703, 0.3299404806269776169, 0.3333333333333333703, 0.3299404806269776169, 0.3333333333333333703, 0.3299404806269776169, 0.3333333333333333703, 0.3299404806269776169, 0.3333333333333333703, 0.3299404806269776169, 0.3333333333333333703, 0.3299404806269776169, 0.3333333333333333703, 0.3299404806269776169, 0.3333333333333333703, 0.3299404806269776169, 0.3333333333333333703, 0.3299404806269776169, 0.3333333333333333703, 0.3299404806269776169, 0.3333333333333333703, 0.3299404806269776169, 0.3333333333333333703, 0.3299404806269776169, 0.3333333333333333703, 0.3299404806269776169, 0.3333333333333333703, 0.3299404806269776169, 0.3333333333333333703, 0.3299404806269776169, 0.3333333333333333703, 0.3299404806269776169, 0.3333333333333333703, 0.3299404806269776169, 0.3333333333333333703, 0.3299404806269776169, 0.3333333333333333703, 0.3299404806269776169, 0.3333333333333333703, 0.3299404806269776169, 0.3333333333333333703, 0.3299404806269776169, 0.3333333333333333703, 0.3299404806269776169, 0.3333333333333333703, 0.3299404806269776169, 0.3333333333333333703, 0.3299404806269776169, 0.3333333333333333703, 0.3299404806269776169, 0.3333333333333333703, 0.3299404806269776169, 0.3333333333333333703, 0.3299404806269776169, 0.3333333333333333703, 0.3299404806269776169, 0.3333333333333333703, 0.3299404806269776169, 0.3333333333333333703, 0.3299404806269776169, 0.3333333333333333703, 0.3299404806269776169, 0.3333333333333333703, 0.3299404806269776169, 0.3333333333333333703, 0.3299404806269776169, 0.3333333333333333703, 0.3299404806269776169, 0.3333333333333333703, 0.3299404806269776169, 0.3333333333333333703, 0.3299404806269776169, 0.3333333333333333703, 0.3299404806269776169, 0.3333333333333333703, 0.3299404806269776169, 0.3333333333333333703, 0.3299404806269776169, 0.3333333333333333703, 0.3299404806269776169, 0.3333333333333333703, 0.3299404806269776169, 0.3333333333333333703, 0.3299404806269776169, 0.3333333333333333703, 0.3299404806269776169, 0.3333333333333333703, 0.3299404806269776169, 0.3333333333333333703, 0.3299404806269776169, 0.3333333333333333703, 0.3299404806269776169, 0.3333333333333333703, 0.3299404806269776169, 0.3333333333333333703, 0.3299404806269776169, 0.3333333333333333703, 0.3299404806269776169, 0.3333333333333333703, 0.3299404806269776169, 0.3333333333333333703, 0.3299404806269776169, 0.3333333333333333703, 0.3299404806269776169, 0.3333333333333333703, 0.3299404806269776169, 0.3333333333333333703, 0.3299404806269776169, 0.3333333333333333703, 0.3299404806269776169, 0.3333333333333333703, 0.3299404806269776169, 0.3333333333333333703, 0.3299404806269776169, 0.3333333333333333703, 0.3299404806269776169, 0.3333333333333333703, 0.3299404806269776169, 0.3333333333333333703, 0.3299404806269776169, 0.3333333333333333703, 0.3299404806269776169, 0.3333333333333333703, 0.3299404806269776169, 0.3333333333333333703, 0.3299404806269776169, 0.3333333333333333703, 0.3299404806269776169, 0.3333333333333333703, 0.3299404806269776169, 0.3333333333333333703, 0.3299404806269776169, 0.3333333333333333703, 0.3299404806269776169, 0.3333333333333333703, 0.3299404806269776169, 0.3333333333333333703, 0.3299404806269776169, 0.3333333333333333703, 0.3299404806269776169, 0.3333333333333333703, 0.3299404806269776169, 0.3333333333333333703, 0.3299404806269776169, 0.3333333333333333703, 0.3299404806269776169, 0.3333333333333333703, 0.3299404806269776169, 0.3333333333333333703, 0.3299404806269776169, 0.3333333333333333703, 0.3299404806269776169, 0.3333333333333333703, 0.3299404806269776169, 0.3333333333333333703, 0.3299404806269776169, 0.3333333333333333703, 0.3299404806269776169, 0.3333333333333333703, 0.3299404806269776169, 0.3333333333333333703, 0.3299404806269776169, 0.3333333333333333703, 0.3299404806269776169, 0.3333333333333333703, 0.3299404806269776169, 0.3333333333333333703, 0.3299404806269776169, 0.3333333333333333703, 0.3299404806269776169, 0.3333333333333333703, 0.3299404806269776169, 0.3333333333333333703, 0.3299404806269776169, 0.3333333333333333703, 0.3299404806269776169, 0.3333333333333333703, 0.3299404806269776169, 0.3333333333333333703, 0.3299404806269776169, 0.3333333333333333703, 0.3299404806269776169, 0.3333333333333333703, 0.3299404806269776169, 0.3333333333333333703, 0.3299404806269776169, 0.3333333333333333703, 0.3299404806269776169, 0.3333333333333333703, 0.3299404806269776169, 0.3333333333333333703, 0.3299404806269776169, 0.3333333333333333703, 0.3299404806269776169, 0.3333333333333333703, 0.3299404806269776169, 0.3333333333333333703, 0.3299404806269776169, 0.3333333333333333703, 0.3299404806269776169, 0.3333333333333333703, 0.3299404806269776169, 0.3333333333333333703, 0.3299404806269776169, 0.3333333333333333703, 0.3299404806269776169, 0.3333333333333333703, 0.3299404806269776169, 0.3333333333333333703, 0.3299404806269776169, 0.3333333333333333703, 0.3299404806269776169, 0.3333333333333333703, 0.3299404806269776169, 0.3333333333333333703, 0.3299404806269776169, 0.3333333333333333703, 0.3299404806269776169, 0.3333333333333333703, 0.3299404806269776169, 0.3333333333333333703, 0.3299404806269776169, 0.3333333333333333703, 0.3299404806269776169, 0.3333333333333333703, 0.3299404806269776169, 0.3333333333333333703, 0.3299404806269776169, 0.3333333333333333703, 0.3299404806269776169, 0.3333333333333333703, 0.3299404806269776169, 0.3333333333333333703, 0.3299404806269776169, 0.3333333333333333703, 0.3299404806269776169, 0.3333333333333333703, 0.3299404806269776169, 0.3333333333333333703, 0.3299404806269776169, 0.3333333333333333703, 0.3299404806269776169, 0.3333333333333333703, 0.3299404806269776169, 0.3333333333333333703, 0.3299404806269776169, 0.3333333333333333703, 0.3299404806269776169, 0.3333333333333333703, 0.3299404806269776169, 0.3333333333333333703, 0.3299404806269776169, 0.3333333333333333703, 0.3299404806269776169, 0.3333333333333333703, 0.3299404806269776169, 0.3333333333333333703, 0.3299404806269776169, 0.3333333333333333703, 0.3299404806269776169, 0.3333333333333333703, 0.3299404806269776169, 0.3333333333333333703, 0.3299404806269776169, 0.3333333333333333703, 0.3299404806269776169, 0.3333333333333333703, 0.3299404806269776169, 0.3333333333333333703, 0.3299404806269776169, 0.3333333333333333703, 0.3299404806269776169, 0.3333333333333333703, 0.3299404806269776169, 0.3333333333333333703, 0.3299404806269776169, 0.3333333333333333703, 0.3299404806269776169, 0.3333333333333333703, 0.3299404806269776169, 0.3333333333333333703, 0.3299404806269776169, 0.3333333333333333703, 0.3299404806269776169, 0.3333333333333333703, 0.3299404806269776169, 0.3333333333333333703, 0.3299404806269776169, 0.3333333333333333703, 0.3299404806269776169, 0.3333333333333333703, 0.3299404806269776169, 0.3333333333333333703, 0.3299404806269776169, 0.3333333333333333703, 0.3299404806269776169, 0.3333333333333333703, 0.3299404806269776169, 0.3333333333333333703, 0.3299404806269776169, 0.3333333333333333703, 0.3299404806269776169, 0.3333333333333333703, 0.3299404806269776169, 0.3333333333333333703, 0.3299404806269776169, 0.3333333333333333703, 0.3299404806269776169, 0.3333333333333333703, 0.3299404806269776169, 0.3333333333333333703, 0.3299404806269776169, 0.3333333333333333703, 0.3299404806269776169, 0.3333333333333333703, 0.3299404806269776169, 0.3333333333333333703, 0.3299404806269776169, 0.3333333333333333703, 0.3299404806269776169, 0.3333333333333333703, 0.3299404806269776169, 0.3333333333333333703, 0.3299404806269776169, 0.3333333333333333703, 0.3299404806269776169, 0.3333333333333333703, 0.3299404806269776169, 0.3333333333333333703, 0.3299404806269776169, 0.3333333333333333703, 0.3299404806269776169, 0.3333333333333333703, 0.3299404806269776169, 0.3333333333333333703, 0.3299404806269776169, 0.3333333333333333703, 0.3299404806269776169, 0.3333333333333333703, 0.3299404806269776169, 0.3333333333333333703, 0.3299404806269776169, 0.3333333333333333703, 0.3299404806269776169, 0.3333333333333333703, 0.3299404806269776169, 0.3333333333333333703, 0.3299404806269776169, 0.3333333333333333703, 0.3299404806269776169, 0.3333333333333333703, 0.3299404806269776169, 0.3333333333333333703, 0.3299404806269776169, 0.3333333333333333703, 0.3299404806269776169, 0.3333333333333333703, 0.3299404806269776169, 0.3333333333333333703, 0.3299404806269776169, 0.3333333333333333703, 0.3299404806269776169, 0.3333333333333333703, 0.3299404806269776169, 0.3333333333333333703, 0.3299404806269776169, 0.3333333333333333703, 0.3299404806269776169, 0.3333333333333333703, 0.3299404806269776169, 0.3333333333333333703, 0.3299404806269776169, 0.3333333333333333703, 0.3299404806269776169, 0.3333333333333333703, 0.3299404806269776169, 0.3333333333333333703, 0.3299404806269776169, 0.3333333333333333703, 0.3299404806269776169, 0.3333333333333333703, 0.3299404806269776169, 0.3333333333333333703, 0.3299404806269776169, 0.3333333333333333703, 0.3299404806269776169, 0.3333333333333333703, 0.3299404806269776169, 0.3333333333333333703, 0.3299404806269776169, 0.3333333333333333703, 0.3299404806269776169, 0.3333333333333333703, 0.3299404806269776169, 0.3333333333333333703, 0.3299404806269776169, 0.3333333333333333703, 0.3299404806269776169, 0.3333333333333333703, 0.3299404806269776169, 0.3333333333333333703, 0.3299404806269776169, 0.3333333333333333703, 0.3299404806269776169, 0.3333333333333333703, 0.3299404806269776169, 0.3333333333333333703, 0.3299404806269776169, 0.3333333333333333703, 0.3299404806269776169, 0.3333333333333333703, 0.3299404806269776169, 0.3333333333333333703, 0.3299404806269776169, 0.3333333333333333703, 0.3299404806269776169, 0.3333333333333333703, 0.3299404806269776169, 0.3333333333333333703, 0.3299404806269776169, 0.3333333333333333703, 0.3299404806269776169, 0.3333333333333333703, 0.3299404806269776169, 0.3333333333333333703, 0.3299404806269776169, 0.3333333333333333703, 0.3299404806269776169, 0.3333333333333333703, 0.3299404806269776169, 0.3333333333333333703, 0.3299404806269776169, 0.3333333333333333703, 0.3299404806269776169, 0.3333333333333333703, 0.3299404806269776169, 0.3333333333333333703, 0.3299404806269776169, 0.3333333333333333703, 0.3299404806269776169, 0.3333333333333333703, 0.3299404806269776169, 0.3333333333333333703, 0.3299404806269776169, 0.3333333333333333703, 0.3299404806269776169, 0.3333333333333333703, 0.3299404806269776169, 0.3333333333333333703, 0.3299404806269776169, 0.3333333333333333703, 0.3299404806269776169, 0.3333333333333333703, 0.3299404806269776169, 0.3333333333333333703, 0.3299404806269776169, 0.3333333333333333703, 0.3299404806269776169, 0.3333333333333333703, 0.3299404806269776169, 0.3333333333333333703, 0.3299404806269776169, 0.3333333333333333703, 0.3299404806269776169, 0.3333333333333333703, 0.3299404806269776169, 0.3333333333333333703, 0.3299404806269776169, 0.3333333333333333703, 0.3299404806269776169, 0.3333333333333333703, 0.3299404806269776169, 0.3333333333333333703, 0.3299404806269776169, 0.3333333333333333703, 0.3299404806269776169, 0.3333333333333333703, 0.3299404806269776169, 0.3333333333333333703, 0.3299404806269776169, 0.3333333333333333703, 0.3299404806269776169, 0.3333333333333333703, 0.3299404806269776169, 0.3333333333333333703, 0.3299404806269776169, 0.3333333333333333703, 0.3299404806269776169, 0.3333333333333333703, 0.3299404806269776169, 0.3333333333333333703, 0.3299404806269776169, 0.3333333333333333703, 0.3299404806269776169, 0.3333333333333333703, 0.3299404806269776169, 0.3333333333333333703, 0.3299404806269776169, 0.3333333333333333703, 0.3299404806269776169, 0.3333333333333333703, 0.3299404806269776169, 0.3333333333333333703, 0.3299404806269776169, 0.3333333333333333703, 0.3299404806269776169, 0.3333333333333333703, 0.3299404806269776169, 0.3333333333333333703, 0.3299404806269776169, 0.3333333333333333703, 0.3299404806269776169, 0.3333333333333333703, 0.3299404806269776169, 0.3333333333333333703, 0.3299404806269776169, 0.3333333333333333703, 0.3299404806269776169, 0.3333333333333333703, 0.3299404806269776169, 0.3333333333333333703, 0.3299404806269776169, 0.3333333333333333703, 0.3299404806269776169, 0.3333333333333333703, 0.3299404806269776169, 0.3333333333333333703, 0.3299404806269776169, 0.3333333333333333703, 0.3299404806269776169, 0.3333333333333333703, 0.3299404806269776169, 0.3333333333333333703, 0.3299404806269776169, 0.3333333333333333703, 0.3299404806269776169, 0.3333333333333333703, 0.3299404806269776169, 0.3333333333333333703, 0.3299404806269776169, 0.3333333333333333703, 0.3299404806269776169, 0.3333333333333333703, 0.3299404806269776169, 0.3333333333333333703, 0.3299404806269776169, 0.3333333333333333703, 0.3299404806269776169, 0.3333333333333333703, 0.3299404806269776169, 0.3333333333333333703, 0.3299404806269776169, 0.3333333333333333703, 0.3299404806269776169, 0.3333333333333333703, 0.3299404806269776169, 0.3333333333333333703, 0.3299404806269776169, 0.3333333333333333703, 0.3299404806269776169, 0.3333333333333333703, 0.3299404806269776169, 0.3333333333333333703, 0.3299404806269776169, 0.3333333333333333703, 0.3299404806269776169, 0.3333333333333333703, 0.3299404806269776169, 0.3333333333333333703, 0.3299404806269776169, 0.3333333333333333703, 0.3299404806269776169, 0.3333333333333333703, 0.3299404806269776169, 0.3333333333333333703, 0.3299404806269776169, 0.3333333333333333703, 0.3299404806269776169, 0.3333333333333333703, 0.3299404806269776169, 0.3333333333333333703, 0.3299404806269776169, 0.3333333333333333703, 0.3299404806269776169, 0.3333333333333333703, 0.3299404806269776169, 0.3333333333333333703, 0.3299404806269776169, 0.3333333333333333703, 0.3299404806269776169, 0.3333333333333333703, 0.3299404806269776169, 0.3333333333333333703, 0.3299404806269776169, 0.3333333333333333703, 0.3299404806269776169, 0.3333333333333333703, 0.3299404806269776169, 0.3333333333333333703, 0.3299404806269776169, 0.3333333333333333703, 0.3299404806269776169, 0.3333333333333333703, 0.3299404806269776169, 0.3333333333333333703, 0.3299404806269776169, 0.3333333333333333703, 0.3299404806269776169, 0.3333333333333333703, 0.3299404806269776169, 0.3333333333333333703, 0.3299404806269776169, 0.3333333333333333703, 0.3299404806269776169, 0.3333333333333333703, 0.3299404806269776169, 0.3333333333333333703, 0.3299404806269776169, 0.3333333333333333703, 0.3299404806269776169, 0.3333333333333333703, 0.3299404806269776169, 0.3333333333333333703, 0.3299404806269776169, 0.3333333333333333703, 0.3299404806269776169, 0.3333333333333333703, 0.3299404806269776169, 0.3333333333333333703, 0.3299404806269776169, 0.3333333333333333703, 0.3299404806269776169, 0.3333333333333333703, 0.3299404806269776169, 0.3333333333333333703, 0.3299404806269776169, 0.3333333333333333703, 0.3299404806269776169, 0.3333333333333333703, 0.3299404806269776169, 0.3333333333333333703, 0.3299404806269776169, 0.3333333333333333703, 0.3299404806269776169, 0.3333333333333333703, 0.3299404806269776169, 0.3333333333333333703, 0.3299404806269776169, 0.3333333333333333703, 0.3299404806269776169, 0.3333333333333333703, 0.3299404806269776169, 0.3333333333333333703, 0.3299404806269776169, 0.3333333333333333703, 0.3299404806269776169, 0.3333333333333333703, 0.3299404806269776169, 0.3333333333333333703, 0.3299404806269776169, 0.3333333333333333703, 0.3299404806269776169, 0.3333333333333333703, 0.3299404806269776169, 0.3333333333333333703, 0.3299404806269776169, 0.3333333333333333703, 0.3299404806269776169, 0.3333333333333333703, 0.3299404806269776169, 0.3333333333333333703, 0.3299404806269776169, 0.3333333333333333703, 0.3299404806269776169, 0.3333333333333333703, 0.3299404806269776169, 0.3333333333333333703, 0.3299404806269776169, 0.3333333333333333703, 0.3299404806269776169, 0.3333333333333333703, 0.3299404806269776169, 0.3333333333333333703, 0.3299404806269776169, 0.3333333333333333703, 0.3299404806269776169, 0.3333333333333333703, 0.3299404806269776169, 0.3333333333333333703, 0.3299404806269776169, 0.3333333333333333703, 0.3299404806269776169, 0.3333333333333333703, 0.3299404806269776169, 0.3333333333333333703, 0.3320603117974822438, 0.3317425830320511193),
 ( 0.3333333333333333703, 0.3299404806269776169, 0.3333333333333333703, 0.3299404806269776169, 0.3333333333333333703, 0.3299404806269776169, 0.3333333333333333703, 0.3299404806269776169, 0.3333333333333333703, 0.3299404806269776169, 0.3333333333333333703, 0.3299404806269776169, 0.3333333333333333703, 0.3299404806269776169, 0.3333333333333333703, 0.3299404806269776169, 0.3333333333333333703, 0.3299404806269776169, 0.3333333333333333703, 0.3299404806269776169, 0.3333333333333333703, 0.3299404806269776169, 0.3333333333333333703, 0.3299404806269776169, 0.3333333333333333703, 0.3299404806269776169, 0.3333333333333333703, 0.3299404806269776169, 0.3333333333333333703, 0.3299404806269776169, 0.3333333333333333703, 0.3299404806269776169, 0.3333333333333333703, 0.3299404806269776169, 0.3333333333333333703, 0.3299404806269776169, 0.3333333333333333703, 0.3299404806269776169, 0.3333333333333333703, 0.3299404806269776169, 0.3333333333333333703, 0.3299404806269776169, 0.3333333333333333703, 0.3299404806269776169, 0.3333333333333333703, 0.3299404806269776169, 0.3333333333333333703, 0.3299404806269776169, 0.3333333333333333703, 0.3299404806269776169, 0.3333333333333333703, 0.3299404806269776169, 0.3333333333333333703, 0.3299404806269776169, 0.3333333333333333703, 0.3299404806269776169, 0.3333333333333333703, 0.3299404806269776169, 0.3333333333333333703, 0.3299404806269776169, 0.3333333333333333703, 0.3299404806269776169, 0.3333333333333333703, 0.3299404806269776169, 0.3333333333333333703, 0.3299404806269776169, 0.3333333333333333703, 0.3299404806269776169, 0.3333333333333333703, 0.3299404806269776169, 0.3333333333333333703, 0.3299404806269776169, 0.3333333333333333703, 0.3299404806269776169, 0.3333333333333333703, 0.3299404806269776169, 0.3333333333333333703, 0.3299404806269776169, 0.3333333333333333703, 0.3299404806269776169, 0.3333333333333333703, 0.3299404806269776169, 0.3333333333333333703, 0.3299404806269776169, 0.3333333333333333703, 0.3299404806269776169, 0.3333333333333333703, 0.3299404806269776169, 0.3333333333333333703, 0.3299404806269776169, 0.3333333333333333703, 0.3299404806269776169, 0.3333333333333333703, 0.3299404806269776169, 0.3333333333333333703, 0.3299404806269776169, 0.3333333333333333703, 0.3299404806269776169, 0.3333333333333333703, 0.3299404806269776169, 0.3333333333333333703, 0.3299404806269776169, 0.3333333333333333703, 0.3299404806269776169, 0.3333333333333333703, 0.3299404806269776169, 0.3333333333333333703, 0.3299404806269776169, 0.3333333333333333703, 0.3299404806269776169, 0.3333333333333333703, 0.3299404806269776169, 0.3333333333333333703, 0.3299404806269776169, 0.3333333333333333703, 0.3299404806269776169, 0.3333333333333333703, 0.3299404806269776169, 0.3333333333333333703, 0.3299404806269776169, 0.3333333333333333703, 0.3299404806269776169, 0.3333333333333333703, 0.3299404806269776169, 0.3333333333333333703, 0.3299404806269776169, 0.3333333333333333703, 0.3299404806269776169, 0.3333333333333333703, 0.3299404806269776169, 0.3333333333333333703, 0.3299404806269776169, 0.3333333333333333703, 0.3299404806269776169, 0.3333333333333333703, 0.3299404806269776169, 0.3333333333333333703, 0.3299404806269776169, 0.3333333333333333703, 0.3299404806269776169, 0.3333333333333333703, 0.3299404806269776169, 0.3333333333333333703, 0.3299404806269776169, 0.3333333333333333703, 0.3299404806269776169, 0.3333333333333333703, 0.3299404806269776169, 0.3333333333333333703, 0.3299404806269776169, 0.3333333333333333703, 0.3299404806269776169, 0.3333333333333333703, 0.3299404806269776169, 0.3333333333333333703, 0.3299404806269776169, 0.3333333333333333703, 0.3299404806269776169, 0.3333333333333333703, 0.3299404806269776169, 0.3333333333333333703, 0.3299404806269776169, 0.3333333333333333703, 0.3299404806269776169, 0.3333333333333333703, 0.3299404806269776169, 0.3333333333333333703, 0.3299404806269776169, 0.3333333333333333703, 0.3299404806269776169, 0.3333333333333333703, 0.3299404806269776169, 0.3333333333333333703, 0.3299404806269776169, 0.3333333333333333703, 0.3299404806269776169, 0.3333333333333333703, 0.3299404806269776169, 0.3333333333333333703, 0.3299404806269776169, 0.3333333333333333703, 0.3299404806269776169, 0.3333333333333333703, 0.3299404806269776169, 0.3333333333333333703, 0.3299404806269776169, 0.3333333333333333703, 0.3299404806269776169, 0.3333333333333333703, 0.3299404806269776169, 0.3333333333333333703, 0.3299404806269776169, 0.3333333333333333703, 0.3299404806269776169, 0.3333333333333333703, 0.3299404806269776169, 0.3333333333333333703, 0.3299404806269776169, 0.3333333333333333703, 0.3299404806269776169, 0.3333333333333333703, 0.3299404806269776169, 0.3333333333333333703, 0.3299404806269776169, 0.3333333333333333703, 0.3299404806269776169, 0.3333333333333333703, 0.3299404806269776169, 0.3333333333333333703, 0.3299404806269776169, 0.3333333333333333703, 0.3299404806269776169, 0.3333333333333333703, 0.3299404806269776169, 0.3333333333333333703, 0.3299404806269776169, 0.3333333333333333703, 0.3299404806269776169, 0.3333333333333333703, 0.3299404806269776169, 0.3333333333333333703, 0.3299404806269776169, 0.3333333333333333703, 0.3299404806269776169, 0.3333333333333333703, 0.3299404806269776169, 0.3333333333333333703, 0.3299404806269776169, 0.3333333333333333703, 0.3299404806269776169, 0.3333333333333333703, 0.3299404806269776169, 0.3333333333333333703, 0.3299404806269776169, 0.3333333333333333703, 0.3299404806269776169, 0.3333333333333333703, 0.3299404806269776169, 0.3333333333333333703, 0.3299404806269776169, 0.3333333333333333703, 0.3299404806269776169, 0.3333333333333333703, 0.3299404806269776169, 0.3333333333333333703, 0.3299404806269776169, 0.3333333333333333703, 0.3299404806269776169, 0.3333333333333333703, 0.3299404806269776169, 0.3333333333333333703, 0.3299404806269776169, 0.3333333333333333703, 0.3299404806269776169, 0.3333333333333333703, 0.3299404806269776169, 0.3333333333333333703, 0.3299404806269776169, 0.3333333333333333703, 0.3299404806269776169, 0.3333333333333333703, 0.3299404806269776169, 0.3333333333333333703, 0.3299404806269776169, 0.3333333333333333703, 0.3299404806269776169, 0.3333333333333333703, 0.3299404806269776169, 0.3333333333333333703, 0.3299404806269776169, 0.3333333333333333703, 0.3299404806269776169, 0.3333333333333333703, 0.3299404806269776169, 0.3333333333333333703, 0.3299404806269776169, 0.3333333333333333703, 0.3299404806269776169, 0.3333333333333333703, 0.3299404806269776169, 0.3333333333333333703, 0.3299404806269776169, 0.3333333333333333703, 0.3299404806269776169, 0.3333333333333333703, 0.3299404806269776169, 0.3333333333333333703, 0.3299404806269776169, 0.3333333333333333703, 0.3299404806269776169, 0.3333333333333333703, 0.3299404806269776169, 0.3333333333333333703, 0.3299404806269776169, 0.3333333333333333703, 0.3299404806269776169, 0.3333333333333333703, 0.3299404806269776169, 0.3333333333333333703, 0.3299404806269776169, 0.3333333333333333703, 0.3299404806269776169, 0.3333333333333333703, 0.3299404806269776169, 0.3333333333333333703, 0.3299404806269776169, 0.3333333333333333703, 0.3299404806269776169, 0.3333333333333333703, 0.3299404806269776169, 0.3333333333333333703, 0.3299404806269776169, 0.3333333333333333703, 0.3299404806269776169, 0.3333333333333333703, 0.3299404806269776169, 0.3333333333333333703, 0.3299404806269776169, 0.3333333333333333703, 0.3299404806269776169, 0.3333333333333333703, 0.3299404806269776169, 0.3333333333333333703, 0.3299404806269776169, 0.3333333333333333703, 0.3299404806269776169, 0.3333333333333333703, 0.3299404806269776169, 0.3333333333333333703, 0.3299404806269776169, 0.3333333333333333703, 0.3299404806269776169, 0.3333333333333333703, 0.3299404806269776169, 0.3333333333333333703, 0.3299404806269776169, 0.3333333333333333703, 0.3299404806269776169, 0.3333333333333333703, 0.3299404806269776169, 0.3333333333333333703, 0.3299404806269776169, 0.3333333333333333703, 0.3299404806269776169, 0.3333333333333333703, 0.3299404806269776169, 0.3333333333333333703, 0.3299404806269776169, 0.3333333333333333703, 0.3299404806269776169, 0.3333333333333333703, 0.3299404806269776169, 0.3333333333333333703, 0.3299404806269776169, 0.3333333333333333703, 0.3299404806269776169, 0.3333333333333333703, 0.3299404806269776169, 0.3333333333333333703, 0.3299404806269776169, 0.3333333333333333703, 0.3299404806269776169, 0.3333333333333333703, 0.3299404806269776169, 0.3333333333333333703, 0.3299404806269776169, 0.3333333333333333703, 0.3299404806269776169, 0.3333333333333333703, 0.3299404806269776169, 0.3333333333333333703, 0.3299404806269776169, 0.3333333333333333703, 0.3299404806269776169, 0.3333333333333333703, 0.3299404806269776169, 0.3333333333333333703, 0.3299404806269776169, 0.3333333333333333703, 0.3299404806269776169, 0.3333333333333333703, 0.3299404806269776169, 0.3333333333333333703, 0.3299404806269776169, 0.3333333333333333703, 0.3299404806269776169, 0.3333333333333333703, 0.3299404806269776169, 0.3333333333333333703, 0.3299404806269776169, 0.3333333333333333703, 0.3299404806269776169, 0.3333333333333333703, 0.3299404806269776169, 0.3333333333333333703, 0.3299404806269776169, 0.3333333333333333703, 0.3299404806269776169, 0.3333333333333333703, 0.3299404806269776169, 0.3333333333333333703, 0.3299404806269776169, 0.3333333333333333703, 0.3299404806269776169, 0.3333333333333333703, 0.3299404806269776169, 0.3333333333333333703, 0.3299404806269776169, 0.3333333333333333703, 0.3299404806269776169, 0.3333333333333333703, 0.3299404806269776169, 0.3333333333333333703, 0.3299404806269776169, 0.3333333333333333703, 0.3299404806269776169, 0.3333333333333333703, 0.3299404806269776169, 0.3333333333333333703, 0.3299404806269776169, 0.3333333333333333703, 0.3299404806269776169, 0.3333333333333333703, 0.3299404806269776169, 0.3333333333333333703, 0.3299404806269776169, 0.3333333333333333703, 0.3299404806269776169, 0.3333333333333333703, 0.3299404806269776169, 0.3333333333333333703, 0.3299404806269776169, 0.3333333333333333703, 0.3299404806269776169, 0.3333333333333333703, 0.3299404806269776169, 0.3333333333333333703, 0.3299404806269776169, 0.3333333333333333703, 0.3299404806269776169, 0.3333333333333333703, 0.3299404806269776169, 0.3333333333333333703, 0.3299404806269776169, 0.3333333333333333703, 0.3299404806269776169, 0.3333333333333333703, 0.3299404806269776169, 0.3333333333333333703, 0.3299404806269776169, 0.3333333333333333703, 0.3299404806269776169, 0.3333333333333333703, 0.3299404806269776169, 0.3333333333333333703, 0.3299404806269776169, 0.3333333333333333703, 0.3299404806269776169, 0.3333333333333333703, 0.3299404806269776169, 0.3333333333333333703, 0.3299404806269776169, 0.3333333333333333703, 0.3299404806269776169, 0.3333333333333333703, 0.3299404806269776169, 0.3333333333333333703, 0.3299404806269776169, 0.3333333333333333703, 0.3299404806269776169, 0.3333333333333333703, 0.3299404806269776169, 0.3333333333333333703, 0.3299404806269776169, 0.3333333333333333703, 0.3299404806269776169, 0.3333333333333333703, 0.3299404806269776169, 0.3333333333333333703, 0.3299404806269776169, 0.3333333333333333703, 0.3299404806269776169, 0.3333333333333333703, 0.3299404806269776169, 0.3333333333333333703, 0.3299404806269776169, 0.3333333333333333703, 0.3299404806269776169, 0.3333333333333333703, 0.3299404806269776169, 0.3333333333333333703, 0.3299404806269776169, 0.3333333333333333703, 0.3299404806269776169, 0.3333333333333333703, 0.3299404806269776169, 0.3333333333333333703, 0.3299404806269776169, 0.3333333333333333703, 0.3299404806269776169, 0.3333333333333333703, 0.3299404806269776169, 0.3333333333333333703, 0.3299404806269776169, 0.3333333333333333703, 0.3299404806269776169, 0.3333333333333333703, 0.3299404806269776169, 0.3333333333333333703, 0.3299404806269776169, 0.3333333333333333703, 0.3299404806269776169, 0.3333333333333333703, 0.3299404806269776169, 0.3333333333333333703, 0.3299404806269776169, 0.3333333333333333703, 0.3299404806269776169, 0.3333333333333333703, 0.3299404806269776169, 0.3333333333333333703, 0.3299404806269776169, 0.3333333333333333703, 0.3299404806269776169, 0.3333333333333333703, 0.3299404806269776169, 0.3333333333333333703, 0.3299404806269776169, 0.3333333333333333703, 0.3299404806269776169, 0.3333333333333333703, 0.3299404806269776169, 0.3333333333333333703, 0.3299404806269776169, 0.3333333333333333703, 0.3299404806269776169, 0.3333333333333333703, 0.3299404806269776169, 0.3333333333333333703, 0.3299404806269776169, 0.3333333333333333703, 0.3299404806269776169, 0.3333333333333333703, 0.3299404806269776169, 0.3333333333333333703, 0.3299404806269776169, 0.3333333333333333703, 0.3299404806269776169, 0.3333333333333333703, 0.3299404806269776169, 0.3333333333333333703, 0.3299404806269776169, 0.3333333333333333703, 0.3299404806269776169, 0.3333333333333333703, 0.3299404806269776169, 0.3333333333333333703, 0.3299404806269776169, 0.3333333333333333703, 0.3299404806269776169, 0.3333333333333333703, 0.3299404806269776169, 0.3333333333333333703, 0.3299404806269776169, 0.3333333333333333703, 0.3299404806269776169, 0.3333333333333333703, 0.3299404806269776169, 0.3333333333333333703, 0.3299404806269776169, 0.3333333333333333703, 0.3299404806269776169, 0.3333333333333333703, 0.3299404806269776169, 0.3333333333333333703, 0.3299404806269776169, 0.3333333333333333703, 0.3299404806269776169, 0.3333333333333333703, 0.3299404806269776169, 0.3333333333333333703, 0.3299404806269776169, 0.3333333333333333703, 0.3299404806269776169, 0.3333333333333333703, 0.3299404806269776169, 0.3333333333333333703, 0.3299404806269776169, 0.3333333333333333703, 0.3299404806269776169, 0.3333333333333333703, 0.3299404806269776169, 0.3333333333333333703, 0.3299404806269776169, 0.3333333333333333703, 0.3299404806269776169, 0.3333333333333333703, 0.3299404806269776169, 0.3333333333333333703, 0.3299404806269776169, 0.3333333333333333703, 0.3299404806269776169, 0.3333333333333333703, 0.3299404806269776169, 0.3333333333333333703, 0.3299404806269776169, 0.3333333333333333703, 0.3299404806269776169, 0.3333333333333333703, 0.3299404806269776169, 0.3333333333333333703, 0.3299404806269776169, 0.3333333333333333703, 0.3299404806269776169, 0.3333333333333333703, 0.3299404806269776169, 0.3333333333333333703, 0.3299404806269776169, 0.3333333333333333703, 0.3299404806269776169, 0.3333333333333333703, 0.3299404806269776169, 0.3333333333333333703, 0.3299404806269776169, 0.3333333333333333703, 0.3299404806269776169, 0.3333333333333333703, 0.3299404806269776169, 0.3333333333333333703, 0.3299404806269776169, 0.3333333333333333703, 0.3299404806269776169, 0.3333333333333333703, 0.3299404806269776169, 0.3333333333333333703, 0.3299404806269776169, 0.3333333333333333703, 0.3299404806269776169, 0.3333333333333333703, 0.3299404806269776169, 0.3333333333333333703, 0.3299404806269776169, 0.3333333333333333703, 0.3299404806269776169, 0.3333333333333333703, 0.3299404806269776169, 0.3333333333333333703, 0.3299404806269776169, 0.3333333333333333703, 0.3299404806269776169, 0.3333333333333333703, 0.3299404806269776169, 0.3333333333333333703, 0.3299404806269776169, 0.3333333333333333703, 0.3299404806269776169, 0.3333333333333333703, 0.3299404806269776169, 0.3333333333333333703, 0.3299404806269776169, 0.3333333333333333703, 0.3299404806269776169, 0.3333333333333333703, 0.3299404806269776169, 0.3333333333333333703, 0.3299404806269776169, 0.3333333333333333703, 0.3299404806269776169, 0.3333333333333333703, 0.3299404806269776169, 0.3333333333333333703, 0.3299404806269776169, 0.3333333333333333703, 0.3299404806269776169, 0.3333333333333333703, 0.3299404806269776169, 0.3333333333333333703, 0.3299404806269776169, 0.3333333333333333703, 0.3299404806269776169, 0.3333333333333333703, 0.3299404806269776169, 0.3333333333333333703, 0.3299404806269776169, 0.3333333333333333703, 0.3299404806269776169, 0.3333333333333333703, 0.3299404806269776169, 0.3333333333333333703, 0.3299404806269776169, 0.3333333333333333703, 0.3299404806269776169, 0.3333333333333333703, 0.3299404806269776169, 0.3333333333333333703, 0.3299404806269776169, 0.3333333333333333703, 0.3299404806269776169, 0.3333333333333333703, 0.3299404806269776169, 0.3333333333333333703, 0.3299404806269776169, 0.3333333333333333703, 0.3299404806269776169, 0.3333333333333333703, 0.3299404806269776169, 0.3333333333333333703, 0.3299404806269776169, 0.3333333333333333703, 0.3299404806269776169, 0.3333333333333333703, 0.3299404806269776169, 0.3333333333333333703, 0.3299404806269776169, 0.3333333333333333703, 0.3299404806269776169, 0.3333333333333333703, 0.3299404806269776169, 0.3333333333333333703, 0.3299404806269776169, 0.3333333333333333703, 0.3299404806269776169, 0.3333333333333333703, 0.3299404806269776169, 0.3333333333333333703, 0.3299404806269776169, 0.3333333333333333703, 0.3299404806269776169, 0.3333333333333333703, 0.3299404806269776169, 0.3333333333333333703, 0.3299404806269776169, 0.3333333333333333703, 0.3299404806269776169, 0.3333333333333333703, 0.3299404806269776169, 0.3333333333333333703, 0.3299404806269776169, 0.3333333333333333703, 0.3299404806269776169, 0.3333333333333333703, 0.3299404806269776169, 0.3333333333333333703, 0.3299404806269776169, 0.3333333333333333703, 0.3299404806269776169, 0.3333333333333333703, 0.3299404806269776169, 0.3333333333333333703, 0.3299404806269776169, 0.3333333333333333703, 0.3299404806269776169, 0.3333333333333333703, 0.3299404806269776169, 0.3333333333333333703, 0.3299404806269776169, 0.3333333333333333703, 0.3299404806269776169, 0.3333333333333333703, 0.3299404806269776169, 0.3333333333333333703, 0.3299404806269776169, 0.3333333333333333703, 0.3299404806269776169, 0.3333333333333333703, 0.3299404806269776169, 0.3333333333333333703, 0.3299404806269776169, 0.3333333333333333703, 0.3299404806269776169, 0.3333333333333333703, 0.3299404806269776169, 0.3333333333333333703, 0.3299404806269776169, 0.3333333333333333703, 0.3299404806269776169, 0.3333333333333333703, 0.3299404806269776169, 0.3333333333333333703, 0.3299404806269776169, 0.3333333333333333703, 0.3299404806269776169, 0.3333333333333333703, 0.3299404806269776169, 0.3333333333333333703, 0.3299404806269776169, 0.3333333333333333703, 0.3299404806269776169, 0.3333333333333333703, 0.3299404806269776169, 0.3333333333333333703, 0.3299404806269776169, 0.3333333333333333703, 0.3299404806269776169, 0.3333333333333333703, 0.3299404806269776169, 0.3333333333333333703, 0.3299404806269776169, 0.3333333333333333703, 0.3299404806269776169, 0.3333333333333333703, 0.3299404806269776169, 0.3333333333333333703, 0.3299404806269776169, 0.3333333333333333703, 0.3299404806269776169, 0.3333333333333333703, 0.3299404806269776169, 0.3333333333333333703, 0.3299404806269776169, 0.3333333333333333703, 0.3299404806269776169, 0.3333333333333333703, 0.3299404806269776169, 0.3333333333333333703, 0.3299404806269776169, 0.3333333333333333703, 0.3299404806269776169, 0.3333333333333333703, 0.3299404806269776169, 0.3333333333333333703, 0.3299404806269776169, 0.3333333333333333703, 0.3299404806269776169, 0.3333333333333333703, 0.3299404806269776169, 0.3333333333333333703, 0.3299404806269776169, 0.3333333333333333703, 0.3299404806269776169, 0.3333333333333333703, 0.3299404806269776169, 0.3333333333333333703, 0.3299404806269776169, 0.3333333333333333703, 0.3299404806269776169, 0.3333333333333333703, 0.3299404806269776169, 0.3333333333333333703, 0.3299404806269776169, 0.3333333333333333703, 0.3299404806269776169, 0.3333333333333333703, 0.3299404806269776169, 0.3333333333333333703, 0.3299404806269776169, 0.3333333333333333703, 0.3299404806269776169, 0.3333333333333333703, 0.3299404806269776169, 0.3333333333333333703, 0.3299404806269776169, 0.3333333333333333703, 0.3299404806269776169, 0.3333333333333333703, 0.3299404806269776169, 0.3333333333333333703, 0.3299404806269776169, 0.3333333333333333703, 0.3299404806269776169, 0.3333333333333333703, 0.3320603117974822438, 0.3317425830320511193),
 ( 1.000000000000000000, 0.9898214418809326842, 1.000000000000000000, 0.9898214418809326842, 1.000000000000000000, 0.9898214418809326842, 1.000000000000000000, 0.9898214418809326842, 1.000000000000000000, 0.9898214418809326842, 1.000000000000000000, 0.9898214418809326842, 1.000000000000000000, 0.9898214418809326842, 1.000000000000000000, 0.9898214418809326842, 1.000000000000000000, 0.9898214418809326842, 1.000000000000000000, 0.9898214418809326842, 1.000000000000000000, 0.9898214418809326842, 1.000000000000000000, 0.9898214418809326842, 1.000000000000000000, 0.9898214418809326842, 1.000000000000000000, 0.9898214418809326842, 1.000000000000000000, 0.9898214418809326842, 1.000000000000000000, 0.9898214418809326842, 1.000000000000000000, 0.9898214418809326842, 1.000000000000000000, 0.9898214418809326842, 1.000000000000000000, 0.9898214418809326842, 1.000000000000000000, 0.9898214418809326842, 1.000000000000000000, 0.9898214418809326842, 1.000000000000000000, 0.9898214418809326842, 1.000000000000000000, 0.9898214418809326842, 1.000000000000000000, 0.9898214418809326842, 1.000000000000000000, 0.9898214418809326842, 1.000000000000000000, 0.9898214418809326842, 1.000000000000000000, 0.9898214418809326842, 1.000000000000000000, 0.9898214418809326842, 1.000000000000000000, 0.9898214418809326842, 1.000000000000000000, 0.9898214418809326842, 1.000000000000000000, 0.9898214418809326842, 1.000000000000000000, 0.9898214418809326842, 1.000000000000000000, 0.9898214418809326842, 1.000000000000000000, 0.9898214418809326842, 1.000000000000000000, 0.9898214418809326842, 1.000000000000000000, 0.9898214418809326842, 1.000000000000000000, 0.9898214418809326842, 1.000000000000000000, 0.9898214418809326842, 1.000000000000000000, 0.9898214418809326842, 1.000000000000000000, 0.9898214418809326842, 1.000000000000000000, 0.9898214418809326842, 1.000000000000000000, 0.9898214418809326842, 1.000000000000000000, 0.9898214418809326842, 1.000000000000000000, 0.9898214418809326842, 1.000000000000000000, 0.9898214418809326842, 1.000000000000000000, 0.9898214418809326842, 1.000000000000000000, 0.9898214418809326842, 1.000000000000000000, 0.9898214418809326842, 1.000000000000000000, 0.9898214418809326842, 1.000000000000000000, 0.9898214418809326842, 1.000000000000000000, 0.9898214418809326842, 1.000000000000000000, 0.9898214418809326842, 1.000000000000000000, 0.9898214418809326842, 1.000000000000000000, 0.9898214418809326842, 1.000000000000000000, 0.9898214418809326842, 1.000000000000000000, 0.9898214418809326842, 1.000000000000000000, 0.9898214418809326842, 1.000000000000000000, 0.9898214418809326842, 1.000000000000000000, 0.9898214418809326842, 1.000000000000000000, 0.9898214418809326842, 1.000000000000000000, 0.9898214418809326842, 1.000000000000000000, 0.9898214418809326842, 1.000000000000000000, 0.9898214418809326842, 1.000000000000000000, 0.9898214418809326842, 1.000000000000000000, 0.9898214418809326842, 1.000000000000000000, 0.9898214418809326842, 1.000000000000000000, 0.9898214418809326842, 1.000000000000000000, 0.9898214418809326842, 1.000000000000000000, 0.9898214418809326842, 1.000000000000000000, 0.9898214418809326842, 1.000000000000000000, 0.9898214418809326842, 1.000000000000000000, 0.9898214418809326842, 1.000000000000000000, 0.9898214418809326842, 1.000000000000000000, 0.9898214418809326842, 1.000000000000000000, 0.9898214418809326842, 1.000000000000000000, 0.9898214418809326842, 1.000000000000000000, 0.9898214418809326842, 1.000000000000000000, 0.9898214418809326842, 1.000000000000000000, 0.9898214418809326842, 1.000000000000000000, 0.9898214418809326842, 1.000000000000000000, 0.9898214418809326842, 1.000000000000000000, 0.9898214418809326842, 1.000000000000000000, 0.9898214418809326842, 1.000000000000000000, 0.9898214418809326842, 1.000000000000000000, 0.9898214418809326842, 1.000000000000000000, 0.9898214418809326842, 1.000000000000000000, 0.9898214418809326842, 1.000000000000000000, 0.9898214418809326842, 1.000000000000000000, 0.9898214418809326842, 1.000000000000000000, 0.9898214418809326842, 1.000000000000000000, 0.9898214418809326842, 1.000000000000000000, 0.9898214418809326842, 1.000000000000000000, 0.9898214418809326842, 1.000000000000000000, 0.9898214418809326842, 1.000000000000000000, 0.9898214418809326842, 1.000000000000000000, 0.9898214418809326842, 1.000000000000000000, 0.9898214418809326842, 1.000000000000000000, 0.9898214418809326842, 1.000000000000000000, 0.9898214418809326842, 1.000000000000000000, 0.9898214418809326842, 1.000000000000000000, 0.9898214418809326842, 1.000000000000000000, 0.9898214418809326842, 1.000000000000000000, 0.9898214418809326842, 1.000000000000000000, 0.9898214418809326842, 1.000000000000000000, 0.9898214418809326842, 1.000000000000000000, 0.9898214418809326842, 1.000000000000000000, 0.9898214418809326842, 1.000000000000000000, 0.9898214418809326842, 1.000000000000000000, 0.9898214418809326842, 1.000000000000000000, 0.9898214418809326842, 1.000000000000000000, 0.9898214418809326842, 1.000000000000000000, 0.9898214418809326842, 1.000000000000000000, 0.9898214418809326842, 1.000000000000000000, 0.9898214418809326842, 1.000000000000000000, 0.9898214418809326842, 1.000000000000000000, 0.9898214418809326842, 1.000000000000000000, 0.9898214418809326842, 1.000000000000000000, 0.9898214418809326842, 1.000000000000000000, 0.9898214418809326842, 1.000000000000000000, 0.9898214418809326842, 1.000000000000000000, 0.9898214418809326842, 1.000000000000000000, 0.9898214418809326842, 1.000000000000000000, 0.9898214418809326842, 1.000000000000000000, 0.9898214418809326842, 1.000000000000000000, 0.9898214418809326842, 1.000000000000000000, 0.9898214418809326842, 1.000000000000000000, 0.9898214418809326842, 1.000000000000000000, 0.9898214418809326842, 1.000000000000000000, 0.9898214418809326842, 1.000000000000000000, 0.9898214418809326842, 1.000000000000000000, 0.9898214418809326842, 1.000000000000000000, 0.9898214418809326842, 1.000000000000000000, 0.9898214418809326842, 1.000000000000000000, 0.9898214418809326842, 1.000000000000000000, 0.9898214418809326842, 1.000000000000000000, 0.9898214418809326842, 1.000000000000000000, 0.9898214418809326842, 1.000000000000000000, 0.9898214418809326842, 1.000000000000000000, 0.9898214418809326842, 1.000000000000000000, 0.9898214418809326842, 1.000000000000000000, 0.9898214418809326842, 1.000000000000000000, 0.9898214418809326842, 1.000000000000000000, 0.9898214418809326842, 1.000000000000000000, 0.9898214418809326842, 1.000000000000000000, 0.9898214418809326842, 1.000000000000000000, 0.9898214418809326842, 1.000000000000000000, 0.9898214418809326842, 1.000000000000000000, 0.9898214418809326842, 1.000000000000000000, 0.9898214418809326842, 1.000000000000000000, 0.9898214418809326842, 1.000000000000000000, 0.9898214418809326842, 1.000000000000000000, 0.9898214418809326842, 1.000000000000000000, 0.9898214418809326842, 1.000000000000000000, 0.9898214418809326842, 1.000000000000000000, 0.9898214418809326842, 1.000000000000000000, 0.9898214418809326842, 1.000000000000000000, 0.9898214418809326842, 1.000000000000000000, 0.9898214418809326842, 1.000000000000000000, 0.9898214418809326842, 1.000000000000000000, 0.9898214418809326842, 1.000000000000000000, 0.9898214418809326842, 1.000000000000000000, 0.9898214418809326842, 1.000000000000000000, 0.9898214418809326842, 1.000000000000000000, 0.9898214418809326842, 1.000000000000000000, 0.9898214418809326842, 1.000000000000000000, 0.9898214418809326842, 1.000000000000000000, 0.9898214418809326842, 1.000000000000000000, 0.9898214418809326842, 1.000000000000000000, 0.9898214418809326842, 1.000000000000000000, 0.9898214418809326842, 1.000000000000000000, 0.9898214418809326842, 1.000000000000000000, 0.9898214418809326842, 1.000000000000000000, 0.9898214418809326842, 1.000000000000000000, 0.9898214418809326842, 1.000000000000000000, 0.9898214418809326842, 1.000000000000000000, 0.9898214418809326842, 1.000000000000000000, 0.9898214418809326842, 1.000000000000000000, 0.9898214418809326842, 1.000000000000000000, 0.9898214418809326842, 1.000000000000000000, 0.9898214418809326842, 1.000000000000000000, 0.9898214418809326842, 1.000000000000000000, 0.9898214418809326842, 1.000000000000000000, 0.9898214418809326842, 1.000000000000000000, 0.9898214418809326842, 1.000000000000000000, 0.9898214418809326842, 1.000000000000000000, 0.9898214418809326842, 1.000000000000000000, 0.9898214418809326842, 1.000000000000000000, 0.9898214418809326842, 1.000000000000000000, 0.9898214418809326842, 1.000000000000000000, 0.9898214418809326842, 1.000000000000000000, 0.9898214418809326842, 1.000000000000000000, 0.9898214418809326842, 1.000000000000000000, 0.9898214418809326842, 1.000000000000000000, 0.9898214418809326842, 1.000000000000000000, 0.9898214418809326842, 1.000000000000000000, 0.9898214418809326842, 1.000000000000000000, 0.9898214418809326842, 1.000000000000000000, 0.9898214418809326842, 1.000000000000000000, 0.9898214418809326842, 1.000000000000000000, 0.9898214418809326842, 1.000000000000000000, 0.9898214418809326842, 1.000000000000000000, 0.9898214418809326842, 1.000000000000000000, 0.9898214418809326842, 1.000000000000000000, 0.9898214418809326842, 1.000000000000000000, 0.9898214418809326842, 1.000000000000000000, 0.9898214418809326842, 1.000000000000000000, 0.9898214418809326842, 1.000000000000000000, 0.9898214418809326842, 1.000000000000000000, 0.9898214418809326842, 1.000000000000000000, 0.9898214418809326842, 1.000000000000000000, 0.9898214418809326842, 1.000000000000000000, 0.9898214418809326842, 1.000000000000000000, 0.9898214418809326842, 1.000000000000000000, 0.9898214418809326842, 1.000000000000000000, 0.9898214418809326842, 1.000000000000000000, 0.9898214418809326842, 1.000000000000000000, 0.9898214418809326842, 1.000000000000000000, 0.9898214418809326842, 1.000000000000000000, 0.9898214418809326842, 1.000000000000000000, 0.9898214418809326842, 1.000000000000000000, 0.9898214418809326842, 1.000000000000000000, 0.9898214418809326842, 1.000000000000000000, 0.9898214418809326842, 1.000000000000000000, 0.9898214418809326842, 1.000000000000000000, 0.9898214418809326842, 1.000000000000000000, 0.9898214418809326842, 1.000000000000000000, 0.9898214418809326842, 1.000000000000000000, 0.9898214418809326842, 1.000000000000000000, 0.9898214418809326842, 1.000000000000000000, 0.9898214418809326842, 1.000000000000000000, 0.9898214418809326842, 1.000000000000000000, 0.9898214418809326842, 1.000000000000000000, 0.9898214418809326842, 1.000000000000000000, 0.9898214418809326842, 1.000000000000000000, 0.9898214418809326842, 1.000000000000000000, 0.9898214418809326842, 1.000000000000000000, 0.9898214418809326842, 1.000000000000000000, 0.9898214418809326842, 1.000000000000000000, 0.9898214418809326842, 1.000000000000000000, 0.9898214418809326842, 1.000000000000000000, 0.9898214418809326842, 1.000000000000000000, 0.9898214418809326842, 1.000000000000000000, 0.9898214418809326842, 1.000000000000000000, 0.9898214418809326842, 1.000000000000000000, 0.9898214418809326842, 1.000000000000000000, 0.9898214418809326842, 1.000000000000000000, 0.9898214418809326842, 1.000000000000000000, 0.9898214418809326842, 1.000000000000000000, 0.9898214418809326842, 1.000000000000000000, 0.9898214418809326842, 1.000000000000000000, 0.9898214418809326842, 1.000000000000000000, 0.9898214418809326842, 1.000000000000000000, 0.9898214418809326842, 1.000000000000000000, 0.9898214418809326842, 1.000000000000000000, 0.9898214418809326842, 1.000000000000000000, 0.9898214418809326842, 1.000000000000000000, 0.9898214418809326842, 1.000000000000000000, 0.9898214418809326842, 1.000000000000000000, 0.9898214418809326842, 1.000000000000000000, 0.9898214418809326842, 1.000000000000000000, 0.9898214418809326842, 1.000000000000000000, 0.9898214418809326842, 1.000000000000000000, 0.9898214418809326842, 1.000000000000000000, 0.9898214418809326842, 1.000000000000000000, 0.9898214418809326842, 1.000000000000000000, 0.9898214418809326842, 1.000000000000000000, 0.9898214418809326842, 1.000000000000000000, 0.9898214418809326842, 1.000000000000000000, 0.9898214418809326842, 1.000000000000000000, 0.9898214418809326842, 1.000000000000000000, 0.9898214418809326842, 1.000000000000000000, 0.9898214418809326842, 1.000000000000000000, 0.9898214418809326842, 1.000000000000000000, 0.9898214418809326842, 1.000000000000000000, 0.9898214418809326842, 1.000000000000000000, 0.9898214418809326842, 1.000000000000000000, 0.9898214418809326842, 1.000000000000000000, 0.9898214418809326842, 1.000000000000000000, 0.9898214418809326842, 1.000000000000000000, 0.9898214418809326842, 1.000000000000000000, 0.9898214418809326842, 1.000000000000000000, 0.9898214418809326842, 1.000000000000000000, 0.9898214418809326842, 1.000000000000000000, 0.9898214418809326842, 1.000000000000000000, 0.9898214418809326842, 1.000000000000000000, 0.9898214418809326842, 1.000000000000000000, 0.9898214418809326842, 1.000000000000000000, 0.9898214418809326842, 1.000000000000000000, 0.9898214418809326842, 1.000000000000000000, 0.9898214418809326842, 1.000000000000000000, 0.9898214418809326842, 1.000000000000000000, 0.9898214418809326842, 1.000000000000000000, 0.9898214418809326842, 1.000000000000000000, 0.9898214418809326842, 1.000000000000000000, 0.9898214418809326842, 1.000000000000000000, 0.9898214418809326842, 1.000000000000000000, 0.9898214418809326842, 1.000000000000000000, 0.9898214418809326842, 1.000000000000000000, 0.9898214418809326842, 1.000000000000000000, 0.9898214418809326842, 1.000000000000000000, 0.9898214418809326842, 1.000000000000000000, 0.9898214418809326842, 1.000000000000000000, 0.9898214418809326842, 1.000000000000000000, 0.9898214418809326842, 1.000000000000000000, 0.9898214418809326842, 1.000000000000000000, 0.9898214418809326842, 1.000000000000000000, 0.9898214418809326842, 1.000000000000000000, 0.9898214418809326842, 1.000000000000000000, 0.9898214418809326842, 1.000000000000000000, 0.9898214418809326842, 1.000000000000000000, 0.9898214418809326842, 1.000000000000000000, 0.9898214418809326842, 1.000000000000000000, 0.9898214418809326842, 1.000000000000000000, 0.9898214418809326842, 1.000000000000000000, 0.9898214418809326842, 1.000000000000000000, 0.9898214418809326842, 1.000000000000000000, 0.9898214418809326842, 1.000000000000000000, 0.9898214418809326842, 1.000000000000000000, 0.9898214418809326842, 1.000000000000000000, 0.9898214418809326842, 1.000000000000000000, 0.9898214418809326842, 1.000000000000000000, 0.9898214418809326842, 1.000000000000000000, 0.9898214418809326842, 1.000000000000000000, 0.9898214418809326842, 1.000000000000000000, 0.9898214418809326842, 1.000000000000000000, 0.9898214418809326842, 1.000000000000000000, 0.9898214418809326842, 1.000000000000000000, 0.9898214418809326842, 1.000000000000000000, 0.9898214418809326842, 1.000000000000000000, 0.9898214418809326842, 1.000000000000000000, 0.9898214418809326842, 1.000000000000000000, 0.9898214418809326842, 1.000000000000000000, 0.9898214418809326842, 1.000000000000000000, 0.9898214418809326842, 1.000000000000000000, 0.9898214418809326842, 1.000000000000000000, 0.9898214418809326842, 1.000000000000000000, 0.9898214418809326842, 1.000000000000000000, 0.9898214418809326842, 1.000000000000000000, 0.9898214418809326842, 1.000000000000000000, 0.9898214418809326842, 1.000000000000000000, 0.9898214418809326842, 1.000000000000000000, 0.9898214418809326842, 1.000000000000000000, 0.9898214418809326842, 1.000000000000000000, 0.9898214418809326842, 1.000000000000000000, 0.9898214418809326842, 1.000000000000000000, 0.9898214418809326842, 1.000000000000000000, 0.9898214418809326842, 1.000000000000000000, 0.9898214418809326842, 1.000000000000000000, 0.9898214418809326842, 1.000000000000000000, 0.9898214418809326842, 1.000000000000000000, 0.9898214418809326842, 1.000000000000000000, 0.9898214418809326842, 1.000000000000000000, 0.9898214418809326842, 1.000000000000000000, 0.9898214418809326842, 1.000000000000000000, 0.9898214418809326842, 1.000000000000000000, 0.9898214418809326842, 1.000000000000000000, 0.9898214418809326842, 1.000000000000000000, 0.9898214418809326842, 1.000000000000000000, 0.9898214418809326842, 1.000000000000000000, 0.9898214418809326842, 1.000000000000000000, 0.9898214418809326842, 1.000000000000000000, 0.9898214418809326842, 1.000000000000000000, 0.9898214418809326842, 1.000000000000000000, 0.9898214418809326842, 1.000000000000000000, 0.9898214418809326842, 1.000000000000000000, 0.9898214418809326842, 1.000000000000000000, 0.9898214418809326842, 1.000000000000000000, 0.9898214418809326842, 1.000000000000000000, 0.9898214418809326842, 1.000000000000000000, 0.9898214418809326842, 1.000000000000000000, 0.9898214418809326842, 1.000000000000000000, 0.9898214418809326842, 1.000000000000000000, 0.9898214418809326842, 1.000000000000000000, 0.9898214418809326842, 1.000000000000000000, 0.9898214418809326842, 1.000000000000000000, 0.9898214418809326842, 1.000000000000000000, 0.9898214418809326842, 1.000000000000000000, 0.9898214418809326842, 1.000000000000000000, 0.9898214418809326842, 1.000000000000000000, 0.9898214418809326842, 1.000000000000000000, 0.9898214418809326842, 1.000000000000000000, 0.9898214418809326842, 1.000000000000000000, 0.9898214418809326842, 1.000000000000000000, 0.9898214418809326842, 1.000000000000000000, 0.9898214418809326842, 1.000000000000000000, 0.9898214418809326842, 1.000000000000000000, 0.9898214418809326842, 1.000000000000000000, 0.9898214418809326842, 1.000000000000000000, 0.9898214418809326842, 1.000000000000000000, 0.9898214418809326842, 1.000000000000000000, 0.9898214418809326842, 1.000000000000000000, 0.9898214418809326842, 1.000000000000000000, 0.9898214418809326842, 1.000000000000000000, 0.9898214418809326842, 1.000000000000000000, 0.9898214418809326842, 1.000000000000000000, 0.9898214418809326842, 1.000000000000000000, 0.9898214418809326842, 1.000000000000000000, 0.9898214418809326842, 1.000000000000000000, 0.9898214418809326842, 1.000000000000000000, 0.9898214418809326842, 1.000000000000000000, 0.9898214418809326842, 1.000000000000000000, 0.9898214418809326842, 1.000000000000000000, 0.9898214418809326842, 1.000000000000000000, 0.9898214418809326842, 1.000000000000000000, 0.9898214418809326842, 1.000000000000000000, 0.9898214418809326842, 1.000000000000000000, 0.9898214418809326842, 1.000000000000000000, 0.9898214418809326842, 1.000000000000000000, 0.9898214418809326842, 1.000000000000000000, 0.9898214418809326842, 1.000000000000000000, 0.9898214418809326842, 1.000000000000000000, 0.9898214418809326842, 1.000000000000000000, 0.9898214418809326842, 1.000000000000000000, 0.9898214418809326842, 1.000000000000000000, 0.9898214418809326842, 1.000000000000000000, 0.9898214418809326842, 1.000000000000000000, 0.9898214418809326842, 1.000000000000000000, 0.9898214418809326842, 1.000000000000000000, 0.9898214418809326842, 1.000000000000000000, 0.9898214418809326842, 1.000000000000000000, 0.9898214418809326842, 1.000000000000000000, 0.9898214418809326842, 1.000000000000000000, 0.9898214418809326842, 1.000000000000000000, 0.9898214418809326842, 1.000000000000000000, 0.9898214418809326842, 1.000000000000000000, 0.9898214418809326842, 1.000000000000000000, 0.9898214418809326842, 1.000000000000000000, 0.9898214418809326842, 1.000000000000000000, 0.9898214418809326842, 1.000000000000000000, 0.9898214418809326842, 1.000000000000000000, 0.9961809353924466759, 0.9952277490961531914) ) ) 
 REPRESENTATION_ITEM ( '' )  SURFACE ( )  );
#43035 = CARTESIAN_POINT ( 'NONE',  ( 989.9999999999992042, -419.8175818341089780, 209.9999999999999716 ) ) ;
#43036 = CARTESIAN_POINT ( 'NONE',  ( 784.1219089521767955, -141.2817908451530400, -315.0488828828318333 ) ) ;
#43037 = CARTESIAN_POINT ( 'NONE',  ( 814.2001403089898304, -17.36187538569322086, 347.4397851343538264 ) ) ;
#43038 = CIRCLE ( 'NONE', #23096, 20.00000000000004619 ) ;
#43039 = DIRECTION ( 'NONE',  ( 1.000000000000000000, -0.000000000000000000, -0.000000000000000000 ) ) ;
#43040 = CARTESIAN_POINT ( 'NONE',  ( 803.8556311672234642, -9.623778108051251223, -365.6418435158340117 ) ) ;
#43041 = CARTESIAN_POINT ( 'NONE',  ( 767.6429770376291799, -345.1800572038739574, -306.8695393053162093 ) ) ;
#43042 = CARTESIAN_POINT ( 'NONE',  ( 787.4999999999992042, -512.9681489794448908, -339.9999999999999432 ) ) ;
#43043 = CARTESIAN_POINT ( 'NONE',  ( 771.1735550268778070, -9.180057203875058747, 316.3353852180827630 ) ) ;
#43044 = AXIS2_PLACEMENT_3D ( 'NONE', #20296, #27237, #41329 ) ;
#43045 = ADVANCED_FACE ( 'NONE', ( #8011, #4529, #25769 ), #39881, .T. ) ;
#43046 = CARTESIAN_POINT ( 'NONE',  ( 786.2694204179717872, -285.2817908451526137, 305.1769319972829067 ) ) ;
#43047 = CARTESIAN_POINT ( 'NONE',  ( 764.3348316497523456, -190.7146871989597798, -308.6759233522265617 ) ) ;
#43048 = CARTESIAN_POINT ( 'NONE',  ( 808.3070685750230950, -234.9982390220561683, 361.1904061080339261 ) ) ;
#43049 = CARTESIAN_POINT ( 'NONE',  ( 810.1134526219336749, -440.5328690171407970, -357.8822607201570349 ) ) ;
#43050 = CARTESIAN_POINT ( 'NONE',  ( -200.7583438952259485, 394.6698570112193920, -274.9999999999999432 ) ) ;
#43051 = EDGE_CURVE ( 'NONE', #44542, #30554, #22318, .T. ) ;
#43052 = CARTESIAN_POINT ( 'NONE',  ( -879.9999999999992042, 240.0000000000000568, -244.9999999999999716 ) ) ;
#43053 = CARTESIAN_POINT ( 'NONE',  ( 791.9812246680005501, -332.6346026584195101, 361.9419747391813189 ) ) ;
#43054 = CARTESIAN_POINT ( 'NONE',  ( 773.4516893846965786, -91.64542720878951343, 315.8398074228977066 ) ) ;
#43055 = CARTESIAN_POINT ( 'NONE',  ( 789.9200121543843807, 22.01258552831228599, -317.0176451133914384 ) ) ;
#43056 = FACE_OUTER_BOUND ( 'NONE', #36607, .T. ) ;
#43057 = DIRECTION ( 'NONE',  ( -1.084653538143406060E-16, 0.6594541114781790059, 0.7517448203044204691 ) ) ;
#43059 = CARTESIAN_POINT ( 'NONE',  ( 802.1676090361156639, -374.6346026584192828, 327.8955696845344505 ) ) ;
#43058 = CARTESIAN_POINT ( 'NONE',  ( 801.3366627262608972, -152.5328690171416781, 353.0897708529566899 ) ) ;
#43060 = ORIENTED_EDGE ( 'NONE', *, *, #24640, .T. ) ;
#43061 = ADVANCED_FACE ( 'NONE', ( #40992 ), #34047, .T. ) ;
#43062 = CARTESIAN_POINT ( 'NONE',  ( 790.8726784830453198, -298.7146871989593251, -362.5472867521010585 ) ) ;
#43063 = PRODUCT_DEFINITION_CONTEXT ( 'detailed design', #16367, 'design' ) ;
#43064 = CARTESIAN_POINT ( 'NONE',  ( 783.7566961878529810, -288.8965053807775121, -305.1792804349288417 ) ) ;
#43065 = CARTESIAN_POINT ( 'NONE',  ( 779.9999999999992042, 166.4563064324884465, -339.9999999999999432 ) ) ;
#43066 = CARTESIAN_POINT ( 'NONE',  ( 796.7737145352015204, 3.365397341579444479, 370.7187646348536987 ) ) ;
#43067 = ORIENTED_EDGE ( 'NONE', *, *, #11114, .F. ) ;
#43068 = CARTESIAN_POINT ( 'NONE',  ( 768.0187753319979720, -320.6346026584195670, 318.0580252608186242 ) ) ;
#43069 = CARTESIAN_POINT ( 'NONE',  ( 773.3843516231979720, -85.44195992623282621, -364.4086373105754433 ) ) ;
#43070 = CARTESIAN_POINT ( 'NONE',  ( 764.8639956371174549, -440.0891481129644944, 319.7806653035542013 ) ) ;
#43071 = CARTESIAN_POINT ( 'NONE',  ( 805.0032342141412300, -133.5436935675110135, -314.9967657858571783 ) ) ;
#43072 = ORIENTED_EDGE ( 'NONE', *, *, #8870, .F. ) ;
#43073 = CIRCLE ( 'NONE', #15766, 2.749999999999835687 ) ;
#43074 = CARTESIAN_POINT ( 'NONE',  ( 797.8594530101009923, -157.5436935675109282, -322.1405469898982119 ) ) ;
#43075 = AXIS2_PLACEMENT_3D ( 'NONE', #20197, #40763, #43999 ) ;
#43076 = ORIENTED_EDGE ( 'NONE', *, *, #43599, .T. ) ;
#43077 = CARTESIAN_POINT ( 'NONE',  ( 799.2566176426618085, -408.0090635724249069, -324.0069404352559559 ) ) ;
#43078 = EDGE_CURVE ( 'NONE', #42263, #5389, #2644, .T. ) ;
#43079 = CARTESIAN_POINT ( 'NONE',  ( 804.6798772138708955, 8.274488250670337663, 334.6312213355107019 ) ) ;
#43080 = CARTESIAN_POINT ( 'NONE',  ( 746.8695393053150156, -221.9073299311470464, 327.6429770376306010 ) ) ;
#43081 = CARTESIAN_POINT ( 'NONE',  ( 775.9200461376533440, -143.8055962898690154, 315.3028492785443291 ) ) ;
#43084 = CARTESIAN_POINT ( 'NONE',  ( 744.9990715423526808, -378.3510508353227806, 341.2370466360926002 ) ) ;
#43083 = CARTESIAN_POINT ( 'NONE',  ( 311.1634899080286232, 256.5000000000000000, -206.1189999999963050 ) ) ;
#43082 = DIRECTION ( 'NONE',  ( -0.000000000000000000, -0.000000000000000000, 1.000000000000000000 ) ) ;
#43085 = ORIENTED_EDGE ( 'NONE', *, *, #21300, .F. ) ;
#43086 = CARTESIAN_POINT ( 'NONE',  ( 763.8424801807145741, -402.0090635724250205, -320.5453621957614700 ) ) ;
#43087 = LINE ( 'NONE', #25760, #43244 ) ;
#43088 = CARTESIAN_POINT ( 'NONE',  ( 764.1737431748507561, -202.3726999360618777, -371.6461892240376415 ) ) ;
#43089 = CARTESIAN_POINT ( 'NONE',  ( 766.4474001241216001, -67.09997266333506616, 307.3154664389482491 ) ) ;
#43090 = VECTOR ( 'NONE', #13732, 1000.000000000000000 ) ;
#43092 = CARTESIAN_POINT ( 'NONE',  ( -338.8365100919713200, 230.0000000000001137, -197.2499999999919282 ) ) ;
#43091 = CARTESIAN_POINT ( 'NONE',  ( 51.16348990802859475, 260.0000000000000568, -199.9999999999945146 ) ) ;
#43093 = CARTESIAN_POINT ( 'NONE',  ( 757.2208543904082489, -328.7146871989592682, -350.9844846989624330 ) ) ;
#43094 = DIRECTION ( 'NONE',  ( 0.000000000000000000, 0.000000000000000000, 1.000000000000000000 ) ) ;
#43095 = CARTESIAN_POINT ( 'NONE',  ( 746.4236121716829757, -183.8272453906074020, -328.8385539511384650 ) ) ;
#43096 = FACE_OUTER_BOUND ( 'NONE', #8987, .T. ) ;
#43097 = FACE_BOUND ( 'NONE', #13211, .T. ) ;
#43098 = CARTESIAN_POINT ( 'NONE',  ( 793.9708237608222134, -406.9181544815157849, 319.2295555964448681 ) ) ;
#43099 = CARTESIAN_POINT ( 'NONE',  ( 811.0346526505617248, -254.6346026584197091, -323.0537975583478101 ) ) ;
#43100 = DIRECTION ( 'NONE',  ( -2.750100768424433062E-32, 1.672022627447525240E-16, -1.000000000000000000 ) ) ;
#43101 = CARTESIAN_POINT ( 'NONE',  ( 802.1676090361156639, -14.63460265842049424, -327.8955696845344505 ) ) ;
#43102 = EDGE_CURVE ( 'NONE', #24267, #25862, #37752, .T. ) ;
#43103 = EDGE_CURVE ( 'NONE', #15531, #14461, #20421, .T. ) ;
#43104 = CARTESIAN_POINT ( 'NONE',  ( 752.7379699480933368, -156.0090635724256742, 361.9858362298580232 ) ) ;
#43105 = CARTESIAN_POINT ( 'NONE',  ( 776.2433038121456548, -84.89650538077830788, -374.8207195650711014 ) ) ;
#43106 = CARTESIAN_POINT ( 'NONE',  ( 772.5602148656447525, -129.7255117493292289, 305.7998596910095443 ) ) ;
#43107 = CARTESIAN_POINT ( 'NONE',  ( 782.4968714119720516, -346.8164208402376971, -305.0891759886411023 ) ) ;
#43108 = CARTESIAN_POINT ( 'NONE',  ( 441.1634899080286232, 256.4999999999999432, -199.9999999999972431 ) ) ;
#43110 = EDGE_CURVE ( 'NONE', #34351, #16943, #34516, .T. ) ;
#43109 = DIRECTION ( 'NONE',  ( 0.000000000000000000, 0.000000000000000000, 1.000000000000000000 ) ) ;
#43111 = CARTESIAN_POINT ( 'NONE',  ( 794.9819416627830151, -228.9982390220561683, 319.9864689768909898 ) ) ;
#43112 = AXIS2_PLACEMENT_3D ( 'NONE', #9556, #26418, #1688 ) ;
#43113 = AXIS2_PLACEMENT_3D ( 'NONE', #34462, #20593, #41620 ) ;
#43114 = CARTESIAN_POINT ( 'NONE',  ( 771.3260364891663130, -451.6454272087884192, 306.0683387631859773 ) ) ;
#43115 = CARTESIAN_POINT ( 'NONE',  ( 771.2368401574024119, -421.4419599262317888, -374.2805881961240857 ) ) ;
#43116 = CARTESIAN_POINT ( 'NONE',  ( 814.8207195650702488, -2.190881754244347945, -336.2433038121456548 ) ) ;
#43117 = DIRECTION ( 'NONE',  ( -0.000000000000000000, -0.000000000000000000, 1.000000000000000000 ) ) ;
#43118 = CARTESIAN_POINT ( 'NONE',  ( 749.8865473780648472, -20.53286901714212931, 322.1177392798429082 ) ) ;
#43119 = EDGE_CURVE ( 'NONE', #28026, #16303, #17412, .T. ) ;
#43120 = CARTESIAN_POINT ( 'NONE',  ( 784.0799538623451781, -179.8055962898688733, -364.6971507214555572 ) ) ;
#43121 = CARTESIAN_POINT ( 'NONE',  ( 800.2193346964447755, -18.99823902205683979, 355.1360043628815788 ) ) ;
#43122 = CARTESIAN_POINT ( 'NONE',  ( 814.8230680027162407, -197.8055962898688733, -333.7305795820267917 ) ) ;
#43123 = CARTESIAN_POINT ( 'NONE',  ( 813.2346286133761168, -341.2601417444138292, 328.9521613784389160 ) ) ;
#43124 = CARTESIAN_POINT ( 'NONE',  ( 797.6776695296629214, -139.5436935675110135, 357.6776695296636603 ) ) ;
#43125 = ORIENTED_EDGE ( 'NONE', *, *, #16471, .F. ) ;
#43126 = VECTOR ( 'NONE', #29764, 1000.000000000000000 ) ;
#43127 = CARTESIAN_POINT ( 'NONE',  ( 761.9338519418445230, -422.5328690171408539, 370.4231160770881957 ) ) ;
#43128 = CARTESIAN_POINT ( 'NONE',  ( 803.6646147819161570, -137.9073299311473875, -348.8264449731210561 ) ) ;
#43129 = CARTESIAN_POINT ( 'NONE',  ( 764.8639956371174549, -344.0891481129647786, 319.7806653035542013 ) ) ;
#43130 = AXIS2_PLACEMENT_3D ( 'NONE', #328, #7281, #35896 ) ;
#43131 = CARTESIAN_POINT ( 'NONE',  ( 746.8695393053150156, -53.90732993114765037, -327.6429770376306010 ) ) ;
#43132 = ORIENTED_EDGE ( 'NONE', *, *, #22159, .T. ) ;
#43133 = CARTESIAN_POINT ( 'NONE',  ( 747.6481478633932056, -445.0999726633338582, -353.4146539503763620 ) ) ;
#43134 = ORIENTED_EDGE ( 'NONE', *, *, #29222, .T. ) ;
#43135 = CARTESIAN_POINT ( 'NONE',  ( 784.1219089521767955, -333.2817908451523863, -315.0488828828318333 ) ) ;
#43136 = CONTEXT_DEPENDENT_SHAPE_REPRESENTATION ( #2205, #17794 ) ;
#43138 = CARTESIAN_POINT ( 'NONE',  ( 776.9254006560222479, -380.1908817542431507, 314.8983024940802125 ) ) ;
#43137 = CARTESIAN_POINT ( 'NONE',  ( 781.7834795799800531, -58.81642084023854267, 315.0636971347436202 ) ) ;
#43139 = CARTESIAN_POINT ( 'NONE',  ( 800.0135310231082713, -302.0891481129650629, -325.0180583372163028 ) ) ;
#43141 = CARTESIAN_POINT ( 'NONE',  ( 758.0141637701419768, -303.0783235625957559, 367.2620300519063790 ) ) ;
#43140 = CARTESIAN_POINT ( 'NONE',  ( 751.6929314249750860, -390.9982390220556567, 318.8095938919659034 ) ) ;
#43142 = CARTESIAN_POINT ( 'NONE',  ( 801.9858362298568863, -75.07832356259649487, 312.7379699480935642 ) ) ;
#43143 = CARTESIAN_POINT ( 'NONE',  ( 757.4527132478984868, -280.3726999360616787, -329.1273215169538844 ) ) ;
#43144 = CARTESIAN_POINT ( 'NONE',  ( 805.1927285166397041, -280.8164208402378677, -341.8018195045277707 ) ) ;
#43145 = DIRECTION ( 'NONE',  ( -0.000000000000000000, -1.110223024625155554E-15, 1.000000000000000000 ) ) ;
#43146 = CARTESIAN_POINT ( 'NONE',  ( 759.9864689768902508, -122.0891481129656171, -354.9819416627836404 ) ) ;
#43147=STYLED_ITEM('',(#45779),#2718);
#43148 = DIRECTION ( 'NONE',  ( 1.000000000000000000, 0.000000000000000000, 0.000000000000000000 ) ) ;
#43149 = ORIENTED_EDGE ( 'NONE', *, *, #10566, .F. ) ;
#43150 = CARTESIAN_POINT ( 'NONE',  ( 815.2698199232961542, -424.8164208402372992, 342.5225473063383106 ) ) ;
#43151 = VECTOR ( 'NONE', #43039, 1000.000000000000000 ) ;
#43153 = LINE ( 'NONE', #14534, #15981 ) ;
#43152 = CARTESIAN_POINT ( 'NONE',  ( 766.1799889109151991, 20.32535068748918050, 313.3728091324376237 ) ) ;
#43154 = CARTESIAN_POINT ( 'NONE',  ( 804.1009440267234822, -71.46360902697141171, -314.0944755984392600 ) ) ;
#43155 = CARTESIAN_POINT ( 'NONE',  ( 919.9999999999993179, 154.9999999999998863, 339.9999999999999432 ) ) ;
#43156 = DIRECTION ( 'NONE',  ( -1.000000000000000000, -0.000000000000000000, -0.000000000000000000 ) ) ;
#43157 = CARTESIAN_POINT ( 'NONE',  ( 805.2837595273609850, -290.7363362996980527, 340.5290396650784714 ) ) ;
#43158 = CARTESIAN_POINT ( 'NONE',  ( 778.2165204200184689, -166.8164208402382087, 364.9363028652563230 ) ) ;
#43159 = ORIENTED_EDGE ( 'NONE', *, *, #41073, .T. ) ;
#43160 = CARTESIAN_POINT ( 'NONE',  ( 749.2812353651451076, -102.4527844766020337, -323.2262854647983090 ) ) ;
#43161 = CARTESIAN_POINT ( 'NONE',  ( 805.0264073115434940, -318.3510508353230080, 339.4763451958999099 ) ) ;
#43162 = DIRECTION ( 'NONE',  ( -1.000000000000000000, 0.000000000000000000, 0.000000000000000000 ) ) ;
#43163 = VECTOR ( 'NONE', #32027, 1000.000000000000000 ) ;
#43164 = CARTESIAN_POINT ( 'NONE',  ( 776.2046728542105711, -44.19088175424421649, 304.8212110874238761 ) ) ;
#43165 = CARTESIAN_POINT ( 'NONE',  ( 749.2812353651451076, -222.4527844766016642, -323.2262854647983090 ) ) ;
#43166 = AXIS2_PLACEMENT_3D ( 'NONE', #20444, #38235, #20659 ) ;
#43167 = CARTESIAN_POINT ( 'NONE',  ( 791.9812246680005501, -116.6346026584201780, 361.9419747391813189 ) ) ;
#43168 = DIRECTION ( 'NONE',  ( 0.000000000000000000, 0.000000000000000000, 1.000000000000000000 ) ) ;
#43169 = CARTESIAN_POINT ( 'NONE',  ( 781.2497674668890113, -324.3510508353229511, -375.3608509340180603 ) ) ;
#43170 = CARTESIAN_POINT ( 'NONE',  ( 763.8424801807145741, 5.990936427573807954, 320.5453621957614700 ) ) ;
#43171 = CARTESIAN_POINT ( 'NONE',  ( 787.4397851343537695, -309.7255117493287457, -374.2001403089903988 ) ) ;
#43172 = FACE_OUTER_BOUND ( 'NONE', #25131, .T. ) ;
#43173 = CARTESIAN_POINT ( 'NONE',  ( 800.7704444035546203, -412.1692326535045936, 326.0291762391768771 ) ) ;
#43174 = ORIENTED_EDGE ( 'NONE', *, *, #18364, .T. ) ;
#43175 = CARTESIAN_POINT ( 'NONE',  ( 804.9363028652555840, -424.2709662947829088, -338.2165204200192079 ) ) ;
#43176 = CARTESIAN_POINT ( 'NONE',  ( 759.8311093483677041, -94.16923265350555994, -310.9282345327691814 ) ) ;
#43177 = DIRECTION ( 'NONE',  ( -0.000000000000000000, 1.000000000000000000, -0.000000000000000000 ) ) ;
#43178 = CARTESIAN_POINT ( 'NONE',  ( 781.2497674668890113, -228.3510508353232922, 375.3608509340180603 ) ) ;
#43179 = CARTESIAN_POINT ( 'NONE',  ( 767.8955696845334842, -48.45278447660221133, 362.1676090361161755 ) ) ;
#43180 = AXIS2_PLACEMENT_3D ( 'NONE', #12746, #4922, #26825 ) ;
#43181 = ORIENTED_EDGE ( 'NONE', *, *, #43367, .F. ) ;
#43182 = CARTESIAN_POINT ( 'NONE',  ( 803.8651313633788504, -245.2601417444141987, -332.4468031744301015 ) ) ;
#43183 = CARTESIAN_POINT ( 'NONE',  ( 792.1044303154645831, -228.4527844766015789, 317.8323909638837677 ) ) ;
#43184 = CARTESIAN_POINT ( 'NONE',  ( 803.8556311672234642, -57.62377810805111267, -365.6418435158340117 ) ) ;
#43185 = CARTESIAN_POINT ( 'NONE',  ( 799.5976253717891495, -452.9681489794447771, -356.1016198435977458 ) ) ;
#43186 = ORIENTED_EDGE ( 'NONE', *, *, #29862, .F. ) ;
#43187 = CARTESIAN_POINT ( 'NONE',  ( 776.2046728542105711, -356.1908817542432075, -304.8212110874238761 ) ) ;
#43188 = VECTOR ( 'NONE', #40351, 1000.000000000000000 ) ;
#43189 = CARTESIAN_POINT ( 'NONE',  ( 814.5518280994195948, -279.7255117493288026, 332.4837098697145166 ) ) ;
#43190 = CARTESIAN_POINT ( 'NONE',  ( 773.7943932421234194, 0.1944037101305369775, 305.5313806188329409 ) ) ;
#43191 = CARTESIAN_POINT ( 'NONE',  ( 775.8780910478218402, -177.2817908451528695, -364.9511171171680530 ) ) ;
#43192 = CARTESIAN_POINT ( 'NONE',  ( 804.4286716492782716, -185.3618753856926844, -345.3141322388244703 ) ) ;
#43193 = CARTESIAN_POINT ( 'NONE',  ( 771.1735550268780344, -369.1800572038739006, -316.3353852180828198 ) ) ;
#43194 = ORIENTED_EDGE ( 'NONE', *, *, #26868, .T. ) ;
#43195 = CARTESIAN_POINT ( 'NONE',  ( 805.0264073115434940, 17.64894916467593688, -339.4763451958999099 ) ) ;
#43196 = EDGE_LOOP ( 'NONE', ( #14874, #36192 ) ) ;
#43197 = CARTESIAN_POINT ( 'NONE',  ( 800.9747183278959710, -324.9982390220559409, 311.9810565676471583 ) ) ;
#43198 = FACE_OUTER_BOUND ( 'NONE', #35039, .T. ) ;
#43199 = CARTESIAN_POINT ( 'NONE',  ( 757.2208543904082489, -352.7146871989593251, 350.9844846989624330 ) ) ;
#43200 = DIRECTION ( 'NONE',  ( 1.000000000000000000, -0.000000000000000000, -0.000000000000000000 ) ) ;
#43201 = CARTESIAN_POINT ( 'NONE',  ( 760.7433823573367135, -156.0090635724256742, 355.9930595647440441 ) ) ;
#43202 = CARTESIAN_POINT ( 'NONE',  ( 755.0636971347428243, -52.27096629478401724, 341.7834795799807353 ) ) ;
#43203 = ORIENTED_EDGE ( 'NONE', *, *, #11778, .T. ) ;
#43204 = CARTESIAN_POINT ( 'NONE',  ( 762.1177392798416577, -402.5545181178795247, -309.8865473780659272 ) ) ;
#43205 = AXIS2_PLACEMENT_3D ( 'NONE', #13267, #9571, #23631 ) ;
#43206 = CARTESIAN_POINT ( 'NONE',  ( 808.0189434323515343, -14.08914811296595460, -319.0252816721025511 ) ) ;
#43207 = CARTESIAN_POINT ( 'NONE',  ( 752.7379699480933368, -276.0090635724253048, 361.9858362298580232 ) ) ;
#43208 = CARTESIAN_POINT ( 'NONE',  ( 787.6308680596127942, -227.2601417444141987, 364.1105419155492768 ) ) ;
#43209 = CARTESIAN_POINT ( 'NONE',  ( 774.6858677611749044, -345.7255117493285184, -315.5713283507209894 ) ) ;
#43210 = CARTESIAN_POINT ( 'NONE',  ( 781.7834795799800531, 13.18357915976123174, -315.0636971347436202 ) ) ;
#43211 = CARTESIAN_POINT ( 'NONE',  ( 762.1405469898971887, -1.543693567511449150, 357.8594530101015607 ) ) ;
#43212 = CARTESIAN_POINT ( 'NONE',  ( 805.2837595273609850, -242.7363362996980811, -340.5290396650784714 ) ) ;
#43213 = CARTESIAN_POINT ( 'NONE',  ( 800.9747183278959710, -36.99823902205679360, 311.9810565676471583 ) ) ;
#43214 = CARTESIAN_POINT ( 'NONE',  ( 751.9810565676468741, -98.08914811296568814, 360.9747183278973921 ) ) ;
#43215 = PLANE ( 'NONE',  #31364 ) ;
#43216 = CYLINDRICAL_SURFACE ( 'NONE', #18056, 10.00000000000000888 ) ;
#43217 = CIRCLE ( 'NONE', #15217, 30.00000000000008171 ) ;
#43218 = CARTESIAN_POINT ( 'NONE',  ( 812.3518521366052028, -385.0999726633340856, 326.5853460496235243 ) ) ;
#43219 = LINE ( 'NONE', #39783, #6581 ) ;
#43220 = CARTESIAN_POINT ( 'NONE',  ( 810.7187646348534145, -354.4527844766012095, 356.7737145352016341 ) ) ;
#43221 = CARTESIAN_POINT ( 'NONE',  ( 762.3223304703356007, -319.5436935675104451, -322.3223304703362828 ) ) ;
#43222 = AXIS2_PLACEMENT_3D ( 'NONE', #29235, #7530, #35238 ) ;
#43223 = CARTESIAN_POINT ( 'NONE',  ( 779.9999999999992042, 126.4563064324884465, 350.0000000000000000 ) ) ;
#43224 = B_SPLINE_CURVE_WITH_KNOTS ( 'NONE', 3,
 ( #23520, #44559, #13379, #13157, #9228, #34387, #38097, #34140, #37622, #9903, #27006, #5974, #30704, #26760, #30932, #2757, #9458, #30234, #6203, #16852, #9677, #12919, #41550, #44326, #2511, #23301, #12681, #5759, #20295, #16616, #23975, #40640, #27236, #20065, #37403, #45026 ),
 .UNSPECIFIED., .F., .F.,
 ( 4, 2, 2, 2, 2, 2, 2, 2, 2, 2, 2, 2, 2, 2, 2, 2, 2, 4 ),
 ( 0.000000000000000000, 0.004405609005296106002, 0.008811218010592212005, 0.01101402251324022814, 0.01321682701588824428, 0.01762243602118459054, 0.01982524052383277668, 0.02202804502648095936, 0.02643365403177701245, 0.02863645853442487593, 0.03083926303707274288, 0.03194066528839652197, 0.03304206753972029759, 0.03359276866538235540, 0.03414346979104441321, 0.03469417091670646408, 0.03496952147953734380, 0.03524487204236821658 ),
 .UNSPECIFIED. ) ;
#43225 = CARTESIAN_POINT ( 'NONE',  ( 797.8594530101008786, -421.5436935675101040, 322.1405469898980982 ) ) ;
#43226 = CARTESIAN_POINT ( 'NONE',  ( 793.0897708529556667, -174.5545181178801784, 361.3366627262616362 ) ) ;
#43227 = CARTESIAN_POINT ( 'NONE',  ( 811.3240766477731540, -76.37269993606228979, -355.6651683502462902 ) ) ;
#43228 = CARTESIAN_POINT ( 'NONE',  ( 802.7791456095903868, -124.7146871989599930, -329.0155153010375102 ) ) ;
#43229 = CARTESIAN_POINT ( 'NONE',  ( 759.8311093483677041, -94.16923265350555994, 310.9282345327691814 ) ) ;
#43230 = CARTESIAN_POINT ( 'NONE',  ( 805.1927285166399315, -424.8164208402373561, 341.8018195045277707 ) ) ;
#43231 = CARTESIAN_POINT ( 'NONE',  ( 801.9858362298568863, -171.0783235625962106, 312.7379699480935642 ) ) ;
#43232 = CARTESIAN_POINT ( 'NONE',  ( 758.0580252608178853, -30.45278447660226817, -328.0187753319985404 ) ) ;
#43233 = CARTESIAN_POINT ( 'NONE',  ( 775.9200461376533440, -119.8055962898690865, -315.3028492785443291 ) ) ;
#43234 = CARTESIAN_POINT ( 'NONE',  ( 778.2165204200184689, -94.81642084023843609, -364.9363028652563230 ) ) ;
#43235 = CARTESIAN_POINT ( 'NONE',  ( 788.7631598425961101, 22.55804007376682918, -305.7194118038759143 ) ) ;
#43236 = EDGE_CURVE ( 'NONE', #20274, #38409, #4661, .T. ) ;
#43238 = CARTESIAN_POINT ( 'NONE',  ( 755.5713283507202505, -269.3618753856924286, 334.6858677611754729 ) ) ;
#43237 = CARTESIAN_POINT ( 'NONE',  ( 801.9419747391806368, -258.4527844766016074, 351.9812246680014027 ) ) ;
#43239 = DIRECTION ( 'NONE',  ( 0.000000000000000000, 0.000000000000000000, 1.000000000000000000 ) ) ;
#43240 = ORIENTED_EDGE ( 'NONE', *, *, #5490, .F. ) ;
#43241 = CARTESIAN_POINT ( 'NONE',  ( 769.1273215169530886, 25.28531280103955226, 317.4527132478988847 ) ) ;
#43242 = AXIS2_PLACEMENT_3D ( 'NONE', #43979, #26867, #12355 ) ;
#43243 = ORIENTED_EDGE ( 'NONE', *, *, #45621, .F. ) ;
#43244 = VECTOR ( 'NONE', #35932, 1000.000000000000000 ) ;
#43245 = CARTESIAN_POINT ( 'NONE',  ( 747.2067596250078623, -195.1800572038744974, 352.2312462859687230 ) ) ;
#43246 = CARTESIAN_POINT ( 'NONE',  ( 759.0159684113467620, -256.9181544815163534, 325.8855110935213020 ) ) ;
#43247 = ORIENTED_EDGE ( 'NONE', *, *, #44758, .T. ) ;
#43248 = CARTESIAN_POINT ( 'NONE',  ( 761.4292242960306112, -65.46360902697142592, -323.2154366446414429 ) ) ;
#43249 = CARTESIAN_POINT ( 'NONE',  ( 800.1688906516307043, -202.1692326535051905, 369.0717654672308186 ) ) ;
#43250 = CARTESIAN_POINT ( 'NONE',  ( 795.1360043628808398, -284.0891481129651197, -360.2193346964456282 ) ) ;
#43251 = VERTEX_POINT ( 'NONE', #16505 ) ;
#43252 = CARTESIAN_POINT ( 'NONE',  ( 800.2193346964447755, -402.9982390220555430, -355.1360043628815788 ) ) ;
#43253 = CARTESIAN_POINT ( 'NONE',  ( 792.1044303154645831, -36.45278447660223975, -317.8323909638837677 ) ) ;
#43254 = CARTESIAN_POINT ( 'NONE',  ( 766.7756240680305382, -254.5328690171413655, 361.5560724626415663 ) ) ;
#43255 = CARTESIAN_POINT ( 'NONE',  ( 999.9999999999992042, -599.0000000000001137, 359.0000000000000000 ) ) ;
#43256 = LINE ( 'NONE', #31934, #35355 ) ;
#43257 = CONICAL_SURFACE ( 'NONE', #16685, 8.024999999999948841, 0.7853981633974337351 ) ;
#43258 = CARTESIAN_POINT ( 'NONE',  ( 762.1177392798416577, -18.55451811788065797, -309.8865473780659272 ) ) ;
#43259 = DIRECTION ( 'NONE',  ( 1.000000000000000000, 4.625929269271485914E-16, 0.000000000000000000 ) ) ;
#43260 = EDGE_LOOP ( 'NONE', ( #23035, #40475 ) ) ;
#43261 = CARTESIAN_POINT ( 'NONE',  ( 814.8207195650702488, -314.1908817542433781, -336.2433038121456548 ) ) ;
#43262 = EDGE_CURVE ( 'NONE', #17108, #5117, #12803, .T. ) ;
#43264 = CARTESIAN_POINT ( 'NONE',  ( 802.1676090361156639, -254.6346026584196238, -327.8955696845344505 ) ) ;
#43263 = DIRECTION ( 'NONE',  ( 1.000000000000000000, 0.000000000000000000, 0.000000000000000000 ) ) ;
#43265 = CARTESIAN_POINT ( 'NONE',  ( 441.1634899080286232, 259.9999999999999432, -199.9999999999972431 ) ) ;
#43266 = CARTESIAN_POINT ( 'NONE',  ( 763.8424801807145741, -138.0090635724257311, -320.5453621957614700 ) ) ;
#43267 = EDGE_CURVE ( 'NONE', #31071, #8149, #31198, .T. ) ;
#43268 = CARTESIAN_POINT ( 'NONE',  ( 831.1634899080286232, 259.9999999999998863, -199.9999999999999432 ) ) ;
#43269 = CARTESIAN_POINT ( 'NONE',  ( 768.8385539511368734, -23.26014174441484883, -306.4236121716840557 ) ) ;
#43270 = CARTESIAN_POINT ( 'NONE',  ( 813.1304606946831655, -353.9073299311467053, -352.3570229623691716 ) ) ;
#43271 = CARTESIAN_POINT ( 'NONE',  ( 1007.605605532488426, -30.07539427629357576, 756.1153575698151599 ) ) ;
#43272 = CARTESIAN_POINT ( 'NONE',  ( 788.8264449731200330, -21.18005720387502677, 363.6646147819171233 ) ) ;
#43273 = AXIS2_PLACEMENT_3D ( 'NONE', #9045, #32868, #24666 ) ;
#43274 = CARTESIAN_POINT ( 'NONE',  ( 768.9521613784389729, -297.8272453906070041, 373.2346286133773106 ) ) ;
#43275 = CARTESIAN_POINT ( 'NONE',  ( 815.0009284576459549, -222.3510508353233206, -338.7629533639073429 ) ) ;
#43276 = CARTESIAN_POINT ( 'NONE',  ( 758.8095938919642549, -224.0891481129653187, 311.6929314249763365 ) ) ;
#43277 = CARTESIAN_POINT ( 'NONE',  ( 796.9462024416508257, 11.54721552339760038, -308.9653473494370246 ) ) ;
#43278 = AXIS2_PLACEMENT_3D ( 'NONE', #22507, #40744, #1490 ) ;
#43279 = CARTESIAN_POINT ( 'NONE',  ( 181.1634899080285948, 260.0000000000000000, -191.9749999999953900 ) ) ;
#43280 = ORIENTED_EDGE ( 'NONE', *, *, #2421, .F. ) ;
#43281 = CARTESIAN_POINT ( 'NONE',  ( 771.2633955100217236, -311.9073299311468759, 363.4237431249939618 ) ) ;
#43282 = VECTOR ( 'NONE', #28139, 1000.000000000000000 ) ;
#43283 = CARTESIAN_POINT ( 'NONE',  ( 780.5236548040995785, -92.73633629969860692, 314.9735926884559944 ) ) ;
#43284 = CARTESIAN_POINT ( 'NONE',  ( 795.9930595647434757, -27.07832356259665474, -320.7433823573372820 ) ) ;
#43285 = VECTOR ( 'NONE', #19674, 1000.000000000000000 ) ;
#43286 = LINE ( 'NONE', #21577, #19573 ) ;
#43287 = DIRECTION ( 'NONE',  ( 1.000000000000000000, 0.000000000000000000, -0.000000000000000000 ) ) ;
#43289 = CARTESIAN_POINT ( 'NONE',  ( 757.8323909638827445, -362.6346026584194533, 352.1044303154654358 ) ) ;
#43288 = CARTESIAN_POINT ( 'NONE',  ( 760.5453621957607311, -141.0783235625962959, 323.8424801807151425 ) ) ;
#43290 = VERTEX_POINT ( 'NONE', #37523 ) ;
#43291 = AXIS2_PLACEMENT_3D ( 'NONE', #29727, #44275, #12861 ) ;
#43292 = CARTESIAN_POINT ( 'NONE',  ( 802.7791456095903868, -292.7146871989594956, -329.0155153010375102 ) ) ;
#43293 = EDGE_CURVE ( 'NONE', #19543, #34761, #8894, .T. ) ;
#43294 = CARTESIAN_POINT ( 'NONE',  ( 756.3353852180819104, -149.9073299311473875, 331.1735550268788302 ) ) ;
#43295 = CARTESIAN_POINT ( 'NONE',  ( 801.9858362298568863, -315.0783235625957559, -312.7379699480935642 ) ) ;
#43296 = CARTESIAN_POINT ( 'NONE',  ( 779.9999999999992042, -452.9681489794448339, -339.9999999999999432 ) ) ;
#43297 = CARTESIAN_POINT ( 'NONE',  ( 795.6651683502461765, -442.7146871989589840, 371.3240766477733814 ) ) ;
#43298 = ORIENTED_EDGE ( 'NONE', *, *, #26419, .F. ) ;
#43299 = CARTESIAN_POINT ( 'NONE',  ( 771.1735550268778070, -321.1800572038740142, 316.3353852180827630 ) ) ;
#43300 = CARTESIAN_POINT ( 'NONE',  ( 770.0799878456142551, -85.98741447168738716, -362.9823548866085616 ) ) ;
#43301 = EDGE_LOOP ( 'NONE', ( #11880, #8240 ) ) ;
#43302 = CARTESIAN_POINT ( 'NONE',  ( 799.9999999999993179, 205.0000000000000568, -360.0000000000000000 ) ) ;
#43303 = CARTESIAN_POINT ( 'NONE',  ( 772.5602148656447525, -177.7255117493290868, -305.7998596910095443 ) ) ;
#43304 = ORIENTED_EDGE ( 'NONE', *, *, #33687, .T. ) ;
#43305 = CARTESIAN_POINT ( 'NONE',  ( 791.9812246680005501, -140.6346026584201070, -361.9419747391813189 ) ) ;
#43306 = ORIENTED_EDGE ( 'NONE', *, *, #33916, .F. ) ;
#43307 = CARTESIAN_POINT ( 'NONE',  ( 755.8894580844503253, -423.8272453906067199, -332.3691319403863531 ) ) ;
#43308 = EDGE_CURVE ( 'NONE', #14977, #28819, #41224, .T. ) ;
#43309 = CARTESIAN_POINT ( 'NONE',  ( 765.0180583372156207, -0.9982390220569063999, 360.0135310231089534 ) ) ;
#43310 = CARTESIAN_POINT ( 'NONE',  ( 789.9200121543843807, -169.9874144716871172, 317.0176451133914384 ) ) ;
#43311 = CIRCLE ( 'NONE', #2730, 10.00000000000000888 ) ;
#43314 = CARTESIAN_POINT ( 'NONE',  ( 813.2346286133761168, -413.2601417444136018, 328.9521613784389160 ) ) ;
#43313 = CARTESIAN_POINT ( 'NONE',  ( 799.9999999999993179, -365.3551492539851893, 8.132432514707076621 ) ) ;
#43312 = DIRECTION ( 'NONE',  ( -0.000000000000000000, 0.000000000000000000, 1.000000000000000000 ) ) ;
#43315 = EDGE_CURVE ( 'NONE', #4330, #12054, #44687, .T. ) ;
#43316 = EDGE_LOOP ( 'NONE', ( #10922, #17582 ) ) ;
#43317 = CARTESIAN_POINT ( 'NONE',  ( 802.9823548866075953, -409.0999726633340288, -330.0799878456151077 ) ) ;
#43318 = CARTESIAN_POINT ( 'NONE',  ( 51.16348990802859475, 260.0000000000000568, -197.2499999999946851 ) ) ;
#43319 = CARTESIAN_POINT ( 'NONE',  ( 793.5525998758768083, -199.0999726633346825, -372.6845335610516941 ) ) ;
#43320 = CARTESIAN_POINT ( 'NONE',  ( 750.9282345327678740, -64.91815448151686496, 319.8311093483690115 ) ) ;
#43321 = CIRCLE ( 'NONE', #41873, 2.749999999999919176 ) ;
#43323 = FACE_OUTER_BOUND ( 'NONE', #37544, .T. ) ;
#43322 = DIRECTION ( 'NONE',  ( 0.000000000000000000, 0.000000000000000000, 1.000000000000000000 ) ) ;
#43324 = CARTESIAN_POINT ( 'NONE',  ( 786.6156483768007774, -337.4419599262319593, -315.5913626894246136 ) ) ;
#43325 = CARTESIAN_POINT ( 'NONE',  ( 879.9999999999992042, 99.99999999999984368, 360.0000000000000000 ) ) ;
#43326 = CARTESIAN_POINT ( 'NONE',  ( 757.7880784355613741, -186.0090635724255890, -312.4576283171834916 ) ) ;
#43327 = FACE_BOUND ( 'NONE', #32625, .T. ) ;
#43328 = DIRECTION ( 'NONE',  ( -0.000000000000000000, 1.000000000000000000, -0.000000000000000000 ) ) ;
#43329 = AXIS2_PLACEMENT_3D ( 'NONE', #5188, #33362, #1493 ) ;
#43330 = EDGE_CURVE ( 'NONE', #44486, #11392, #20191, .T. ) ;
#43331 = CARTESIAN_POINT ( 'NONE',  ( 772.4468031744293057, -393.8272453906067199, 363.8651313633793620 ) ) ;
#43332 = CARTESIAN_POINT ( 'NONE',  ( 767.6429770376291799, -249.1800572038742700, -306.8695393053162093 ) ) ;
#43333 = DIRECTION ( 'NONE',  ( 1.000000000000000000, -0.000000000000000000, -0.000000000000000000 ) ) ;
#43334 = CARTESIAN_POINT ( 'NONE',  ( 778.2165204200184689, 1.183579159761269040, -364.9363028652563230 ) ) ;
#43335 = CARTESIAN_POINT ( 'NONE',  ( 750.9282345327678740, -184.9181544815165239, 319.8311093483690115 ) ) ;
#43336 = CARTESIAN_POINT ( 'NONE',  ( 746.7653713866222915, -137.2601417444144829, -351.0478386215610271 ) ) ;
#43337 = CARTESIAN_POINT ( 'NONE',  ( 814.9108240113580450, -136.2709662947837330, 337.5031285880265273 ) ) ;
#43338 = CARTESIAN_POINT ( 'NONE',  ( 772.5602148656447525, -369.7255117493284615, -305.7998596910095443 ) ) ;
#43339 = DIRECTION ( 'NONE',  ( 0.000000000000000000, 1.000000000000000000, -0.000000000000000000 ) ) ;
#43340 = LINE ( 'NONE', #39205, #12423 ) ;
#43341 = CARTESIAN_POINT ( 'NONE',  ( 804.4286716492782716, -233.3618753856925423, 345.3141322388244703 ) ) ;
#43342 = CARTESIAN_POINT ( 'NONE',  ( 796.1575198192839480, -30.00906357242607925, 359.4546378042384163 ) ) ;
#43343 = EDGE_CURVE ( 'NONE', #27904, #30052, #5882, .T. ) ;
#43344 = CARTESIAN_POINT ( 'NONE',  ( 776.2433038121456548, -420.8965053807772279, -374.8207195650711014 ) ) ;
#43345 = CARTESIAN_POINT ( 'NONE',  ( 795.8262568251477660, 1.627300063937458408, -308.3538107759623585 ) ) ;
#43347 = EDGE_CURVE ( 'NONE', #21916, #38320, #9799, .T. ) ;
#43346 = DIRECTION ( 'NONE',  ( 0.000000000000000000, 0.000000000000000000, 1.000000000000000000 ) ) ;
#43348 = CARTESIAN_POINT ( 'NONE',  ( 812.6845335610512393, -31.98741447168754348, 353.5525998758768651 ) ) ;
#43349 = ORIENTED_EDGE ( 'NONE', *, *, #8252, .F. ) ;
#43350 = CARTESIAN_POINT ( 'NONE',  ( 790.8726784830453198, -202.7146871989597514, -362.5472867521010585 ) ) ;
#43351 = CARTESIAN_POINT ( 'NONE',  ( 755.0636971347428243, -28.27096629478409540, 341.7834795799807353 ) ) ;
#43352 = CARTESIAN_POINT ( 'NONE',  ( 805.9055244015594326, -219.6237781080506295, -315.8990559732753240 ) ) ;
#43353 = CARTESIAN_POINT ( 'NONE',  ( 751.2241431872005251, -328.1692326535048210, 359.9636004259367610 ) ) ;
#43354 = CARTESIAN_POINT ( 'NONE',  ( 771.2633955100217236, -167.9073299311473022, 363.4237431249939618 ) ) ;
#43355 = CARTESIAN_POINT ( 'NONE',  ( 792.1044303154645831, -84.45278447660206211, -317.8323909638837677 ) ) ;
#43356 = ORIENTED_EDGE ( 'NONE', *, *, #4722, .F. ) ;
#43357 = AXIS2_PLACEMENT_3D ( 'NONE', #4892, #30269, #12499 ) ;
#43358 = CARTESIAN_POINT ( 'NONE',  ( 788.7631598425961101, -433.4419599262316183, 305.7194118038759143 ) ) ;
#43359 = CARTESIAN_POINT ( 'NONE',  ( 754.8072714833581358, -148.8164208402382656, -338.1981804954720587 ) ) ;
#43360 = CARTESIAN_POINT ( 'NONE',  ( 800.0135310231082713, -326.0891481129649492, 325.0180583372163028 ) ) ;
#43361 = CARTESIAN_POINT ( 'NONE',  ( 787.4397851343537695, -45.72551174932949181, -374.2001403089903988 ) ) ;
#43362 = EDGE_CURVE ( 'NONE', #16032, #17925, #19744, .T. ) ;
#43363 = ORIENTED_EDGE ( 'NONE', *, *, #16308, .F. ) ;
#43364 = CARTESIAN_POINT ( 'NONE',  ( 754.3581564841646241, -449.4636090269702322, -316.1443688327762516 ) ) ;
#43365 = ORIENTED_EDGE ( 'NONE', *, *, #16194, .T. ) ;
#43366 = CARTESIAN_POINT ( 'NONE',  ( 763.0428371773158460, -323.4636090269706301, -358.7617431975195359 ) ) ;
#43367 = EDGE_CURVE ( 'NONE', #38472, #5383, #32698, .T. ) ;
#43369 = CARTESIAN_POINT ( 'NONE',  ( 790.9844846989617508, -382.3726999360613945, 317.2208543904092721 ) ) ;
#43368 = CARTESIAN_POINT ( 'NONE',  ( 759.7806653035534055, -54.99823902205672255, 324.8639956371180801 ) ) ;
#43370 = CARTESIAN_POINT ( 'NONE',  ( 757.8323909638827445, -290.6346026584195101, -352.1044303154654358 ) ) ;
#43371 = CARTESIAN_POINT ( 'NONE',  ( 754.9967657858570647, -409.5436935675101608, 365.0032342141425943 ) ) ;
#43372 = EDGE_CURVE ( 'NONE', #463, #38191, #12756, .T. ) ;
#43373 = CARTESIAN_POINT ( 'NONE',  ( 773.7943932421234194, -95.80559628986917176, 305.5313806188329409 ) ) ;
#43374 = CARTESIAN_POINT ( 'NONE',  ( 769.9779781133707957, -283.0999726633344267, -316.7813123517150871 ) ) ;
#43375 = CARTESIAN_POINT ( 'NONE',  ( 755.5713283507202505, -293.3618753856923718, -334.6858677611754729 ) ) ;
#43376 = CARTESIAN_POINT ( 'NONE',  ( 756.5762568750052424, -147.1800572038746395, -348.7366044899774238 ) ) ;
#43377 = DIRECTION ( 'NONE',  ( -0.000000000000000000, -0.3826834323650836756, -0.9238795325112892920 ) ) ;
#43378 = CARTESIAN_POINT ( 'NONE',  ( 812.7932403749906598, -423.1800572038737300, 327.7687537140311633 ) ) ;
#43380 = LINE ( 'NONE', #25814, #17480 ) ;
#43379 = DIRECTION ( 'NONE',  ( -0.000000000000000000, -1.000000000000000000, -0.000000000000000000 ) ) ;
#43381 = CARTESIAN_POINT ( 'NONE',  ( 813.5763878283155464, -99.82724539060768620, -351.1614460488615350 ) ) ;
#43382 = LINE ( 'NONE', #11750, #25615 ) ;
#43384 = EDGE_CURVE ( 'NONE', #11148, #39743, #26885, .T. ) ;
#43383 = DIRECTION ( 'NONE',  ( 5.551115123125783688E-16, -1.000000000000000000, 0.000000000000000000 ) ) ;
#43385 = CARTESIAN_POINT ( 'NONE',  ( 766.9102291470427417, -306.5545181178797520, 318.6633372737382501 ) ) ;
#43386 = CARTESIAN_POINT ( 'NONE',  ( 803.6646147819161570, -137.9073299311473875, 348.8264449731210561 ) ) ;
#43387 = ORIENTED_EDGE ( 'NONE', *, *, #12538, .F. ) ;
#43388 = CARTESIAN_POINT ( 'NONE',  ( 751.9810565676468741, -146.0891481129655176, -360.9747183278973921 ) ) ;
#43389 = CARTESIAN_POINT ( 'NONE',  ( 790.8726784830453198, -322.7146871989593819, 362.5472867521010585 ) ) ;
#43390 = VECTOR ( 'NONE', #23936, 1000.000000000000000 ) ;
#43391 = DIRECTION ( 'NONE',  ( 1.000000000000000000, 0.000000000000000000, 0.000000000000000000 ) ) ;
#43392 = CARTESIAN_POINT ( 'NONE',  ( 750.9282345327678740, -64.91815448151686496, 319.8311093483690115 ) ) ;
#43393 = CARTESIAN_POINT ( 'NONE',  ( 762.1405469898971887, -193.5436935675108714, 357.8594530101015607 ) ) ;
#43394 = CARTESIAN_POINT ( 'NONE',  ( 787.4397851343537695, -261.7255117493288026, -374.2001403089903988 ) ) ;
#43395 = CARTESIAN_POINT ( 'NONE',  ( 749.2812353651451076, -198.4527844766017495, 323.2262854647983090 ) ) ;
#43396 = CARTESIAN_POINT ( 'NONE',  ( 764.8639956371174549, -128.0891481129655176, 319.7806653035542013 ) ) ;
#43397 = PRESENTATION_STYLE_ASSIGNMENT (( #29323 ) ) ;
#43398 = CARTESIAN_POINT ( 'NONE',  ( 798.0661480581538854, -290.5328690171412518, -309.5768839229118043 ) ) ;
#43399 = CARTESIAN_POINT ( 'NONE',  ( 783.0745993439762742, -8.190881754244330182, 365.1016975059196739 ) ) ;
#43400 = CARTESIAN_POINT ( 'NONE',  ( 751.9810565676468741, -338.0891481129649492, -360.9747183278973921 ) ) ;
#43401 = CARTESIAN_POINT ( 'NONE',  ( 311.1634899080286232, 256.5000000000000000, -199.9999999999963336 ) ) ;
#43402 = CARTESIAN_POINT ( 'NONE',  ( 805.0264073115434940, -390.3510508353227237, 339.4763451958999099 ) ) ;
#43403 = ORIENTED_EDGE ( 'NONE', *, *, #11150, .F. ) ;
#43404 = CARTESIAN_POINT ( 'NONE',  ( 774.6312213355099630, -407.3618753856920307, -364.6798772138717482 ) ) ;
#43405 = CARTESIAN_POINT ( 'NONE',  ( 811.6461892240364477, -100.7146871989600356, -324.1737431748509835 ) ) ;
#43406 = CARTESIAN_POINT ( 'NONE',  ( -26.63011601220122060, -496.5085659523897448, -356.8883017825714319 ) ) ;
#43407 = CARTESIAN_POINT ( 'NONE',  ( 800.1688906516307043, -226.1692326535051052, 369.0717654672308186 ) ) ;
#43408 = CARTESIAN_POINT ( 'NONE',  ( 762.1405469898973024, -49.54369356751129772, 357.8594530101016176 ) ) ;
#43409 = CARTESIAN_POINT ( 'NONE',  ( 801.3366627262608972, -224.5328690171415076, -353.0897708529566899 ) ) ;
#43410 = CARTESIAN_POINT ( 'NONE',  ( 801.9419747391806368, -234.4527844766016358, 351.9812246680014027 ) ) ;
#43411 = CARTESIAN_POINT ( 'NONE',  ( 768.8385539511368734, -71.26014174441469606, -306.4236121716840557 ) ) ;
#43412 = CARTESIAN_POINT ( 'NONE',  ( 804.5667330414263461, -452.9681489794450044, -348.7981942340067576 ) ) ;
#43413 = ORIENTED_EDGE ( 'NONE', *, *, #11931, .T. ) ;
#43414 = EDGE_LOOP ( 'NONE', ( #65, #1989 ) ) ;
#43415 = CARTESIAN_POINT ( 'NONE',  ( 773.7305795820266212, -345.2817908451523863, -374.8230680027170365 ) ) ;
#43416 = AXIS2_PLACEMENT_3D ( 'NONE', #15399, #29480, #43552 ) ;
#43417 = CARTESIAN_POINT ( 'NONE',  ( 751.9810565676468741, -290.0891481129650629, 360.9747183278973921 ) ) ;
#43418 = CARTESIAN_POINT ( 'NONE',  ( 764.3348316497523456, -46.71468719896022748, 308.6759233522265617 ) ) ;
#43419 = CARTESIAN_POINT ( 'NONE',  ( 802.9823548866075953, -169.0999726633347393, -330.0799878456151077 ) ) ;
#43420 = CARTESIAN_POINT ( 'NONE',  ( 781.8018195045266339, -190.2709662947835909, -365.1927285166406705 ) ) ;
#43421 = CARTESIAN_POINT ( 'NONE',  ( 756.5762568750052424, -387.1800572038738437, -348.7366044899774238 ) ) ;
#43422 = ORIENTED_EDGE ( 'NONE', *, *, #35409, .F. ) ;
#43423 = CARTESIAN_POINT ( 'NONE',  ( 794.1144889064781864, 13.83076734649413098, -360.9840315886528401 ) ) ;
#43424 = EDGE_LOOP ( 'NONE', ( #5487, #42285 ) ) ;
#43425 = CARTESIAN_POINT ( 'NONE',  ( 782.4968714119720516, -322.8164208402377540, 305.0891759886411023 ) ) ;
#43426 = DIRECTION ( 'NONE',  ( 0.000000000000000000, 0.000000000000000000, 1.000000000000000000 ) ) ;
#43427 = LINE ( 'NONE', #18721, #6902 ) ;
#43428 = CARTESIAN_POINT ( 'NONE',  ( 790.0220218866281812, -199.0999726633346825, 363.2186876482849129 ) ) ;
#43429 = CARTESIAN_POINT ( 'NONE',  ( 758.0580252608178853, -54.45278447660219001, 328.0187753319985404 ) ) ;
#43430 = ORIENTED_EDGE ( 'NONE', *, *, #24477, .F. ) ;
#43431 = CARTESIAN_POINT ( 'NONE',  ( 744.6391490659812007, -422.7363362996975980, -338.7502325331110455 ) ) ;
#43432 = CARTESIAN_POINT ( 'NONE',  ( 746.8695393053151292, -29.90732993114772142, -327.6429770376306578 ) ) ;
#43433 = CARTESIAN_POINT ( 'NONE',  ( 805.1016975059191054, -222.8965053807778531, 343.0745993439771837 ) ) ;
#43434 = CARTESIAN_POINT ( 'NONE',  ( 756.5762568750052424, -387.1800572038738437, -348.7366044899774238 ) ) ;
#43435 = CARTESIAN_POINT ( 'NONE',  ( 804.4286716492782716, 6.638124614306706306, -345.3141322388244703 ) ) ;
#43436 = CARTESIAN_POINT ( 'NONE',  ( 745.7998596910086917, -437.3618753856919170, 332.5602148656461168 ) ) ;
#43437 = DIRECTION ( 'NONE',  ( 0.000000000000000000, 1.000000000000000000, -0.000000000000000000 ) ) ;
#43438 = CARTESIAN_POINT ( 'NONE',  ( 754.7162404726377645, -254.7363362996981095, -339.4709603349214717 ) ) ;
#43439 = CARTESIAN_POINT ( 'NONE',  ( 777.5031285880264704, -166.8164208402382087, -374.9108240113588408 ) ) ;
#43440 = CARTESIAN_POINT ( 'NONE',  ( 763.2262854647970016, -56.63460265842036279, 309.2812353651462445 ) ) ;
#43441 = CARTESIAN_POINT ( 'NONE',  ( 814.5518280994195948, -111.7255117493293000, 332.4837098697145734 ) ) ;
#43442 = CARTESIAN_POINT ( 'NONE',  ( 772.8365271371600329, 16.45630643248849267, -315.6518837687410723 ) ) ;
#43443 = LINE ( 'NONE', #266, #10661 ) ;
#43444 = VECTOR ( 'NONE', #29136, 1000.000000000000000 ) ;
#43445 = CARTESIAN_POINT ( 'NONE',  ( 810.4231160770870019, -384.5545181178795247, 321.9338519418446936 ) ) ;
#43446 = DIRECTION ( 'NONE',  ( -1.000000000000000000, 0.000000000000000000, 0.000000000000000000 ) ) ;
#43447 = CARTESIAN_POINT ( 'NONE',  ( 814.2001403089898304, -353.3618753856922012, 347.4397851343538264 ) ) ;
#43448 = CARTESIAN_POINT ( 'NONE',  ( 785.3141322388236176, -309.7255117493287457, -364.4286716492789537 ) ) ;
#43449 = CARTESIAN_POINT ( 'NONE',  ( 783.0433043558608688, -0.8965053807785533513, 315.1538015810313027 ) ) ;
#43450 = CARTESIAN_POINT ( 'NONE',  ( 773.4516893846965786, -187.6454272087892434, 315.8398074228977066 ) ) ;
#43451 = CARTESIAN_POINT ( 'NONE',  ( 814.2805881961230625, -49.64542720878965554, -331.2368401574024119 ) ) ;
#43452 = CARTESIAN_POINT ( 'NONE',  ( 765.8855110935204493, -118.1692326535054463, -319.0159684113471599 ) ) ;
#43453 = CARTESIAN_POINT ( 'NONE',  ( 798.0661480581538854, -122.5328690171417918, 309.5768839229118043 ) ) ;
#43454 = CARTESIAN_POINT ( 'NONE',  ( 800.0135310231082713, -446.0891481129646081, 325.0180583372163028 ) ) ;
#43455 = CARTESIAN_POINT ( 'NONE',  ( 803.6646147819161570, -17.90732993114776406, -348.8264449731210561 ) ) ;
#43456 = CARTESIAN_POINT ( 'NONE',  ( 794.1144889064781864, -130.1692326535054463, -360.9840315886528401 ) ) ;
#43457 = CARTESIAN_POINT ( 'NONE',  ( 797.6776695296629214, -139.5436935675110135, -357.6776695296636603 ) ) ;
#43458 = CARTESIAN_POINT ( 'NONE',  ( 783.0433043558608688, -432.8965053807771142, -315.1538015810313027 ) ) ;
#43460 = CARTESIAN_POINT ( 'NONE',  ( 800.0135310231082713, -254.0891481129652334, 325.0180583372163028 ) ) ;
#43459 = CARTESIAN_POINT ( 'NONE',  ( 768.0187753319979720, -248.6346026584197659, 318.0580252608186242 ) ) ;
#43461 = DIRECTION ( 'NONE',  ( 1.000000000000000000, 0.000000000000000000, -0.000000000000000000 ) ) ;
#43462 = ORIENTED_EDGE ( 'NONE', *, *, #9440, .F. ) ;
#43463 = CARTESIAN_POINT ( 'NONE',  ( 773.3843516231979720, 10.55804007376686826, 364.4086373105754433 ) ) ;
#43464 = ORIENTED_EDGE ( 'NONE', *, *, #9214, .F. ) ;
#43465 = CARTESIAN_POINT ( 'NONE',  ( 744.7301800767020268, -196.8164208402380950, 337.4774526936615189 ) ) ;
#43466 = CARTESIAN_POINT ( 'NONE',  ( 755.1538015810308480, -254.1908817542435770, 343.0433043558613804 ) ) ;
#43467 = CARTESIAN_POINT ( 'NONE',  ( 795.9930595647434757, -387.0783235625955285, 320.7433823573372820 ) ) ;
#43468 = ORIENTED_EDGE ( 'NONE', *, *, #45636, .T. ) ;
#43469 = CARTESIAN_POINT ( 'NONE',  ( 793.9708237608222134, -94.91815448151677970, -319.2295555964448681 ) ) ;
#43470 = CARTESIAN_POINT ( 'NONE',  ( 812.6845335610512393, -223.9874144716869182, 353.5525998758768651 ) ) ;
#43471 = CARTESIAN_POINT ( 'NONE',  ( 759.9864689768902508, -290.0891481129650629, -354.9819416627836404 ) ) ;
#43472 = ORIENTED_EDGE ( 'NONE', *, *, #29773, .T. ) ;
#43473 = CARTESIAN_POINT ( 'NONE',  ( 774.6312213355099630, -407.3618753856920307, -364.6798772138717482 ) ) ;
#43474 = CARTESIAN_POINT ( 'NONE',  ( 804.4286716492782716, -65.36187538569306810, -345.3141322388244703 ) ) ;
#43475 = CARTESIAN_POINT ( 'NONE',  ( 763.2154366446407039, -261.6237781080504305, 321.4292242960311228 ) ) ;
#43476 = CARTESIAN_POINT ( 'NONE',  ( -338.8365100919713200, 258.0940000000001078, -193.8809999999918148 ) ) ;
#43477 = CYLINDRICAL_SURFACE ( 'NONE', #12331, 10.00000000000000888 ) ;
#43478 = CARTESIAN_POINT ( 'NONE',  ( 809.0717654672305343, -28.91815448151699286, -360.1688906516309885 ) ) ;
#43479 = CARTESIAN_POINT ( 'NONE',  ( -37.63011601220122770, -563.3203001761230553, -342.3463313526983143 ) ) ;
#43480 = ORIENTED_EDGE ( 'NONE', *, *, #14757, .F. ) ;
#43481 = CARTESIAN_POINT ( 'NONE',  ( 783.7953271457878373, -320.1908817542434349, -375.1787889125761239 ) ) ;
#43482 = CARTESIAN_POINT ( 'NONE',  ( 783.7953271457878373, -176.1908817542438328, 375.1787889125761239 ) ) ;
#43484 = CARTESIAN_POINT ( 'NONE',  ( 755.0636971347428243, -292.2709662947831930, -341.7834795799807353 ) ) ;
#43483 = LINE ( 'NONE', #22456, #11374 ) ;
#43485 = CARTESIAN_POINT ( 'NONE',  ( -769.9999999999992042, 205.0000000000000568, -319.9999999999999432 ) ) ;
#43486 = CARTESIAN_POINT ( 'NONE',  ( 763.0428371773158460, -155.4636090269711417, -358.7617431975195359 ) ) ;
#43487 = APPLICATION_CONTEXT ( 'automotive_design' ) ;
#43488 = CARTESIAN_POINT ( 'NONE',  ( 800.9747183278959710, -12.99823902205686821, 311.9810565676471583 ) ) ;
#43489 = DIRECTION ( 'NONE',  ( -0.000000000000000000, 1.000000000000000000, -0.000000000000000000 ) ) ;
#43490 = CARTESIAN_POINT ( 'NONE',  ( 745.0891759886404770, -364.2709662947830793, -342.4968714119734159 ) ) ;
#43491 = CARTESIAN_POINT ( 'NONE',  ( 311.1634899080286232, 256.5000000000000000, -199.9999999999963336 ) ) ;
#43492 = CARTESIAN_POINT ( 'NONE',  ( 788.7366044899766848, -35.90732993114770011, 316.5762568750059813 ) ) ;
#43493 = CARTESIAN_POINT ( 'NONE',  ( 795.8262568251477660, -286.3726999360617356, 308.3538107759623585 ) ) ;
#43494 = CARTESIAN_POINT ( 'NONE',  ( 813.9316612368132837, -223.4419599262323857, -348.6739635108323228 ) ) ;
#43495 = CARTESIAN_POINT ( 'NONE',  ( 811.0346526505616112, -254.6346026584196238, 323.0537975583477532 ) ) ;
#43496 = CARTESIAN_POINT ( 'NONE',  ( 814.9108240113580450, 7.729033705215793582, -337.5031285880265273 ) ) ;
#43497 = DIRECTION ( 'NONE',  ( 0.000000000000000000, -0.000000000000000000, -1.000000000000000000 ) ) ;
#43498 = ORIENTED_EDGE ( 'NONE', *, *, #24740, .T. ) ;
#43499 = CARTESIAN_POINT ( 'NONE',  ( 757.8323909638827445, -338.6346026584195101, 352.1044303154654358 ) ) ;
#43500 = CARTESIAN_POINT ( 'NONE',  ( 796.1575198192839480, -102.0090635724258448, 359.4546378042384163 ) ) ;
#43501 = CARTESIAN_POINT ( 'NONE',  ( 803.8651313633788504, -29.26014174441482751, -332.4468031744301015 ) ) ;
#43502 = CARTESIAN_POINT ( 'NONE',  ( 919.9999999999993179, 219.9999999999998863, 350.0000000000000000 ) ) ;
#43503 = DIRECTION ( 'NONE',  ( -1.000000000000000000, 0.000000000000000000, -0.000000000000000000 ) ) ;
#43504 = CARTESIAN_POINT ( 'NONE',  ( 758.0141637701419768, -135.0783235625962959, 367.2620300519063790 ) ) ;
#43505 = CARTESIAN_POINT ( 'NONE',  ( 755.3201227861273992, -387.7255117493283478, 345.3687786644892981 ) ) ;
#43506 = ORIENTED_EDGE ( 'NONE', *, *, #41678, .T. ) ;
#43507 = CARTESIAN_POINT ( 'NONE',  ( 755.0488828828309806, -329.8055962898683902, -344.1219089521771934 ) ) ;
#43508 = CARTESIAN_POINT ( 'NONE',  ( 785.3141322388236176, -165.7255117493291152, 364.4286716492789537 ) ) ;
#43509 = UNCERTAINTY_MEASURE_WITH_UNIT (LENGTH_MEASURE( 1.000000000000000082E-05 ), #24063, 'distance_accuracy_value', 'NONE');
#43510 = CARTESIAN_POINT ( 'NONE',  ( 759.8311093483677041, -334.1692326535047073, -310.9282345327691814 ) ) ;
#43511 = CARTESIAN_POINT ( 'NONE',  ( 441.1634899080286232, 229.9999999999999716, -202.7499999999971010 ) ) ;
#43512 = CARTESIAN_POINT ( 'NONE',  ( 792.2269492836462632, -443.1233509495419298, 372.8191558162650949 ) ) ;
#43513 = ADVANCED_FACE ( 'NONE', ( #19971 ), #15038, .F. ) ;
#43514 = ORIENTED_EDGE ( 'NONE', *, *, #30379, .T. ) ;
#43515 = CARTESIAN_POINT ( 'NONE',  ( 768.0187753319979720, -368.6346026584193964, 318.0580252608186242 ) ) ;
#43516 = ORIENTED_EDGE ( 'NONE', *, *, #13436, .T. ) ;
#43517 = LINE ( 'NONE', #43302, #6196 ) ;
#43518 = EDGE_CURVE ( 'NONE', #40312, #16670, #20863, .T. ) ;
#43519 = CARTESIAN_POINT ( 'NONE',  ( 746.8695393053150156, -173.9073299311472169, -327.6429770376306010 ) ) ;
#43520 = ORIENTED_EDGE ( 'NONE', *, *, #21050, .F. ) ;
#43521 = CARTESIAN_POINT ( 'NONE',  ( 757.8323909638828582, -170.6346026584199933, -352.1044303154654358 ) ) ;
#43522 = EDGE_LOOP ( 'NONE', ( #9710, #27437, #25240, #7251 ) ) ;
#43523 = CARTESIAN_POINT ( 'NONE',  ( 802.9823548866075953, -433.0999726633339151, -330.0799878456151077 ) ) ;
#43524 = CARTESIAN_POINT ( 'NONE',  ( 804.8461984189677878, -458.1908817542429802, 336.9566956441385628 ) ) ;
#43525 = CARTESIAN_POINT ( 'NONE',  ( 751.9810565676468741, -218.0891481129653187, 360.9747183278973921 ) ) ;
#43526 = CARTESIAN_POINT ( 'NONE',  ( 789.9200121543843807, -145.9874144716871740, 317.0176451133914384 ) ) ;
#43528 = LINE ( 'NONE', #25966, #18170 ) ;
#43527 = DIRECTION ( 'NONE',  ( -0.000000000000000000, 1.000000000000000000, -0.000000000000000000 ) ) ;
#43529 = ORIENTED_EDGE ( 'NONE', *, *, #7822, .F. ) ;
#43530 = CARTESIAN_POINT ( 'NONE',  ( 761.4292242960306112, -425.4636090269703459, -323.2154366446414429 ) ) ;
#43531 = CARTESIAN_POINT ( 'NONE',  ( 772.4999999999993179, -462.9681489794447202, -270.0000000000000568 ) ) ;
#43532 = CARTESIAN_POINT ( 'NONE',  ( 811.3240766477731540, -220.3726999360618208, -355.6651683502462902 ) ) ;
#43533 = CARTESIAN_POINT ( 'NONE',  ( 813.5763878283155464, -75.82724539060775726, 351.1614460488615350 ) ) ;
#43535 = PLANE ( 'NONE',  #43958 ) ;
#43534 = DIRECTION ( 'NONE',  ( 8.326672684688676025E-16, -1.000000000000000000, 0.000000000000000000 ) ) ;
#43536 = CARTESIAN_POINT ( 'NONE',  ( 805.0264073115434940, -318.3510508353230080, -339.4763451958999099 ) ) ;
#43537 = DIRECTION ( 'NONE',  ( -1.000000000000000000, 0.000000000000000000, -0.000000000000000000 ) ) ;
#43538 = CARTESIAN_POINT ( 'NONE',  ( 791.0478386215596629, -213.8272453906073167, -306.7653713866226326 ) ) ;
#43539 = CARTESIAN_POINT ( 'NONE',  ( 939.9999999999992042, -184.9457194955397767, 62.92409052808234549 ) ) ;
#43540 = DIRECTION ( 'NONE',  ( 1.000000000000000000, 0.000000000000000000, 0.000000000000000000 ) ) ;
#43541 = CARTESIAN_POINT ( 'NONE',  ( 755.1538015810308480, -398.1908817542431507, 343.0433043558613804 ) ) ;
#43542 = ADVANCED_FACE ( 'NONE', ( #42127 ), #17429, .F. ) ;
#43543 = CARTESIAN_POINT ( 'NONE',  ( 745.7998596910086917, -245.3618753856925139, -332.5602148656461168 ) ) ;
#43544 = CARTESIAN_POINT ( 'NONE',  ( 790.9844846989617508, -238.3726999360617640, 317.2208543904092721 ) ) ;
#43545 = CARTESIAN_POINT ( 'NONE',  ( 928.0249999999991815, 219.9999999999998863, -360.0000000000000000 ) ) ;
#43546 = CARTESIAN_POINT ( 'NONE',  ( 785.3687786644884454, -11.36187538569323863, -315.3201227861279676 ) ) ;
#43547 = CARTESIAN_POINT ( 'NONE',  ( 762.1177392798416577, -186.5545181178801215, 309.8865473780659272 ) ) ;
#43548 = CARTESIAN_POINT ( 'NONE',  ( 800.1688906516307043, -130.1692326535054463, -369.0717654672308186 ) ) ;
#43549 = CARTESIAN_POINT ( 'NONE',  ( 814.2001403089898304, -161.3618753856927697, 347.4397851343538264 ) ) ;
#43550 = CARTESIAN_POINT ( 'NONE',  ( 749.2812353651451076, -366.4527844766012095, -323.2262854647983090 ) ) ;
#43551 = FACE_OUTER_BOUND ( 'NONE', #39970, .T. ) ;
#43552 = DIRECTION ( 'NONE',  ( 0.000000000000000000, 0.000000000000000000, 1.000000000000000000 ) ) ;
#43553 = CARTESIAN_POINT ( 'NONE',  ( 803.4237431249931660, -207.1800572038744406, 331.2633955100225194 ) ) ;
#43554 = CARTESIAN_POINT ( 'NONE',  ( 793.0897708529556667, -30.55451811788062244, 361.3366627262616362 ) ) ;
#43555 = CARTESIAN_POINT ( 'NONE',  ( 785.3141322388236176, -381.7255117493284615, -364.4286716492789537 ) ) ;
#43556 = CARTESIAN_POINT ( 'NONE',  ( 766.4474001241216001, 4.900027336664720679, -307.3154664389482491 ) ) ;
#43557 = DIRECTION ( 'NONE',  ( -0.000000000000000000, -0.000000000000000000, 1.000000000000000000 ) ) ;
#43558 = CARTESIAN_POINT ( 'NONE',  ( 751.2241431872005251, -40.16923265350570915, 359.9636004259367610 ) ) ;
#43559 = ORIENTED_EDGE ( 'NONE', *, *, #31734, .T. ) ;
#43560 = ADVANCED_FACE ( 'NONE', ( #27575 ), #28895, .F. ) ;
#43561 = CARTESIAN_POINT ( 'NONE',  ( 754.8983024940795303, -210.8965053807778816, -336.9254006560228163 ) ) ;
#43562 = CARTESIAN_POINT ( 'NONE',  ( 758.0580252608178853, -30.45278447660226817, 328.0187753319985404 ) ) ;
#43563 = CARTESIAN_POINT ( 'NONE',  ( 764.3348316497523456, -238.7146871989596661, -308.6759233522265617 ) ) ;
#43564 = DIRECTION ( 'NONE',  ( 0.000000000000000000, 0.000000000000000000, 1.000000000000000000 ) ) ;
#43565 = CARTESIAN_POINT ( 'NONE',  ( 746.0683387631852383, -331.4419599262320162, 331.3260364891676204 ) ) ;
#43566 = EDGE_LOOP ( 'NONE', ( #44299, #19484, #28659, #45536, #8199 ) ) ;
#43567 = CARTESIAN_POINT ( 'NONE',  ( 778.7502325331095108, -432.3510508353226669, 304.6391490659818828 ) ) ;
#43568 = EDGE_CURVE ( 'NONE', #34810, #10891, #20900, .T. ) ;
#43569 = CARTESIAN_POINT ( 'NONE',  ( 803.6646147819161570, -353.9073299311467053, 348.8264449731210561 ) ) ;
#43570 = ADVANCED_FACE ( 'NONE', ( #38216 ), #31947, .F. ) ;
#43571 = CARTESIAN_POINT ( 'NONE',  ( 759.0252816721024374, -72.99823902205667991, -368.0189434323527280 ) ) ;
#43572 = CARTESIAN_POINT ( 'NONE',  ( 797.6776695296629214, -67.54369356751125508, -357.6776695296636603 ) ) ;
#43573 = ORIENTED_EDGE ( 'NONE', *, *, #169, .F. ) ;
#43574 = CARTESIAN_POINT ( 'NONE',  ( 784.1219089521767955, 2.718209154846545683, -315.0488828828318333 ) ) ;
#43575 = ORIENTED_EDGE ( 'NONE', *, *, #44398, .F. ) ;
#43576 = CARTESIAN_POINT ( 'NONE',  ( 755.3028492785439312, -327.2817908451525000, -335.9200461376539693 ) ) ;
#43577 = ITEM_DEFINED_TRANSFORMATION ( 'NONE', 'NONE', #17965,  #26858 ) ;
#43579 = CARTESIAN_POINT ( 'NONE',  ( 755.1538015810308480, -374.1908817542432075, 343.0433043558613804 ) ) ;
#43578 = CARTESIAN_POINT ( 'NONE',  ( 758.0580252608178853, -54.45278447660219001, 328.0187753319985404 ) ) ;
#43580 = CARTESIAN_POINT ( 'NONE',  ( 759.9864689768902508, -338.0891481129649492, -354.9819416627836404 ) ) ;
#43582 = CARTESIAN_POINT ( 'NONE',  ( 745.1769319972822814, -305.8055962898684470, 346.2694204179732083 ) ) ;
#43581 = CARTESIAN_POINT ( 'NONE',  ( 801.1904061080338124, -428.0891481129645513, 368.3070685750236066 ) ) ;
#43583 = CARTESIAN_POINT ( 'NONE',  ( 812.6845335610512393, -103.9874144716873161, 353.5525998758768651 ) ) ;
#43584 = CARTESIAN_POINT ( 'NONE',  ( 755.1538015810308480, -326.1908817542433781, -343.0433043558613804 ) ) ;
#43585 = CARTESIAN_POINT ( 'NONE',  ( 804.9363028652555840, -280.2709662947833067, -338.2165204200192079 ) ) ;
#43586 = DIRECTION ( 'NONE',  ( 0.000000000000000000, 0.000000000000000000, 1.000000000000000000 ) ) ;
#43587 = CARTESIAN_POINT ( 'NONE',  ( 803.6646147819161570, -161.9073299311472454, -348.8264449731210561 ) ) ;
#43588 = EDGE_CURVE ( 'NONE', #32812, #18154, #2442, .T. ) ;
#43589 = LINE ( 'NONE', #26024, #29203 ) ;
#43590 = CARTESIAN_POINT ( 'NONE',  ( 801.1904061080336987, -428.0891481129644944, 368.3070685750235498 ) ) ;
#43592 = DIRECTION ( 'NONE',  ( -0.000000000000000000, -0.000000000000000000, 1.000000000000000000 ) ) ;
#43591 = LINE ( 'NONE', #3894, #1966 ) ;
#43593 = ADVANCED_FACE ( 'NONE', ( #13959, #25661, #38436 ), #36059, .T. ) ;
#43594 = CARTESIAN_POINT ( 'NONE',  ( 745.5313806188320314, -87.28179084515316788, -333.7943932421247268 ) ) ;
#43595 = CARTESIAN_POINT ( 'NONE',  ( 989.9999999999992042, 249.9999999999998863, 209.9999999999999716 ) ) ;
#43596 = LINE ( 'NONE', #880, #17892 ) ;
#43597 = CARTESIAN_POINT ( 'NONE',  ( 780.5236548040995785, -308.7363362996979390, 314.9735926884559944 ) ) ;
#43598 = CARTESIAN_POINT ( 'NONE',  ( 803.6646147819161570, -161.9073299311472454, 348.8264449731210561 ) ) ;
#43599 = EDGE_CURVE ( 'NONE', #120, #3087, #36277, .T. ) ;
#43600 = ORIENTED_EDGE ( 'NONE', *, *, #33454, .T. ) ;
#43601 = CARTESIAN_POINT ( 'NONE',  ( 772.5602148656447525, -129.7255117493292289, -305.7998596910095443 ) ) ;
#43602 = CARTESIAN_POINT ( 'NONE',  ( 754.8983024940795303, -330.8965053807774552, 336.9254006560228163 ) ) ;
#43603 = CARTESIAN_POINT ( 'NONE',  ( 1007.605605532488426, -110.5936016518798652, 750.6326042729449455 ) ) ;
#43604 = CARTESIAN_POINT ( 'NONE',  ( 805.6418435158337843, -77.46360902697138329, 363.8556311672236916 ) ) ;
#43605 = CARTESIAN_POINT ( 'NONE',  ( 751.9810565676468741, -266.0891481129651197, -360.9747183278973921 ) ) ;
#43606 = CARTESIAN_POINT ( 'NONE',  ( 745.0891759886404770, -196.2709662947835909, 342.4968714119734159 ) ) ;
#43607 = CARTESIAN_POINT ( 'NONE',  ( 788.7366044899766848, -131.9073299311473875, 316.5762568750059813 ) ) ;
#43608 = ORIENTED_EDGE ( 'NONE', *, *, #21836, .F. ) ;
#43609 = CARTESIAN_POINT ( 'NONE',  ( 746.7653713866222915, -329.2601417444138860, -351.0478386215610271 ) ) ;
#43610 = CARTESIAN_POINT ( 'NONE',  ( 758.8095938919642549, -80.08914811296574499, -311.6929314249763365 ) ) ;
#43611 = ADVANCED_FACE ( 'NONE', ( #24553 ), #20641, .T. ) ;
#43612 = CARTESIAN_POINT ( 'NONE',  ( 796.9571628226829034, 0.5363909730283709099, 321.2382568024804641 ) ) ;
#43613 = CARTESIAN_POINT ( 'NONE',  ( 767.6429770376289525, -345.1800572038739006, -306.8695393053162093 ) ) ;
#43614 = FACE_BOUND ( 'NONE', #39174, .T. ) ;
#43615 = CARTESIAN_POINT ( 'NONE',  ( 761.2382568024794409, -399.6237781080500326, 356.9571628226838129 ) ) ;
#43616 = EDGE_LOOP ( 'NONE', ( #8418, #38288, #7248, #18873 ) ) ;
#43617 = CARTESIAN_POINT ( 'NONE',  ( 776.9566956441375396, -84.89650538077830788, 364.8461984189686405 ) ) ;
#43618 = CARTESIAN_POINT ( 'NONE',  ( 781.8018195045266339, -430.2709662947827383, -365.1927285166406705 ) ) ;
#43619 = EDGE_CURVE ( 'NONE', #338, #44890, #32370, .T. ) ;
#43620 = CARTESIAN_POINT ( 'NONE',  ( 795.1360043628807261, -212.0891481129652902, -360.2193346964456282 ) ) ;
#43621 = CARTESIAN_POINT ( 'NONE',  ( 751.2241431872005251, -112.1692326535054889, -359.9636004259367610 ) ) ;
#43622 = CARTESIAN_POINT ( 'NONE',  ( 180.7583438952258916, 294.6698570112193920, -224.9999999999999716 ) ) ;
#43623 = CARTESIAN_POINT ( 'NONE',  ( 786.2056067578752163, -251.8055962898686744, 374.4686193811670023 ) ) ;
#43624 = CARTESIAN_POINT ( 'NONE',  ( 778.2165204200184689, -46.81642084023858530, 364.9363028652563230 ) ) ;
#43625 = CARTESIAN_POINT ( 'NONE',  ( 802.7791456095903868, -244.7146871989596093, -329.0155153010375102 ) ) ;
#43626 = CARTESIAN_POINT ( 'NONE',  ( 804.4286716492782716, -233.3618753856925423, 345.3141322388244703 ) ) ;
#43627 = EDGE_CURVE ( 'NONE', #22885, #5495, #32592, .T. ) ;
#43628 = CARTESIAN_POINT ( 'NONE',  ( 772.5602148656447525, 14.27448825067031812, -305.7998596910095443 ) ) ;
#43629 = CARTESIAN_POINT ( 'NONE',  ( 776.2433038121456548, -60.89650538077837894, -374.8207195650711014 ) ) ;
#43630 = DIRECTION ( 'NONE',  ( -1.000000000000000000, -0.000000000000000000, -0.000000000000000000 ) ) ;
#43631 = ORIENTED_EDGE ( 'NONE', *, *, #90, .T. ) ;
#43632 = ORIENTED_EDGE ( 'NONE', *, *, #10271, .F. ) ;
#43633 = CARTESIAN_POINT ( 'NONE',  ( 771.3260364891663130, -379.6454272087886466, -306.0683387631859773 ) ) ;
#43634 = CARTESIAN_POINT ( 'NONE',  ( 801.1904061080338124, -284.0891481129651197, 368.3070685750236066 ) ) ;
#43635 = CARTESIAN_POINT ( 'NONE',  ( 744.8212110874229666, -18.89650538077849617, 336.2046728542121627 ) ) ;
#43636 = CARTESIAN_POINT ( 'NONE',  ( 804.8461984189677878, -194.1908817542437475, -336.9566956441385628 ) ) ;
#43637 = CARTESIAN_POINT ( 'NONE',  ( 755.3201227861273992, -171.7255117493291152, -345.3687786644892981 ) ) ;
#43638 = CIRCLE ( 'NONE', #6013, 8.024999999999948841 ) ;
#43639 = CARTESIAN_POINT ( 'NONE',  ( 785.3687786644885591, -371.3618753856920307, -315.3201227861280813 ) ) ;
#43640 = EDGE_LOOP ( 'NONE', ( #38255, #6079, #19062, #12226, #42164, #2337, #16592 ) ) ;
#43641 = CARTESIAN_POINT ( 'NONE',  ( 762.3223304703356007, -223.5436935675107577, 322.3223304703362828 ) ) ;
#43642 = CARTESIAN_POINT ( 'NONE',  ( 784.0799538623451781, 12.19440371013049784, -364.6971507214555572 ) ) ;
#43643 = ORIENTED_EDGE ( 'NONE', *, *, #44755, .F. ) ;
#43644 = CARTESIAN_POINT ( 'NONE',  ( 747.2067596250078623, -315.1800572038740711, 352.2312462859687230 ) ) ;
#43645 = CARTESIAN_POINT ( 'NONE',  ( 799.9999999999993179, -373.0259173205825505, 36.60293108048681887 ) ) ;
#43646 = CARTESIAN_POINT ( 'NONE',  ( 792.0613484971601110, -458.0032201311295807, -367.4685979341032294 ) ) ;
#43647 = DIRECTION ( 'NONE',  ( -0.000000000000000000, 1.000000000000000000, -0.000000000000000000 ) ) ;
#43648 = CARTESIAN_POINT ( 'NONE',  ( 763.0428371773158460, -179.4636090269710849, 358.7617431975195359 ) ) ;
#43649 = CARTESIAN_POINT ( 'NONE',  ( 805.1927285166397041, -64.81642084023852135, 341.8018195045277707 ) ) ;
#43650 = ORIENTED_EDGE ( 'NONE', *, *, #18208, .T. ) ;
#43651 = CARTESIAN_POINT ( 'NONE',  ( 754.3581564841646241, -401.4636090269704027, -316.1443688327762516 ) ) ;
#43652 = CARTESIAN_POINT ( 'NONE',  ( 792.3570229623691148, -21.18005720387502322, -373.1304606946836770 ) ) ;
#43653 = CARTESIAN_POINT ( 'NONE',  ( 772.3691319403857278, -239.2601417444141987, 315.8894580844506663 ) ) ;
#43654 = CARTESIAN_POINT ( 'NONE',  ( 762.1405469898971887, -409.5436935675101040, -357.8594530101015607 ) ) ;
#43655 = CARTESIAN_POINT ( 'NONE',  ( 756.5762568750052424, -3.180057203875080063, -348.7366044899774238 ) ) ;
#43656 = CARTESIAN_POINT ( 'NONE',  ( 772.5602148656447525, -417.7255117493283478, 305.7998596910095443 ) ) ;
#43657 = DIRECTION ( 'NONE',  ( 0.000000000000000000, 0.000000000000000000, 1.000000000000000000 ) ) ;
#43658 = CARTESIAN_POINT ( 'NONE',  ( 783.0745993439762742, -248.1908817542435202, -365.1016975059196739 ) ) ;
#43659 = CARTESIAN_POINT ( 'NONE',  ( 772.5602148656447525, -153.7255117493291721, -305.7998596910095443 ) ) ;
#43660 = CARTESIAN_POINT ( 'NONE',  ( 814.5518280994195948, -63.72551174932939233, 332.4837098697145734 ) ) ;
#43661 = CARTESIAN_POINT ( 'NONE',  ( 755.2512626584698410, -103.5436935675111272, 315.2512626584710915 ) ) ;
#43662 = CARTESIAN_POINT ( 'NONE',  ( 795.2260422076361692, 16.45630643248849978, -314.2591110605560516 ) ) ;
#43663 = DIRECTION ( 'NONE',  ( 0.000000000000000000, 0.000000000000000000, 1.000000000000000000 ) ) ;
#43664 = CARTESIAN_POINT ( 'NONE',  ( 764.1737431748507561, -394.3726999360613377, 371.6461892240376415 ) ) ;
#43665 = EDGE_CURVE ( 'NONE', #23858, #19525, #5, .T. ) ;
#43666 = CARTESIAN_POINT ( 'NONE',  ( -746.4999999999993179, -365.3551492539851893, -28.13243251470704109 ) ) ;
#43667 = CARTESIAN_POINT ( 'NONE',  ( 777.5031285880264704, -358.8164208402375834, 374.9108240113588408 ) ) ;
#43668 = CARTESIAN_POINT ( 'NONE',  ( 759.7806653035534055, -318.9982390220557704, -324.8639956371180801 ) ) ;
#43669 = CARTESIAN_POINT ( 'NONE',  ( 784.0799538623451781, 12.19440371013049784, 364.6971507214555572 ) ) ;
#43670 = AXIS2_PLACEMENT_3D ( 'NONE', #19073, #29250, #25977 ) ;
#43671 = CARTESIAN_POINT ( 'NONE',  ( 747.6481478633932056, -109.0999726633349241, -353.4146539503763620 ) ) ;
#43672 = CARTESIAN_POINT ( 'NONE',  ( 804.1601925771018387, -127.4419599262326983, -346.5483106153029098 ) ) ;
#43673 = CARTESIAN_POINT ( 'NONE',  ( 808.7758568127978833, -124.1692326535054463, 320.0363995740631822 ) ) ;
#43674 = CARTESIAN_POINT ( 'NONE',  ( 800.2193346964446619, -426.9982390220555430, 355.1360043628816925 ) ) ;
#43675 = CARTESIAN_POINT ( 'NONE',  ( 804.9363028652555840, -16.27096629478413092, -338.2165204200192079 ) ) ;
#43676 = CARTESIAN_POINT ( 'NONE',  ( 776.9566956441375396, -132.8965053807781374, -364.8461984189686405 ) ) ;
#43677 = CARTESIAN_POINT ( 'NONE',  ( 756.3353852180819104, -125.9073299311474159, -331.1735550268788302 ) ) ;
#43678 = CARTESIAN_POINT ( 'NONE',  ( 804.4286716492782716, -113.3618753856929260, 345.3141322388244703 ) ) ;
#43679 = CARTESIAN_POINT ( 'NONE',  ( 801.3366627262608972, -440.5328690171407970, -353.0897708529566899 ) ) ;
#43681 = CARTESIAN_POINT ( 'NONE',  ( 800.2193346964446619, -258.9982390220561115, 355.1360043628816925 ) ) ;
#43680 = CARTESIAN_POINT ( 'NONE',  ( 774.6858677611749044, -249.7255117493288594, 315.5713283507209894 ) ) ;
#43682 = LINE ( 'NONE', #40009, #32316 ) ;
#43683 = VERTEX_POINT ( 'NONE', #6664 ) ;
#43684 = CARTESIAN_POINT ( 'NONE',  ( 803.8651313633788504, 18.73985825558501972, 332.4468031744301015 ) ) ;
#43685 = VERTEX_POINT ( 'NONE', #193 ) ;
#43686 = CARTESIAN_POINT ( 'NONE',  ( 777.4774526936600978, -178.2709662947835909, 304.7301800767028226 ) ) ;
#43687 = CARTESIAN_POINT ( 'NONE',  ( 801.5560724626406000, -312.5545181178797520, 326.7756240680316182 ) ) ;
#43688 = CARTESIAN_POINT ( 'NONE',  ( 783.0433043558608688, -408.8965053807772847, 315.1538015810313027 ) ) ;
#43689 = ORIENTED_EDGE ( 'NONE', *, *, #12005, .F. ) ;
#43690 = CARTESIAN_POINT ( 'NONE',  ( 802.9823548866075953, -73.09997266333502353, -330.0799878456151077 ) ) ;
#43691 = AXIS2_PLACEMENT_3D ( 'NONE', #35302, #10833, #24669 ) ;
#43692 = CARTESIAN_POINT ( 'NONE',  ( 754.8072714833583632, -292.8164208402378108, -338.1981804954721156 ) ) ;
#43693 = VERTEX_POINT ( 'NONE', #38534 ) ;
#43694 = CARTESIAN_POINT ( 'NONE',  ( 778.1981804954714335, -394.2709662947827951, -314.8072714833589885 ) ) ;
#43695 = CARTESIAN_POINT ( 'NONE',  ( 774.6312213355099630, -47.36187538569312494, -364.6798772138717482 ) ) ;
#43696 = CARTESIAN_POINT ( 'NONE',  ( 801.3366627262608972, -272.5328690171413086, 353.0897708529566899 ) ) ;
#43697 = CARTESIAN_POINT ( 'NONE',  ( -26.63011601220122060, -512.9681489794448908, -339.9999999999999432 ) ) ;
#43698 = FACE_BOUND ( 'NONE', #18137, .T. ) ;
#43699 = CARTESIAN_POINT ( 'NONE',  ( 749.5768839229115201, -12.55451811788067751, -358.0661480581553064 ) ) ;
#43700 = CARTESIAN_POINT ( 'NONE',  ( -26.63011601220122060, -563.3203001761230553, -342.3463313526983143 ) ) ;
#43701 = ORIENTED_EDGE ( 'NONE', *, *, #40816, .F. ) ;
#43702 = CARTESIAN_POINT ( 'NONE',  ( 749.5768839229115201, -300.5545181178797520, -358.0661480581553064 ) ) ;
#43703 = CARTESIAN_POINT ( 'NONE',  ( 764.1737431748507561, -178.3726999360619629, 371.6461892240376415 ) ) ;
#43705 = CARTESIAN_POINT ( 'NONE',  ( 754.8072714833581358, -292.8164208402376971, -338.1981804954720587 ) ) ;
#43704 = LINE ( 'NONE', #29413, #39411 ) ;
#43706 = CARTESIAN_POINT ( 'NONE',  ( 180.7583438952259201, 294.6698570112193920, -244.9999999999999716 ) ) ;
#43707 = CARTESIAN_POINT ( 'NONE',  ( 801.5560724626406000, -144.5545181178802636, -326.7756240680316182 ) ) ;
#43708 = CARTESIAN_POINT ( 'NONE',  ( 831.1634899080286232, 239.9999999999999147, -197.2500000000000853 ) ) ;
#43709 = CARTESIAN_POINT ( 'NONE',  ( 754.0944755984390895, -15.62377810805123524, -364.1009440267246760 ) ) ;
#43710 = CARTESIAN_POINT ( 'NONE',  ( 810.7187646348534145, -330.4527844766013231, -356.7737145352016341 ) ) ;
#43711 = DIRECTION ( 'NONE',  ( 0.000000000000000000, -0.000000000000000000, -1.000000000000000000 ) ) ;
#43712 = CARTESIAN_POINT ( 'NONE',  ( 755.0636971347428243, -28.27096629478409540, 341.7834795799807353 ) ) ;
#43713 = CARTESIAN_POINT ( 'NONE',  ( 778.7629533639073998, -296.7363362996979390, 375.0009284576466371 ) ) ;
#43714 = CARTESIAN_POINT ( 'NONE',  ( 759.0252816721024374, -264.9982390220561115, 368.0189434323527280 ) ) ;
#43715 = CARTESIAN_POINT ( 'NONE',  ( 811.0346526505616112, 9.365397341579420498, -323.0537975583477532 ) ) ;
#43716 = DIRECTION ( 'NONE',  ( 0.000000000000000000, -1.000000000000000000, 0.000000000000000000 ) ) ;
#43717 = VERTEX_POINT ( 'NONE', #21663 ) ;
#43718 = CARTESIAN_POINT ( 'NONE',  ( 755.3201227861273992, -363.7255117493284047, 345.3687786644892981 ) ) ;
#43719 = CIRCLE ( 'NONE', #42249, 8.024999999999948841 ) ;
#43720 = CARTESIAN_POINT ( 'NONE',  ( 763.8424801807145741, -138.0090635724257311, 320.5453621957614700 ) ) ;
#43721 = CARTESIAN_POINT ( 'NONE',  ( 790.8726784830453198, -10.71468719896033761, -362.5472867521010585 ) ) ;
#43722 = DIRECTION ( 'NONE',  ( 0.000000000000000000, 0.000000000000000000, 1.000000000000000000 ) ) ;
#43723 = CARTESIAN_POINT ( 'NONE',  ( 799.9999999999993179, 212.6707680665973612, -236.5295014342203785 ) ) ;
#43724 = CARTESIAN_POINT ( 'NONE',  ( 765.0180583372156207, -384.9982390220556567, 360.0135310231089534 ) ) ;
#43725 = ORIENTED_EDGE ( 'NONE', *, *, #35171, .T. ) ;
#43726 = CARTESIAN_POINT ( 'NONE',  ( 783.0433043558608688, -312.8965053807775689, -315.1538015810313027 ) ) ;
#43727 = CARTESIAN_POINT ( 'NONE',  ( 757.8323909638827445, -170.6346026584199649, 352.1044303154654358 ) ) ;
#43728 = CARTESIAN_POINT ( 'NONE',  ( 803.8556311672234642, -345.6237781080501463, -365.6418435158340117 ) ) ;
#43729 = CARTESIAN_POINT ( 'NONE',  ( -468.8365100919714337, 260.0000000000001705, -193.8809999999909053 ) ) ;
#43730 = EDGE_LOOP ( 'NONE', ( #18832, #6498 ) ) ;
#43731 = CARTESIAN_POINT ( 'NONE',  ( 765.0180583372156207, -360.9982390220557704, 360.0135310231089534 ) ) ;
#43732 = ORIENTED_EDGE ( 'NONE', *, *, #13049, .F. ) ;
#43733 = CARTESIAN_POINT ( 'NONE',  ( 781.7834795799800531, -442.8164208402372992, 315.0636971347436202 ) ) ;
#43734 = CARTESIAN_POINT ( 'NONE',  ( 744.7301800767019131, -172.8164208402381234, -337.4774526936615757 ) ) ;
#43735 = CARTESIAN_POINT ( 'NONE',  ( 747.2067596250078623, -99.18005720387478164, 352.2312462859687230 ) ) ;
#43736 = EDGE_LOOP ( 'NONE', ( #15149, #8000, #20609, #22996 ) ) ;
#43737 = CARTESIAN_POINT ( 'NONE',  ( 778.2165204200184689, -166.8164208402382087, -364.9363028652563230 ) ) ;
#43738 = ORIENTED_EDGE ( 'NONE', *, *, #5789, .F. ) ;
#43739 = CARTESIAN_POINT ( 'NONE',  ( 805.2837595273609850, -410.7363362996976548, -340.5290396650784714 ) ) ;
#43740 = CARTESIAN_POINT ( 'NONE',  ( 764.8639956371174549, -8.089148112965974136, 319.7806653035542013 ) ) ;
#43741 = CARTESIAN_POINT ( 'NONE',  ( 756.1348686366196716, -161.2601417444143976, 347.5531968255698416 ) ) ;
#43743 = CARTESIAN_POINT ( 'NONE',  ( -26.63011601220122060, -513.1383975375929367, -349.9999999999999432 ) ) ;
#43742 = DIRECTION ( 'NONE',  ( 0.000000000000000000, 0.000000000000000000, 1.000000000000000000 ) ) ;
#43744 = VERTEX_POINT ( 'NONE', #3889 ) ;
#43745 = CARTESIAN_POINT ( 'NONE',  ( 804.8461984189677878, -434.1908817542430370, -336.9566956441385628 ) ) ;
#43746 = CARTESIAN_POINT ( 'NONE',  ( 769.9999999999992042, 205.0000000000000568, -360.0000000000000000 ) ) ;
#43747 = CIRCLE ( 'NONE', #20145, 10.00000000000000888 ) ;
#43748 = CARTESIAN_POINT ( 'NONE',  ( 786.2694204179717872, -189.2817908451528979, -305.1769319972829067 ) ) ;
#43749 = CIRCLE ( 'NONE', #43044, 6.118999999999985562 ) ;
#43750 = CARTESIAN_POINT ( 'NONE',  ( 755.8990559732751535, -83.46360902697136908, 365.9055244015606831 ) ) ;
#43752 = CARTESIAN_POINT ( 'NONE',  ( 756.5762568750052424, -171.1800572038745543, -348.7366044899774238 ) ) ;
#43751 = DIRECTION ( 'NONE',  ( -1.000000000000000000, -0.000000000000000000, -0.000000000000000000 ) ) ;
#43753 = CARTESIAN_POINT ( 'NONE',  ( 804.9511171171677688, -341.8055962898683333, -335.8780910478229202 ) ) ;
#43754 = CARTESIAN_POINT ( 'NONE',  ( 571.1634899080285095, 259.9999999999999432, -199.9999999999981526 ) ) ;
#43755 = CARTESIAN_POINT ( 'NONE',  ( 788.6739635108323228, -223.6454272087891013, -373.9316612368139090 ) ) ;
#43756 = CARTESIAN_POINT ( 'NONE',  ( -338.8365100919713200, 240.0000000000001421, -199.9999999999917861 ) ) ;
#43757 = DIRECTION ( 'NONE',  ( 0.000000000000000000, 0.9238795325112891810, -0.3826834323650838421 ) ) ;
#43758 = CARTESIAN_POINT ( 'NONE',  ( 790.0220218866281812, -31.09997266333516919, -363.2186876482849129 ) ) ;
#43759 = CARTESIAN_POINT ( 'NONE',  ( 790.0220218866281812, -415.0999726633340288, 363.2186876482849129 ) ) ;
#43760 = CARTESIAN_POINT ( 'NONE',  ( 755.2512626584698410, -247.5436935675106724, -315.2512626584710915 ) ) ;
#43761 = LINE ( 'NONE', #37297, #12083 ) ;
#43762 = CARTESIAN_POINT ( 'NONE',  ( 755.3201227861273992, -3.725511749329622813, -345.3687786644892981 ) ) ;
#43763 = CARTESIAN_POINT ( 'NONE',  ( 814.8207195650702488, -194.1908817542437475, 336.2433038121456548 ) ) ;
#43764 = CARTESIAN_POINT ( 'NONE',  ( 752.4576283171824116, -117.0783235625963528, -317.7880784355627952 ) ) ;
#43765 = CARTESIAN_POINT ( 'NONE',  ( 759.0252816721024374, -144.9982390220564525, 368.0189434323527280 ) ) ;
#43766 = CARTESIAN_POINT ( 'NONE',  ( 747.2067596250078623, -387.1800572038738437, -352.2312462859687230 ) ) ;
#43767 = CARTESIAN_POINT ( 'NONE',  ( 911.9999999999994316, 154.9999999999998863, 360.0000000000000000 ) ) ;
#43768 = DIRECTION ( 'NONE',  ( -0.000000000000000000, -0.000000000000000000, 1.000000000000000000 ) ) ;
#43769 = CARTESIAN_POINT ( 'NONE',  ( 762.3223304703356007, -247.5436935675106724, 322.3223304703362828 ) ) ;
#43770 = CARTESIAN_POINT ( 'NONE',  ( 799.2566176426618085, -24.00906357242609346, 324.0069404352559559 ) ) ;
#43771 = CARTESIAN_POINT ( 'NONE',  ( 795.1360043628807261, -380.0891481129646650, -360.2193346964456282 ) ) ;
#43772 = CARTESIAN_POINT ( 'NONE',  ( 755.2512626584698410, 16.45630643248848912, -315.2512626584710915 ) ) ;
#43773 = CARTESIAN_POINT ( 'NONE',  ( 814.9108240113580450, -448.2709662947827951, -337.5031285880265273 ) ) ;
#43774 = DIRECTION ( 'NONE',  ( 1.000000000000000000, 2.313994520913686024E-32, 2.750100768424433609E-32 ) ) ;
#43775 = CARTESIAN_POINT ( 'NONE',  ( 757.2208543904082489, -64.71468719896019195, 350.9844846989624330 ) ) ;
#43776 = ORIENTED_EDGE ( 'NONE', *, *, #42420, .F. ) ;
#43777 = CARTESIAN_POINT ( 'NONE',  ( 779.4709603349208464, -216.3510508353233490, -314.7162404726379918 ) ) ;
#43778 = VECTOR ( 'NONE', #2413, 1000.000000000000000 ) ;
#43779 = CARTESIAN_POINT ( 'NONE',  ( 771.2633955100217236, -23.90732993114773919, 363.4237431249939618 ) ) ;
#43780 = CIRCLE ( 'NONE', #31266, 2.749999999999863665 ) ;
#43781 = CARTESIAN_POINT ( 'NONE',  ( 761.9338519418445230, -230.5328690171415076, -370.4231160770881957 ) ) ;
#43782 = LINE ( 'NONE', #23210, #22365 ) ;
#43783 = CARTESIAN_POINT ( 'NONE',  ( 811.6461892240364477, -340.7146871989592114, 324.1737431748509835 ) ) ;
#43784 = ORIENTED_EDGE ( 'NONE', *, *, #30897, .F. ) ;
#43785 = CARTESIAN_POINT ( 'NONE',  ( 762.3223304703356007, -151.5436935675109851, -322.3223304703362828 ) ) ;
#43786 = CARTESIAN_POINT ( 'NONE',  ( 791.9812246680005501, -332.6346026584195101, 361.9419747391813189 ) ) ;
#43787 = CARTESIAN_POINT ( 'NONE',  ( 767.6429770376289525, -81.18005720387481006, -306.8695393053162093 ) ) ;
#43788 = EDGE_CURVE ( 'NONE', #13142, #39820, #10825, .T. ) ;
#43789 = CARTESIAN_POINT ( 'NONE',  ( 774.6312213355098493, -71.36187538569303968, -364.6798772138717482 ) ) ;
#43790 = ORIENTED_EDGE ( 'NONE', *, *, #4385, .T. ) ;
#43791 = CARTESIAN_POINT ( 'NONE',  ( 760.7433823573367135, -12.00906357242613609, -355.9930595647440441 ) ) ;
#43792 = ORIENTED_EDGE ( 'NONE', *, *, #14813, .F. ) ;
#43793 = CARTESIAN_POINT ( 'NONE',  ( 766.9102291470427417, -330.5545181178796952, -318.6633372737382501 ) ) ;
#43794 = CIRCLE ( 'NONE', #27585, 2.749999999999863665 ) ;
#43796 = CARTESIAN_POINT ( 'NONE',  ( 780.5236548040995785, -356.7363362996978253, 314.9735926884559944 ) ) ;
#43795 = CARTESIAN_POINT ( 'NONE',  ( 754.8072714833581358, -52.81642084023856398, 338.1981804954720587 ) ) ;
#43799 = CARTESIAN_POINT ( 'NONE',  ( 749.8865473780648472, -308.5328690171412518, 322.1177392798429082 ) ) ;
#43798 = PLANE ( 'NONE',  #23277 ) ;
#43797 = CARTESIAN_POINT ( 'NONE',  ( 814.2001403089898304, -425.3618753856919170, 347.4397851343538264 ) ) ;
#43800 = CARTESIAN_POINT ( 'NONE',  ( 800.1688906516307043, -106.1692326535054889, 369.0717654672308186 ) ) ;
#43801 = CARTESIAN_POINT ( 'NONE',  ( 769.9779781133707957, -331.0999726633342561, -316.7813123517150871 ) ) ;
#43802 = CARTESIAN_POINT ( 'NONE',  ( 788.8264449731200330, -309.1800572038740711, -363.6646147819171233 ) ) ;
#43803 = CARTESIAN_POINT ( 'NONE',  ( 771.2633955100217236, -143.9073299311473590, -363.4237431249939618 ) ) ;
#43804 = CARTESIAN_POINT ( 'NONE',  ( 745.7998596910086917, -413.3618753856920307, 332.5602148656461168 ) ) ;
#43806 = CARTESIAN_POINT ( 'NONE',  ( 911.9999999999992042, 219.9999999999998863, 359.9749999999999659 ) ) ;
#43805 = LINE ( 'NONE', #9166, #26301 ) ;
#43807 = CARTESIAN_POINT ( 'NONE',  ( 768.9521613784389729, -105.8272453906076578, -373.2346286133773106 ) ) ;
#43808 = DIRECTION ( 'NONE',  ( 1.892425610156518354E-16, 1.000000000000000000, -0.000000000000000000 ) ) ;
#43809 = DIRECTION ( 'NONE',  ( 0.000000000000000000, 0.000000000000000000, 1.000000000000000000 ) ) ;
#43810 = EDGE_CURVE ( 'NONE', #296, #14734, #24660, .T. ) ;
#43811 = CARTESIAN_POINT ( 'NONE',  ( 758.4439275373578084, -300.5545181178797520, 353.2243759319684386 ) ) ;
#43812 = ORIENTED_EDGE ( 'NONE', *, *, #11429, .T. ) ;
#43813 = CIRCLE ( 'NONE', #29811, 30.00000000000002842 ) ;
#43814 = CARTESIAN_POINT ( 'NONE',  ( 777.5031285880264704, -142.8164208402382656, -374.9108240113588408 ) ) ;
#43815 = CARTESIAN_POINT ( 'NONE',  ( 791.0478386215596629, -69.82724539060775726, 306.7653713866226326 ) ) ;
#43816 = CARTESIAN_POINT ( 'NONE',  ( 801.1904061080336987, -284.0891481129650629, -368.3070685750235498 ) ) ;
#43817 = EDGE_CURVE ( 'NONE', #8116, #11158, #34919, .T. ) ;
#43818 = CARTESIAN_POINT ( 'NONE',  ( 755.2512626584698410, -439.5436935675101040, -315.2512626584710915 ) ) ;
#43819 = CARTESIAN_POINT ( 'NONE',  ( 788.7366044899766848, -107.9073299311474727, 316.5762568750059813 ) ) ;
#43820 = ORIENTED_EDGE ( 'NONE', *, *, #1581, .T. ) ;
#43821 = CARTESIAN_POINT ( 'NONE',  ( 756.1443688327750579, -333.6237781080502600, -314.3581564841659315 ) ) ;
#43822 = CARTESIAN_POINT ( 'NONE',  ( 747.2067596250078623, -75.18005720387485269, -352.2312462859687230 ) ) ;
#43823 = AXIS2_PLACEMENT_3D ( 'NONE', #5959, #43630, #26063 ) ;
#43824 = CARTESIAN_POINT ( 'NONE',  ( 793.9708237608222134, 1.081845518482914104, 319.2295555964448681 ) ) ;
#43825 = CARTESIAN_POINT ( 'NONE',  ( 755.2512626584698410, -343.5436935675103314, -315.2512626584710915 ) ) ;
#43826 = CARTESIAN_POINT ( 'NONE',  ( -78.83651009197140525, 260.0000000000000568, -199.9999999999936051 ) ) ;
#43827 = CARTESIAN_POINT ( 'NONE',  ( 755.0488828828309806, -401.8055962898681059, 344.1219089521771934 ) ) ;
#43828 = ORIENTED_EDGE ( 'NONE', *, *, #6400, .F. ) ;
#43829 = VECTOR ( 'NONE', #18631, 1000.000000000000114 ) ;
#43830 = CARTESIAN_POINT ( 'NONE',  ( 756.3353852180819104, -221.9073299311470464, -331.1735550268788302 ) ) ;
#43831 = CARTESIAN_POINT ( 'NONE',  ( 814.8230680027162407, -125.8055962898690581, -333.7305795820267917 ) ) ;
#43832 = DIRECTION ( 'NONE',  ( -1.000000000000000000, -0.000000000000000000, 0.000000000000000000 ) ) ;
#43833 = CARTESIAN_POINT ( 'NONE',  ( 766.5853460496234675, -229.9874144716869466, 372.3518521366060554 ) ) ;
#43834 = CARTESIAN_POINT ( 'NONE',  ( 785.3141322388236176, -45.72551174932949181, 364.4286716492789537 ) ) ;
#43835 = ORIENTED_EDGE ( 'NONE', *, *, #11411, .F. ) ;
#43836 = EDGE_CURVE ( 'NONE', #7747, #12562, #39011, .T. ) ;
#43837 = CARTESIAN_POINT ( 'NONE',  ( 770.0799878456142551, -229.9874144716869466, -362.9823548866085616 ) ) ;
#43838 = CARTESIAN_POINT ( 'NONE',  ( 755.5713283507202505, -221.3618753856925707, 334.6858677611754729 ) ) ;
#43839 = CARTESIAN_POINT ( 'NONE',  ( 744.8212110874229666, -426.8965053807771142, -336.2046728542121627 ) ) ;
#43840 = CARTESIAN_POINT ( 'NONE',  ( 811.6461892240364477, -76.71468719896012090, -324.1737431748509835 ) ) ;
#43841 = ADVANCED_FACE ( 'NONE', ( #18224 ), #32300, .F. ) ;
#43842 = PLANE ( 'NONE',  #31310 ) ;
#43843 = AXIS2_PLACEMENT_3D ( 'NONE', #5833, #12087, #9060 ) ;
#43844 = VERTEX_POINT ( 'NONE', #424 ) ;
#43845 = VERTEX_POINT ( 'NONE', #17533 ) ;
#43846 = CARTESIAN_POINT ( 'NONE',  ( 749.5768839229115201, -372.5545181178796383, -358.0661480581553064 ) ) ;
#43847 = CIRCLE ( 'NONE', #23932, 2.749999999999842792 ) ;
#43848 = CARTESIAN_POINT ( 'NONE',  ( 791.9812246680005501, -236.6346026584198228, -361.9419747391813189 ) ) ;
#43849 = CARTESIAN_POINT ( 'NONE',  ( 814.9108240113580450, -328.2709662947831362, 337.5031285880265273 ) ) ;
#43850 = CARTESIAN_POINT ( 'NONE',  ( 805.9055244015594326, -27.62377810805120149, 315.8990559732753240 ) ) ;
#43851 = CARTESIAN_POINT ( 'NONE',  ( 793.0897708529556667, -222.5545181178800362, -361.3366627262616362 ) ) ;
#43852 = CARTESIAN_POINT ( 'NONE',  ( 803.6646147819161570, -185.9073299311472454, -348.8264449731210561 ) ) ;
#43853 = CARTESIAN_POINT ( 'NONE',  ( 754.8072714833583632, -388.8164208402374129, -338.1981804954721156 ) ) ;
#43854 = ORIENTED_EDGE ( 'NONE', *, *, #37699, .F. ) ;
#43855 = CARTESIAN_POINT ( 'NONE',  ( 762.3223304703356007, -199.5436935675108430, 322.3223304703362828 ) ) ;
#43856 = CARTESIAN_POINT ( 'NONE',  ( 791.9812246680005501, -116.6346026584201780, -361.9419747391813189 ) ) ;
#43857 = EDGE_LOOP ( 'NONE', ( #14702, #28768, #32861, #18238, #32162 ) ) ;
#43858 = CARTESIAN_POINT ( 'NONE',  ( 792.3570229623688874, -309.1800572038740711, 373.1304606946836202 ) ) ;
#43859 = CIRCLE ( 'NONE', #23942, 30.00000000000008171 ) ;
#43860 = EDGE_CURVE ( 'NONE', #20005, #19031, #21212, .T. ) ;
#43861 = DIRECTION ( 'NONE',  ( -0.000000000000000000, 0.000000000000000000, 1.000000000000000000 ) ) ;
#43862 = CARTESIAN_POINT ( 'NONE',  ( -928.0249999999991815, 219.9999999999998863, -360.0000000000000000 ) ) ;
#43863 = DIRECTION ( 'NONE',  ( 0.000000000000000000, 0.000000000000000000, 1.000000000000000000 ) ) ;
#43864 = AXIS2_PLACEMENT_3D ( 'NONE', #3349, #42140, #33121 ) ;
#43865 = EDGE_CURVE ( 'NONE', #29001, #1656, #28829, .T. ) ;
#43866 = CARTESIAN_POINT ( 'NONE',  ( 755.5913626894240451, -181.6454272087892434, 346.6156483768012890 ) ) ;
#43867 = VECTOR ( 'NONE', #2181, 1000.000000000000000 ) ;
#43868 = CARTESIAN_POINT ( 'NONE',  ( 762.3223304703356007, -79.54369356751119824, 322.3223304703362828 ) ) ;
#43869 = VERTEX_POINT ( 'NONE', #34831 ) ;
#43870 = CARTESIAN_POINT ( 'NONE',  ( 809.0717654672305343, -436.9181544815157281, -360.1688906516309885 ) ) ;
#43871 = CARTESIAN_POINT ( 'NONE',  ( 759.0252816721024374, -48.99823902205675807, -368.0189434323527280 ) ) ;
#43872 = CARTESIAN_POINT ( 'NONE',  ( 755.0488828828309806, -257.8055962898686744, 344.1219089521771934 ) ) ;
#43873 = CARTESIAN_POINT ( 'NONE',  ( 755.3201227861273992, -411.7255117493282910, -345.3687786644892981 ) ) ;
#43874 = CARTESIAN_POINT ( 'NONE',  ( 771.2633955100217236, -23.90732993114773919, -363.4237431249939618 ) ) ;
#43875 = CARTESIAN_POINT ( 'NONE',  ( 792.3570229623688874, -429.1800572038737869, 373.1304606946836202 ) ) ;
#43876 = DIRECTION ( 'NONE',  ( -0.000000000000000000, 1.000000000000000000, -0.000000000000000000 ) ) ;
#43877 = CARTESIAN_POINT ( 'NONE',  ( 798.5707757039680246, -245.4636090269709143, -356.7845633553585003 ) ) ;
#43878 = CARTESIAN_POINT ( 'NONE',  ( 777.4774526936600978, -178.2709662947835625, -304.7301800767027657 ) ) ;
#43879 = EDGE_CURVE ( 'NONE', #5823, #35615, #3671, .T. ) ;
#43880 = AXIS2_PLACEMENT_3D ( 'NONE', #34220, #1671, #15776 ) ;
#43881 = CARTESIAN_POINT ( 'NONE',  ( 787.5162901302840055, -59.36187538569306810, 305.4481719005792684 ) ) ;
#43882 = CARTESIAN_POINT ( 'NONE',  ( 755.2512626584698410, -151.5436935675109851, 315.2512626584710915 ) ) ;
#43883 = CARTESIAN_POINT ( 'NONE',  ( 791.7419236033215384, 16.45630643248850689, -314.5156751397937001 ) ) ;
#43884 = AXIS2_PLACEMENT_3D ( 'NONE', #503, #14830, #10906 ) ;
#43885 = AXIS2_PLACEMENT_3D ( 'NONE', #33492, #1840, #2296 ) ;
#43886 = DIRECTION ( 'NONE',  ( 0.000000000000000000, 0.000000000000000000, 1.000000000000000000 ) ) ;
#43887 = CARTESIAN_POINT ( 'NONE',  ( 811.0346526505616112, -374.6346026584192828, 323.0537975583477532 ) ) ;
#43888 = CARTESIAN_POINT ( 'NONE',  ( 804.6798772138708955, -327.7255117493285184, -334.6312213355107019 ) ) ;
#43889 = CARTESIAN_POINT ( 'NONE',  ( 756.7813123517142913, 4.012585528312341054, 329.9779781133712504 ) ) ;
#43890 = AXIS2_PLACEMENT_3D ( 'NONE', #29011, #29676, #18850 ) ;
#43891 = CARTESIAN_POINT ( 'NONE',  ( 760.0363995740630116, -82.91815448151682233, -368.7758568127991907 ) ) ;
#43892 = CARTESIAN_POINT ( 'NONE',  ( 790.8726784830453198, -130.7146871989599504, -362.5472867521010585 ) ) ;
#43893 = EDGE_CURVE ( 'NONE', #40820, #15260, #22351, .T. ) ;
#43894 = CARTESIAN_POINT ( 'NONE',  ( 812.6845335610512393, -127.9874144716872308, 353.5525998758768651 ) ) ;
#43895 = DIRECTION ( 'NONE',  ( -0.000000000000000000, 1.000000000000000000, -0.000000000000000000 ) ) ;
#43896 = AXIS2_PLACEMENT_3D ( 'NONE', #31740, #335, #39376 ) ;
#43897 = ADVANCED_FACE ( 'NONE', ( #41285 ), #9180, .F. ) ;
#43898 = CARTESIAN_POINT ( 'NONE',  ( 795.1360043628807261, -20.08914811296592973, -360.2193346964456282 ) ) ;
#43899 = CARTESIAN_POINT ( 'NONE',  ( 756.7813123517142913, -115.9874144716872877, -329.9779781133712504 ) ) ;
#43900 = CARTESIAN_POINT ( 'NONE',  ( 804.6798772138708955, -135.7255117493291152, -334.6312213355107019 ) ) ;
#43901 = CARTESIAN_POINT ( 'NONE',  ( 805.1927285166397041, -136.8164208402382371, 341.8018195045277707 ) ) ;
#43902 = AXIS2_PLACEMENT_3D ( 'NONE', #43502, #30312, #11869 ) ;
#43903 = CARTESIAN_POINT ( 'NONE',  ( 775.9200461376533440, -431.8055962898681059, -315.3028492785443291 ) ) ;
#43905 = CARTESIAN_POINT ( 'NONE',  ( 756.5762568750052424, -267.1800572038742985, 348.7366044899774238 ) ) ;
#43904 = CARTESIAN_POINT ( 'NONE',  ( 778.1981804954714335, -274.2709662947833067, 314.8072714833589885 ) ) ;
#43906 = CARTESIAN_POINT ( 'NONE',  ( 999.9999999999992042, -590.0000000000001137, 360.0000000000000000 ) ) ;
#43907 = ORIENTED_EDGE ( 'NONE', *, *, #9431, .F. ) ;
#43908 = CARTESIAN_POINT ( 'NONE',  ( 789.9200121543843807, 22.01258552831228599, 317.0176451133914384 ) ) ;
#43909 = CARTESIAN_POINT ( 'NONE',  ( 799.9636004259356241, -286.9181544815161828, -311.2241431872006956 ) ) ;
#43910 = ORIENTED_EDGE ( 'NONE', *, *, #21483, .F. ) ;
#43911 = DIRECTION ( 'NONE',  ( 1.000000000000000000, 0.000000000000000000, 0.000000000000000000 ) ) ;
#43912 = CARTESIAN_POINT ( 'NONE',  ( 812.7932403749906598, -231.1800572038743553, 327.7687537140311633 ) ) ;
#43913 = CARTESIAN_POINT ( 'NONE',  ( 766.9102291470427417, -306.5545181178797520, 318.6633372737382501 ) ) ;
#43914 = CARTESIAN_POINT ( 'NONE',  ( 803.8651313633788504, -389.2601417444136018, 332.4468031744301015 ) ) ;
#43915 = ORIENTED_EDGE ( 'NONE', *, *, #40244, .F. ) ;
#43916 = CARTESIAN_POINT ( 'NONE',  ( 804.8461984189677878, -98.19088175424404596, -336.9566956441385628 ) ) ;
#43917 = CARTESIAN_POINT ( 'NONE',  ( 755.3201227861273992, -291.7255117493286320, -345.3687786644892981 ) ) ;
#43918 = VECTOR ( 'NONE', #28832, 1000.000000000000000 ) ;
#43919 = ORIENTED_EDGE ( 'NONE', *, *, #42160, .T. ) ;
#43920 = CARTESIAN_POINT ( 'NONE',  ( 759.9864689768902508, -410.0891481129647218, -354.9819416627836404 ) ) ;
#43921 = CARTESIAN_POINT ( 'NONE',  ( 755.3201227861273992, -99.72551174932928575, -345.3687786644892981 ) ) ;
#43922 = CIRCLE ( 'NONE', #37299, 30.00000000000008171 ) ;
#43923 = ADVANCED_FACE ( 'NONE', ( #44514 ), #8742, .F. ) ;
#43924 = CARTESIAN_POINT ( 'NONE',  ( 761.2382568024794409, -279.6237781080503737, 356.9571628226838129 ) ) ;
#43925 = DIRECTION ( 'NONE',  ( -0.000000000000000000, -0.000000000000000000, 1.000000000000000000 ) ) ;
#43926 = CARTESIAN_POINT ( 'NONE',  ( 0.000000000000000000, 0.000000000000000000, 339.9999999999999432 ) ) ;
#43927 = EDGE_CURVE ( 'NONE', #38426, #30631, #4999, .T. ) ;
#43928 = CARTESIAN_POINT ( 'NONE',  ( 814.4686193811664907, -3.281790845153435221, -346.2056067578752732 ) ) ;
#43929 = DIRECTION ( 'NONE',  ( -0.000000000000000000, 1.000000000000000000, -0.000000000000000000 ) ) ;
#43930 = VERTEX_POINT ( 'NONE', #36682 ) ;
#43931 = CARTESIAN_POINT ( 'NONE',  ( 791.0478386215596629, -309.8272453906070041, -306.7653713866226326 ) ) ;
#43932 = CARTESIAN_POINT ( 'NONE',  ( 804.1009440267234822, -191.4636090269709996, 314.0944755984392600 ) ) ;
#43934 = CARTESIAN_POINT ( 'NONE',  ( 756.5762568750052424, -291.1800572038741848, -348.7366044899774238 ) ) ;
#43933 = LINE ( 'NONE', #36997, #19465 ) ;
#43935 = FACE_BOUND ( 'NONE', #24529, .T. ) ;
#43936 = CARTESIAN_POINT ( 'NONE',  ( 802.9823548866075953, -169.0999726633347393, -330.0799878456151077 ) ) ;
#43937 = AXIS2_PLACEMENT_3D ( 'NONE', #32468, #135, #24840 ) ;
#43938 = PRODUCT_RELATED_PRODUCT_CATEGORY ( 'part', '', ( #6326 ) ) ;
#43939 = AXIS2_PLACEMENT_3D ( 'NONE', #30890, #23705, #44985 ) ;
#43940 = DIRECTION ( 'NONE',  ( 1.000000000000000000, 0.000000000000000000, 0.000000000000000000 ) ) ;
#43941 = CARTESIAN_POINT ( 'NONE',  ( 745.0891759886404770, -340.2709662947831362, -342.4968714119734159 ) ) ;
#43942 = DIRECTION ( 'NONE',  ( -1.000000000000000000, -0.000000000000000000, 0.000000000000000000 ) ) ;
#43943 = CARTESIAN_POINT ( 'NONE',  ( 768.0187753319979720, -32.63460265842044095, 318.0580252608186242 ) ) ;
#43944 = CARTESIAN_POINT ( 'NONE',  ( 793.5525998758768083, -271.0999726633344267, 372.6845335610516941 ) ) ;
#43945 = CARTESIAN_POINT ( 'NONE',  ( 745.4481719005789273, -267.7255117493286320, 347.5162901302853129 ) ) ;
#43946 = CARTESIAN_POINT ( 'NONE',  ( 768.8385539511368734, -431.2601417444136018, -306.4236121716840557 ) ) ;
#43947 = DIRECTION ( 'NONE',  ( 0.000000000000000000, 0.000000000000000000, -1.000000000000000000 ) ) ;
#43948 = DIRECTION ( 'NONE',  ( 0.000000000000000000, 0.000000000000000000, -1.000000000000000000 ) ) ;
#43949 = CARTESIAN_POINT ( 'NONE',  ( 774.6858677611749044, -345.7255117493285184, 315.5713283507209894 ) ) ;
#43950 = CARTESIAN_POINT ( 'NONE',  ( 801.5560724626406000, -120.5545181178803205, 326.7756240680316182 ) ) ;
#43951 = CARTESIAN_POINT ( 'NONE',  ( 798.7617431975189675, -27.62377810805120149, -323.0428371773161871 ) ) ;
#43952 = AXIS2_PLACEMENT_3D ( 'NONE', #44904, #19958, #3081 ) ;
#43953 = DIRECTION ( 'NONE',  ( 0.000000000000000000, 1.000000000000000000, 0.000000000000000000 ) ) ;
#43954 = CARTESIAN_POINT ( 'NONE',  ( 879.9999999999990905, -419.8175818341089780, 210.0000000000000000 ) ) ;
#43955 = CARTESIAN_POINT ( 'NONE',  ( 767.8955696845333705, -384.4527844766011526, 362.1676090361162323 ) ) ;
#43956 = VERTEX_POINT ( 'NONE', #23254 ) ;
#43957 = VECTOR ( 'NONE', #2130, 1000.000000000000114 ) ;
#43958 = AXIS2_PLACEMENT_3D ( 'NONE', #43531, #21839, #15151 ) ;
#43959 = CARTESIAN_POINT ( 'NONE',  ( 779.4709603349208464, -336.3510508353228943, -314.7162404726379918 ) ) ;
#43960 = CARTESIAN_POINT ( 'NONE',  ( 803.6646147819161570, -161.9073299311472454, 348.8264449731210561 ) ) ;
#43961 = PRODUCT_DEFINITION_CONTEXT ( 'detailed design', #15185, 'design' ) ;
#43962 = CARTESIAN_POINT ( 'NONE',  ( 758.0141637701419768, -327.0783235625956991, -367.2620300519063790 ) ) ;
#43963 = PLANE ( 'NONE',  #26363 ) ;
#43964 = ORIENTED_EDGE ( 'NONE', *, *, #30634, .T. ) ;
#43965 = CARTESIAN_POINT ( 'NONE',  ( 795.1360043628807261, -356.0891481129647218, 360.2193346964456282 ) ) ;
#43966 = AXIS2_PLACEMENT_3D ( 'NONE', #6428, #35496, #10803 ) ;
#43967 = ORIENTED_EDGE ( 'NONE', *, *, #24972, .F. ) ;
#43968 =( LENGTH_UNIT ( ) NAMED_UNIT ( * ) SI_UNIT ( .MILLI., .METRE. ) );
#43969 = VECTOR ( 'NONE', #36721, 1000.000000000000000 ) ;
#43970 = CARTESIAN_POINT ( 'NONE',  ( 749.2812353651451076, -174.4527844766018063, -323.2262854647983090 ) ) ;
#43971 = CARTESIAN_POINT ( 'NONE',  ( 763.0537975583476964, -72.45278447660213317, 371.0346526505628617 ) ) ;
#43972 = ORIENTED_EDGE ( 'NONE', *, *, #44199, .T. ) ;
#43973 = CARTESIAN_POINT ( 'NONE',  ( 764.8639956371174549, -176.0891481129654039, -319.7806653035542581 ) ) ;
#43974 = ORIENTED_EDGE ( 'NONE', *, *, #43343, .F. ) ;
#43975 = CARTESIAN_POINT ( 'NONE',  ( 804.1105419155481968, -411.8272453906067199, -347.6308680596136469 ) ) ;
#43976 = CARTESIAN_POINT ( 'NONE',  ( 747.2067596250078623, -243.1800572038743269, 352.2312462859687230 ) ) ;
#43977 = CARTESIAN_POINT ( 'NONE',  ( 795.9930595647434757, -171.0783235625962106, 320.7433823573372820 ) ) ;
#43979 = CARTESIAN_POINT ( 'NONE',  ( 914.9999999999992042, 74.99999999999984368, -360.0000000000000000 ) ) ;
#43978 = CARTESIAN_POINT ( 'NONE',  ( 767.9999999999992042, 205.0000000000000568, 360.0000000000000000 ) ) ;
#43980 = ORIENTED_EDGE ( 'NONE', *, *, #43330, .F. ) ;
#43981 = CARTESIAN_POINT ( 'NONE',  ( 799.2566176426618085, -432.0090635724247932, -324.0069404352559559 ) ) ;
#43982 = DIRECTION ( 'NONE',  ( 1.000000000000000000, 0.000000000000000000, 0.000000000000000000 ) ) ;
#43983 = CARTESIAN_POINT ( 'NONE',  ( 781.2370466360911223, -188.7363362996983085, -304.9990715423533629 ) ) ;
#43984 = CARTESIAN_POINT ( 'NONE',  ( 766.4474001241216001, -115.0999726633348956, 307.3154664389482491 ) ) ;
#43985 = AXIS2_PLACEMENT_3D ( 'NONE', #37216, #36991, #1437 ) ;
#43987 = CARTESIAN_POINT ( 'NONE',  ( 802.1676090361156639, -182.6346026584199649, -327.8955696845344505 ) ) ;
#43986 = CARTESIAN_POINT ( 'NONE',  ( 759.9999999999992042, 205.0000000000000568, 339.9999999999999432 ) ) ;
#43988 = CARTESIAN_POINT ( 'NONE',  ( 800.7704444035546203, -364.1692326535046504, -326.0291762391768771 ) ) ;
#43989 = DIRECTION ( 'NONE',  ( 0.000000000000000000, 0.000000000000000000, -1.000000000000000000 ) ) ;
#43990 = CARTESIAN_POINT ( 'NONE',  ( 766.4474001241216001, -211.0999726633346540, -307.3154664389482491 ) ) ;
#43991 = DIRECTION ( 'NONE',  ( 0.000000000000000000, 0.000000000000000000, -1.000000000000000000 ) ) ;
#43992 = LINE ( 'NONE', #8685, #11296 ) ;
#43993 = CARTESIAN_POINT ( 'NONE',  ( 790.0220218866281812, -55.09997266333508747, -363.2186876482849129 ) ) ;
#43994 = VECTOR ( 'NONE', #9572, 1000.000000000000000 ) ;
#43995 = CARTESIAN_POINT ( 'NONE',  ( 758.4439275373578084, -396.5545181178794678, 353.2243759319684386 ) ) ;
#43996 = VECTOR ( 'NONE', #27291, 1000.000000000000000 ) ;
#43997 = CARTESIAN_POINT ( 'NONE',  ( 804.7487373415286811, -259.5436935675106156, -364.7487373415288516 ) ) ;
#43998 = CARTESIAN_POINT ( 'NONE',  ( 804.6971507214547046, -243.2817908451526705, 344.0799538623459739 ) ) ;
#43999 = DIRECTION ( 'NONE',  ( 0.000000000000000000, 0.000000000000000000, 1.000000000000000000 ) ) ;
#44000 = LINE ( 'NONE', #26451, #11358 ) ;
#44001 = CARTESIAN_POINT ( 'NONE',  ( 788.8264449731200330, -45.18005720387493085, -363.6646147819171233 ) ) ;
#44002 = CARTESIAN_POINT ( 'NONE',  ( 791.0478386215596629, -165.8272453906074873, 306.7653713866226326 ) ) ;
#44003 = CARTESIAN_POINT ( 'NONE',  ( 759.8311093483677041, -118.1692326535054463, -310.9282345327691814 ) ) ;
#44004 = CARTESIAN_POINT ( 'NONE',  ( 744.7301800767019131, -148.8164208402382656, 337.4774526936615757 ) ) ;
#44005 = CARTESIAN_POINT ( 'NONE',  ( 787.5162901302840055, -371.3618753856919739, -305.4481719005792684 ) ) ;
#44006 = AXIS2_PLACEMENT_3D ( 'NONE', #33419, #44744, #9403 ) ;
#44007 = DIRECTION ( 'NONE',  ( 0.000000000000000000, 0.000000000000000000, 1.000000000000000000 ) ) ;
#44008 = CARTESIAN_POINT ( 'NONE',  ( 805.1927285166397041, -256.8164208402379245, 341.8018195045277707 ) ) ;
#44009 = CARTESIAN_POINT ( 'NONE',  ( 760.7433823573367135, -12.00906357242613609, 355.9930595647440441 ) ) ;
#44010 = CARTESIAN_POINT ( 'NONE',  ( 802.1676090361156639, -398.6346026584193396, -327.8955696845344505 ) ) ;
#44011 = CARTESIAN_POINT ( 'NONE',  ( -598.8365100919716042, 260.0000000000001705, -199.9999999999899671 ) ) ;
#44012 = CARTESIAN_POINT ( 'NONE',  ( 749.5768839229115201, -12.55451811788067751, -358.0661480581553064 ) ) ;
#44013 = DIRECTION ( 'NONE',  ( -1.000000000000000000, -0.000000000000000000, -0.000000000000000000 ) ) ;
#44014 = CARTESIAN_POINT ( 'NONE',  ( 757.2208543904082489, -88.71468719896009247, 350.9844846989624330 ) ) ;
#44015 = VERTEX_POINT ( 'NONE', #8954 ) ;
#44016 = CARTESIAN_POINT ( 'NONE',  ( 756.7813123517142913, -211.9874144716869750, -329.9779781133712504 ) ) ;
#44017 = CARTESIAN_POINT ( 'NONE',  ( 778.2165204200184689, -70.81642084023850714, 364.9363028652563230 ) ) ;
#44018 = CARTESIAN_POINT ( 'NONE',  ( 786.2056067578752163, -227.8055962898687596, -374.4686193811670023 ) ) ;
#44019 = CARTESIAN_POINT ( 'NONE',  ( -39.63011601220123481, -544.8427095258973623, -369.9999999999999432 ) ) ;
#44020 = CARTESIAN_POINT ( 'NONE',  ( 756.1443688327750579, -357.6237781080501463, 314.3581564841659315 ) ) ;
#44021 = EDGE_LOOP ( 'NONE', ( #32188, #21470, #41314, #6199 ) ) ;
#44022 = AXIS2_PLACEMENT_3D ( 'NONE', #38550, #7844, #14544 ) ;
#44023 = CARTESIAN_POINT ( 'NONE',  ( 755.5713283507202505, -365.3618753856920875, 334.6858677611754729 ) ) ;
#44024 = CIRCLE ( 'NONE', #13817, 30.00000000000008171 ) ;
#44025 = CARTESIAN_POINT ( 'NONE',  ( 815.2698199232961542, -88.81642084023842187, -342.5225473063383106 ) ) ;
#44026 = CARTESIAN_POINT ( 'NONE',  ( 781.7834795799800531, -58.81642084023854267, -315.0636971347436202 ) ) ;
#44027 = VERTEX_POINT ( 'NONE', #41056 ) ;
#44028 = CARTESIAN_POINT ( 'NONE',  ( 776.9254006560222479, -20.19088175424429110, -314.8983024940802125 ) ) ;
#44029 = VECTOR ( 'NONE', #16434, 1000.000000000000000 ) ;
#44030 = ORIENTED_EDGE ( 'NONE', *, *, #43362, .T. ) ;
#44031 = CARTESIAN_POINT ( 'NONE',  ( 763.8424801807145741, -330.0090635724251342, -320.5453621957614700 ) ) ;
#44033 = CARTESIAN_POINT ( 'NONE',  ( 804.4086373105744769, -409.6454272087884760, 333.3843516231986541 ) ) ;
#44032 = CARTESIAN_POINT ( 'NONE',  ( 803.4237431249931660, -111.1800572038747532, 331.2633955100225194 ) ) ;
#44034 = CIRCLE ( 'NONE', #17518, 24.99999999999991118 ) ;
#44037 = CARTESIAN_POINT ( 'NONE',  ( 746.0683387631852383, -331.4419599262320162, 331.3260364891676204 ) ) ;
#44036 = LINE ( 'NONE', #5026, #4119 ) ;
#44035 = CARTESIAN_POINT ( 'NONE',  ( 787.5162901302840055, -443.3618753856917465, 305.4481719005793252 ) ) ;
#44038 = CARTESIAN_POINT ( 'NONE',  ( 815.1787889125755555, -102.8965053807782368, 343.7953271457877804 ) ) ;
#44039 = CARTESIAN_POINT ( 'NONE',  ( 804.1105419155481968, -315.8272453906070609, -347.6308680596136469 ) ) ;
#44040 = CARTESIAN_POINT ( 'NONE',  ( 756.5762568750052424, -339.1800572038740142, -348.7366044899774238 ) ) ;
#44041 = CARTESIAN_POINT ( 'NONE',  ( 781.8018195045266339, -142.2709662947837330, -365.1927285166406705 ) ) ;
#44042 = EDGE_CURVE ( 'NONE', #2736, #17707, #29034, .T. ) ;
#44043 = CARTESIAN_POINT ( 'NONE',  ( 748.9653473494363425, -410.6346026584191122, 356.9462024416521331 ) ) ;
#44045 = DIRECTION ( 'NONE',  ( 0.000000000000000000, 0.000000000000000000, 1.000000000000000000 ) ) ;
#44044 = CARTESIAN_POINT ( 'NONE',  ( 779.9999999999990905, 18.49609980828599376, 309.9999999999999432 ) ) ;
#44046 = CARTESIAN_POINT ( 'NONE',  ( 794.1144889064781864, -274.1692326535049915, -360.9840315886528401 ) ) ;
#44047 = CARTESIAN_POINT ( 'NONE',  ( 755.8990559732751535, -131.4636090269711985, -365.9055244015606831 ) ) ;
#44048 = DIRECTION ( 'NONE',  ( -0.000000000000000000, 1.000000000000000000, -0.000000000000000000 ) ) ;
#44049 = CYLINDRICAL_SURFACE ( 'NONE', #2371, 6.119000000000013095 ) ;
#44050 = CARTESIAN_POINT ( 'NONE',  ( 763.0428371773158460, -299.4636090269707438, 358.7617431975195359 ) ) ;
#44051 = CARTESIAN_POINT ( 'NONE',  ( 771.1735550268778070, -177.1800572038744690, 316.3353852180827630 ) ) ;
#44052 = ORIENTED_EDGE ( 'NONE', *, *, #8646, .T. ) ;
#44053 = CARTESIAN_POINT ( 'NONE',  ( 747.6481478633932056, -277.0999726633344267, 353.4146539503763620 ) ) ;
#44054 = CARTESIAN_POINT ( 'NONE',  ( 745.0891759886404770, -148.2709662947837330, -342.4968714119734159 ) ) ;
#44055 = CARTESIAN_POINT ( 'NONE',  ( 758.7867965644026071, 16.45630643248849267, -318.7867965644036303 ) ) ;
#44056 = CARTESIAN_POINT ( 'NONE',  ( 748.6759233522253680, -64.37269993606231822, 324.3348316497537098 ) ) ;
#44058 = VECTOR ( 'NONE', #28559, 1000.000000000000000 ) ;
#44057 = CARTESIAN_POINT ( 'NONE',  ( 812.7932403749906598, -255.1800572038742700, -327.7687537140311633 ) ) ;
#44059 = DIRECTION ( 'NONE',  ( 1.000000000000000000, 0.000000000000000000, -0.000000000000000000 ) ) ;
#44060 = EDGE_CURVE ( 'NONE', #4703, #45720, #39358, .T. ) ;
#44061 = CARTESIAN_POINT ( 'NONE',  ( 759.7806653035534055, -150.9982390220563957, 324.8639956371180801 ) ) ;
#44062 = ORIENTED_EDGE ( 'NONE', *, *, #988, .T. ) ;
#44063 = CARTESIAN_POINT ( 'NONE',  ( 814.8230680027162407, -341.8055962898683333, -333.7305795820267917 ) ) ;
#44064 = AXIS2_PLACEMENT_3D ( 'NONE', #19714, #8416, #1920 ) ;
#44065 = CARTESIAN_POINT ( 'NONE',  ( 744.7301800767019131, -76.81642084023845030, -337.4774526936615757 ) ) ;
#44066 = CARTESIAN_POINT ( 'NONE',  ( 769.9779781133707957, -19.09997266333520116, 316.7813123517150871 ) ) ;
#44067 = CARTESIAN_POINT ( 'NONE',  ( 759.0252816721024374, -360.9982390220557704, -368.0189434323527280 ) ) ;
#44068 = DIRECTION ( 'NONE',  ( 1.644774851296528363E-16, -1.000000000000000000, 0.000000000000000000 ) ) ;
#44069 = CARTESIAN_POINT ( 'NONE',  ( 787.6308680596127942, -395.2601417444136587, 364.1105419155492768 ) ) ;
#44070 = ORIENTED_EDGE ( 'NONE', *, *, #20206, .T. ) ;
#44071 = CARTESIAN_POINT ( 'NONE',  ( 758.0141637701419768, -135.0783235625962959, -367.2620300519063790 ) ) ;
#44072 = CARTESIAN_POINT ( 'NONE',  ( 791.7608162188021197, 178.9475563372491251, 320.0000000000000000 ) ) ;
#44073 = CARTESIAN_POINT ( 'NONE',  ( 788.7631598425961101, -241.4419599262322720, 305.7194118038759143 ) ) ;
#44074 = CARTESIAN_POINT ( 'NONE',  ( 762.3223304703356007, -103.5436935675111272, 322.3223304703362828 ) ) ;
#44075 = ORIENTED_EDGE ( 'NONE', *, *, #37114, .F. ) ;
#44076 = ORIENTED_EDGE ( 'NONE', *, *, #26922, .F. ) ;
#44077 = CARTESIAN_POINT ( 'NONE',  ( 784.0799538623451781, -11.80559628986942577, -364.6971507214555572 ) ) ;
#44078 = CARTESIAN_POINT ( 'NONE',  ( 755.3201227861273992, -219.7255117493289447, 345.3687786644892981 ) ) ;
#44079 = CARTESIAN_POINT ( 'NONE',  ( 793.9861285913068514, -442.9180389616178672, -372.1637643035757606 ) ) ;
#44080 = CARTESIAN_POINT ( 'NONE',  ( 939.9999999999992042, 74.99999999999984368, 360.0000000000000000 ) ) ;
#44081 = EDGE_CURVE ( 'NONE', #10220, #45456, #13114, .T. ) ;
#44082 = ORIENTED_EDGE ( 'NONE', *, *, #20764, .T. ) ;
#44083 = ORIENTED_EDGE ( 'NONE', *, *, #41717, .F. ) ;
#44084 = CARTESIAN_POINT ( 'NONE',  ( 799.9636004259356241, -382.9181544815159555, -311.2241431872006956 ) ) ;
#44085 = EDGE_CURVE ( 'NONE', #21104, #27172, #23023, .T. ) ;
#44086 = CARTESIAN_POINT ( 'NONE',  ( 749.2812353651451076, -318.4527844766014368, 323.2262854647983090 ) ) ;
#44087 = CARTESIAN_POINT ( 'NONE',  ( 778.7502325331095108, -48.35105083532386061, 304.6391490659818828 ) ) ;
#44088 =( REPRESENTATION_RELATIONSHIP ('NONE','NONE', #39835, #27662 ) REPRESENTATION_RELATIONSHIP_WITH_TRANSFORMATION ( #863 )SHAPE_REPRESENTATION_RELATIONSHIP( ) );
#44089 = CARTESIAN_POINT ( 'NONE',  ( 754.7162404726377645, -230.7363362996981664, -339.4709603349214717 ) ) ;
#44090 = CARTESIAN_POINT ( 'NONE',  ( 797.8594530101008786, -229.5436935675106440, -322.1405469898980982 ) ) ;
#44091 = CARTESIAN_POINT ( 'NONE',  ( 794.9819416627830151, -396.9982390220556567, -319.9864689768909898 ) ) ;
#44092 = ORIENTED_EDGE ( 'NONE', *, *, #41342, .F. ) ;
#44093 = CARTESIAN_POINT ( 'NONE',  ( 755.5713283507202505, -197.3618753856926560, 334.6858677611754729 ) ) ;
#44094 = CARTESIAN_POINT ( 'NONE',  ( 774.6858677611749044, -105.7255117493293000, -315.5713283507209894 ) ) ;
#44095 = ORIENTED_EDGE ( 'NONE', *, *, #30571, .F. ) ;
#44096 = AXIS2_PLACEMENT_3D ( 'NONE', #1422, #29604, #12053 ) ;
#44097 = CARTESIAN_POINT ( 'NONE',  ( 767.6429770376289525, -321.1800572038740142, 306.8695393053162093 ) ) ;
#44098 = CARTESIAN_POINT ( 'NONE',  ( 1820.038553321469863, 240.0000000000001990, 201.9999999999999716 ) ) ;
#44099 = LINE ( 'NONE', #12463, #24839 ) ;
#44100 = DIRECTION ( 'NONE',  ( -0.000000000000000000, 1.000000000000000000, -0.000000000000000000 ) ) ;
#44101 = CARTESIAN_POINT ( 'NONE',  ( 798.5707757039680246, -197.4636090269709996, 356.7845633553585003 ) ) ;
#44102 = CARTESIAN_POINT ( 'NONE',  ( 757.8323909638827445, -74.63460265842032015, 352.1044303154654358 ) ) ;
#44103 = ORIENTED_EDGE ( 'NONE', *, *, #23205, .T. ) ;
#44104 = CARTESIAN_POINT ( 'NONE',  ( 814.2805881961230625, -433.6454272087884760, -331.2368401574024119 ) ) ;
#44105 = CARTESIAN_POINT ( 'NONE',  ( 745.0891759886404770, -28.27096629478409540, -342.4968714119734159 ) ) ;
#44106 = CARTESIAN_POINT ( 'NONE',  ( 786.6156483768007774, -265.4419599262323004, 315.5913626894246136 ) ) ;
#44107 = CARTESIAN_POINT ( 'NONE',  ( 795.1360043628807261, -380.0891481129646650, -360.2193346964456282 ) ) ;
#44108 = CARTESIAN_POINT ( 'NONE',  ( 756.3353852180820240, -5.907329931147799584, -331.1735550268787733 ) ) ;
#44109 = CARTESIAN_POINT ( 'NONE',  ( 787.5162901302840055, -419.3618753856918033, 305.4481719005792684 ) ) ;
#44110 = LINE ( 'NONE', #12474, #19567 ) ;
#44111 = CARTESIAN_POINT ( 'NONE',  ( 760.7433823573367135, -276.0090635724253048, -355.9930595647440441 ) ) ;
#44112 = CARTESIAN_POINT ( 'NONE',  ( 763.2262854647970016, -152.6346026584200786, -309.2812353651462445 ) ) ;
#44113 = CARTESIAN_POINT ( 'NONE',  ( 755.2512626584698410, -55.54369356751127640, 315.2512626584710915 ) ) ;
#44114 = CARTESIAN_POINT ( 'NONE',  ( 808.0189434323515343, -158.0891481129655176, 319.0252816721025511 ) ) ;
#44115 = CARTESIAN_POINT ( 'NONE',  ( 831.1634899080286232, 258.0939999999998804, -199.9999999999999432 ) ) ;
#44116 = LINE ( 'NONE', #2297, #41659 ) ;
#44117 = CARTESIAN_POINT ( 'NONE',  ( 998.9999999999992042, 478.9999999999999432, 0.000000000000000000 ) ) ;
#44118 = CARTESIAN_POINT ( 'NONE',  ( 815.2698199232961542, -376.8164208402375834, 342.5225473063383106 ) ) ;
#44119 = CARTESIAN_POINT ( 'NONE',  ( 803.6646147819161570, -353.9073299311467053, -348.8264449731210561 ) ) ;
#44120 = CARTESIAN_POINT ( 'NONE',  ( 793.2243759319678702, 21.46713098285774279, 318.4439275373583200 ) ) ;
#44121 = CARTESIAN_POINT ( 'NONE',  ( 791.0478386215596629, -93.82724539060770041, -306.7653713866226326 ) ) ;
#44122 = CARTESIAN_POINT ( 'NONE',  ( 805.1016975059191054, -102.8965053807782368, -343.0745993439771837 ) ) ;
#44123 = CARTESIAN_POINT ( 'NONE',  ( 814.8230680027162407, -149.8055962898689870, 333.7305795820267917 ) ) ;
#44124 = CARTESIAN_POINT ( 'NONE',  ( 794.9819416627830151, 11.00176097794305541, 319.9864689768909898 ) ) ;
#44125 = AXIS2_PLACEMENT_3D ( 'NONE', #700, #25395, #31863 ) ;
#44126 = CARTESIAN_POINT ( 'NONE',  ( 804.9363028652555840, -40.27096629478405987, -338.2165204200192079 ) ) ;
#44127 = CARTESIAN_POINT ( 'NONE',  ( 799.4546378042377910, -129.0783235625963243, -356.1575198192848006 ) ) ;
#44128 = CARTESIAN_POINT ( 'NONE',  ( 804.4286716492782716, -137.3618753856928265, -345.3141322388244703 ) ) ;
#44129 = CARTESIAN_POINT ( 'NONE',  ( 762.1405469898971887, -121.5436935675110419, 357.8594530101015607 ) ) ;
#44130 = ADVANCED_FACE ( 'NONE', ( #12874 ), #33888, .F. ) ;
#44131 = CARTESIAN_POINT ( 'NONE',  ( 808.7758568127978833, 19.83076734649410966, -320.0363995740631822 ) ) ;
#44133 = CARTESIAN_POINT ( 'NONE',  ( 759.7806653035535192, -246.9982390220560831, 324.8639956371181370 ) ) ;
#44132 = CARTESIAN_POINT ( 'NONE',  ( 778.1981804954714335, -298.2709662947830793, 314.8072714833589885 ) ) ;
#44134 = DIRECTION ( 'NONE',  ( 0.000000000000000000, 1.000000000000000000, -0.000000000000000000 ) ) ;
#44135 = VERTEX_POINT ( 'NONE', #12642 ) ;
#44136 = CARTESIAN_POINT ( 'NONE',  ( 769.1273215169530886, 1.285312801039623753, 317.4527132478988847 ) ) ;
#44137 = CARTESIAN_POINT ( 'NONE',  ( 776.2046728542105711, -260.1908817542435486, -304.8212110874238761 ) ) ;
#44138 = EDGE_LOOP ( 'NONE', ( #38952, #34383 ) ) ;
#44139 = APPLICATION_PROTOCOL_DEFINITION ( 'draft international standard', 'automotive_design', 1998, #8103 ) ;
#44140 = ADVANCED_FACE ( 'NONE', ( #37356 ), #37115, .F. ) ;
#44141 = CARTESIAN_POINT ( 'NONE',  ( 801.1904061080338124, -236.0891481129652334, 368.3070685750236066 ) ) ;
#44142 = CARTESIAN_POINT ( 'NONE',  ( 802.9823548866075953, -289.0999726633343698, 330.0799878456151077 ) ) ;
#44143 = CARTESIAN_POINT ( 'NONE',  ( 758.6633372737375112, -404.5328690171409107, 326.9102291470432533 ) ) ;
#44144 = VERTEX_POINT ( 'NONE', #23480 ) ;
#44145 = CARTESIAN_POINT ( 'NONE',  ( 801.5560724626406000, -120.5545181178803205, -326.7756240680316182 ) ) ;
#44146 = CARTESIAN_POINT ( 'NONE',  ( 765.0180583372156207, -120.9982390220565378, -360.0135310231089534 ) ) ;
#44147 = CARTESIAN_POINT ( 'NONE',  ( 774.6858677611749044, -297.7255117493286889, -315.5713283507209894 ) ) ;
#44148 = EDGE_LOOP ( 'NONE', ( #16803, #21328 ) ) ;
#44149 = CARTESIAN_POINT ( 'NONE',  ( 804.9363028652555840, -424.2709662947829088, -338.2165204200192079 ) ) ;
#44150 = CARTESIAN_POINT ( 'NONE',  ( 768.0187753319979720, -80.63460265842029173, -318.0580252608186242 ) ) ;
#44151 = CARTESIAN_POINT ( 'NONE',  ( 764.0069404352550464, -303.0783235625957559, 359.2566176426627180 ) ) ;
#44152 = CARTESIAN_POINT ( 'NONE',  ( 51.16348990802859475, 240.0000000000000568, -202.7499999999943441 ) ) ;
#44153 = CYLINDRICAL_SURFACE ( 'NONE', #13792, 9.999999999999980460 ) ;
#44154 = DIRECTION ( 'NONE',  ( 0.000000000000000000, -1.000000000000000000, 0.000000000000000000 ) ) ;
#44155 = EDGE_LOOP ( 'NONE', ( #12554, #2021 ) ) ;
#44156 = CARTESIAN_POINT ( 'NONE',  ( 799.9636004259356241, -334.9181544815160692, -311.2241431872006956 ) ) ;
#44157 = ADVANCED_FACE ( 'NONE', ( #33666 ), #2469, .F. ) ;
#44158 = CARTESIAN_POINT ( 'NONE',  ( 797.8822607201568644, -198.5545181178800647, 370.1134526219340160 ) ) ;
#44159 = AXIS2_PLACEMENT_3D ( 'NONE', #23371, #36399, #26232 ) ;
#44161 = CARTESIAN_POINT ( 'NONE',  ( 788.7366044899766848, -299.9073299311468759, -316.5762568750059813 ) ) ;
#44160 = DIRECTION ( 'NONE',  ( 0.000000000000000000, 0.000000000000000000, -1.000000000000000000 ) ) ;
#44162 = EDGE_CURVE ( 'NONE', #9315, #1111, #30495, .T. ) ;
#44163 = DIRECTION ( 'NONE',  ( -1.000000000000000000, -0.000000000000000000, -0.000000000000000000 ) ) ;
#44164 = CARTESIAN_POINT ( 'NONE',  ( 804.4086373105744769, -193.6454272087891582, -333.3843516231986541 ) ) ;
#44165 = ADVANCED_FACE ( 'NONE', ( #22808 ), #36901, .T. ) ;
#44166 = CARTESIAN_POINT ( 'NONE',  ( 805.0032342141412300, -37.54369356751132614, 314.9967657858571783 ) ) ;
#44167 = CYLINDRICAL_SURFACE ( 'NONE', #24030, 19.99999999999990763 ) ;
#44168 = CARTESIAN_POINT ( 'NONE',  ( 772.5602148656447525, -369.7255117493284615, -305.7998596910095443 ) ) ;
#44169 = DIRECTION ( 'NONE',  ( 0.000000000000000000, -0.3826834323650837866, -0.9238795325112891810 ) ) ;
#44170 = CARTESIAN_POINT ( 'NONE',  ( 771.1735550268778070, -57.18005720387489532, 316.3353852180827630 ) ) ;
#44171 = CARTESIAN_POINT ( 'NONE',  ( 757.7880784355613741, -306.0090635724252479, 312.4576283171834916 ) ) ;
#44172 = CARTESIAN_POINT ( 'NONE',  ( 792.2312462859673587, -251.9073299311470748, 307.2067596250082602 ) ) ;
#44173 = CARTESIAN_POINT ( 'NONE',  ( 749.2812353651451076, -30.45278447660226817, -323.2262854647983090 ) ) ;
#44174 = CARTESIAN_POINT ( 'NONE',  ( 939.9999999999993179, -418.3138125091625170, 201.9999999999998863 ) ) ;
#44175 = DIRECTION ( 'NONE',  ( -0.000000000000000000, 1.000000000000000000, -0.000000000000000000 ) ) ;
#44176 = CARTESIAN_POINT ( 'NONE',  ( 800.2193346964447755, -354.9982390220557704, 355.1360043628815788 ) ) ;
#44177 = CARTESIAN_POINT ( 'NONE',  ( 760.7433823573367135, -132.0090635724257595, 355.9930595647440441 ) ) ;
#44178 = CARTESIAN_POINT ( 'NONE',  ( 776.9566956441375396, -12.89650538077851216, -364.8461984189686405 ) ) ;
#44179 = CARTESIAN_POINT ( 'NONE',  ( 919.9999999999993179, 219.9999999999998863, 350.0000000000000000 ) ) ;
#44180 = EDGE_CURVE ( 'NONE', #29887, #23669, #1773, .T. ) ;
#44181 = LINE ( 'NONE', #4941, #45442 ) ;
#44182 = CARTESIAN_POINT ( 'NONE',  ( 813.9316612368132837, -127.4419599262326983, 348.6739635108323228 ) ) ;
#44183 = CARTESIAN_POINT ( 'NONE',  ( 804.4286716492782716, -401.3618753856920307, 345.3141322388244703 ) ) ;
#44184 = ORIENTED_EDGE ( 'NONE', *, *, #2106, .F. ) ;
#44185 = CARTESIAN_POINT ( 'NONE',  ( 801.9419747391806368, -42.45278447660223264, -351.9812246680014027 ) ) ;
#44186 = ADVANCED_FACE ( 'NONE', ( #34793 ), #6409, .F. ) ;
#44187 = CARTESIAN_POINT ( 'NONE',  ( 760.5453621957607311, -333.0783235625956991, -323.8424801807151425 ) ) ;
#44189 = CARTESIAN_POINT ( 'NONE',  ( 754.8072714833583632, -172.8164208402381519, 338.1981804954721156 ) ) ;
#44188 = CARTESIAN_POINT ( 'NONE',  ( 755.5713283507202505, -173.3618753856927128, 334.6858677611754729 ) ) ;
#44190 = CARTESIAN_POINT ( 'NONE',  ( 756.1443688327750579, -333.6237781080502600, -314.3581564841659315 ) ) ;
#44191 = DIRECTION ( 'NONE',  ( 1.000000000000000000, 0.000000000000000000, -0.000000000000000000 ) ) ;
#44192 = ADVANCED_BREP_SHAPE_REPRESENTATION ( '', ( #31946, #26858 ), #27503 ) ;
#44193 = EDGE_LOOP ( 'NONE', ( #6898, #34068 ) ) ;
#44194 = CARTESIAN_POINT ( 'NONE',  ( 794.9819416627830151, -348.9982390220558273, 319.9864689768909898 ) ) ;
#44195 = CIRCLE ( 'NONE', #24273, 7.999999999999896083 ) ;
#44196 = ORIENTED_EDGE ( 'NONE', *, *, #45351, .F. ) ;
#44197 = CARTESIAN_POINT ( 'NONE',  ( -784.4999999999993179, -359.5698779088871788, -26.28906389436296109 ) ) ;
#44198 = EDGE_CURVE ( 'NONE', #22109, #37078, #43747, .T. ) ;
#44199 = EDGE_CURVE ( 'NONE', #4508, #42212, #17721, .T. ) ;
#44200 = CARTESIAN_POINT ( 'NONE',  ( 811.0346526505616112, -182.6346026584199649, -323.0537975583477532 ) ) ;
#44201 = CARTESIAN_POINT ( 'NONE',  ( 792.2312462859673587, -131.9073299311473875, 307.2067596250082602 ) ) ;
#44202 = ORIENTED_EDGE ( 'NONE', *, *, #26039, .T. ) ;
#44203 = CARTESIAN_POINT ( 'NONE',  ( 803.6646147819162707, -185.9073299311472169, -348.8264449731211130 ) ) ;
#44204 = VERTEX_POINT ( 'NONE', #35024 ) ;
#44205 = CARTESIAN_POINT ( 'NONE',  ( 805.2837595273609850, -458.7363362996973706, -340.5290396650784714 ) ) ;
#44206 = CARTESIAN_POINT ( 'NONE',  ( 748.9653473494363425, -242.6346026584197659, 356.9462024416521331 ) ) ;
#44207 = CARTESIAN_POINT ( 'NONE',  ( 770.0799878456142551, -181.9874144716870887, 362.9823548866085616 ) ) ;
#44210 = CARTESIAN_POINT ( 'NONE',  ( 815.0009284576459549, -414.3510508353227237, 338.7629533639073429 ) ) ;
#44209 = FACE_OUTER_BOUND ( 'NONE', #30893, .T. ) ;
#44208 = DIRECTION ( 'NONE',  ( 0.000000000000000000, 0.9235249282889854694, -0.3835384033298675499 ) ) ;
#44211 = ORIENTED_EDGE ( 'NONE', *, *, #13072, .T. ) ;
#44212 = CARTESIAN_POINT ( 'NONE',  ( 769.0155153010367712, -418.3726999360612808, -362.7791456095907279 ) ) ;
#44213 = DIRECTION ( 'NONE',  ( -1.000000000000000000, -0.000000000000000000, -0.000000000000000000 ) ) ;
#44214 = ORIENTED_EDGE ( 'NONE', *, *, #12264, .F. ) ;
#44215 = CARTESIAN_POINT ( 'NONE',  ( 747.6481478633932056, -229.0999726633345404, -353.4146539503763620 ) ) ;
#44216 = CARTESIAN_POINT ( 'NONE',  ( 815.3608509340175488, -98.73633629969859271, 341.2497674668889545 ) ) ;
#44218 = CARTESIAN_POINT ( 'NONE',  ( 804.9363028652555840, -184.2709662947835909, -338.2165204200192079 ) ) ;
#44217 = DIRECTION ( 'NONE',  ( -1.000000000000000000, -0.000000000000000000, -0.000000000000000000 ) ) ;
#44219 = CARTESIAN_POINT ( 'NONE',  ( 787.6308680596127942, -347.2601417444138860, -364.1105419155492768 ) ) ;
#44220 = DIRECTION ( 'NONE',  ( 0.000000000000000000, 0.000000000000000000, -1.000000000000000000 ) ) ;
#44221 = CARTESIAN_POINT ( 'NONE',  ( 745.5313806188320314, -231.2817908451527558, -333.7943932421247268 ) ) ;
#44222 = DIRECTION ( 'NONE',  ( -0.000000000000000000, -0.000000000000000000, 1.000000000000000000 ) ) ;
#44223 = DIRECTION ( 'NONE',  ( 0.000000000000000000, -0.3826834323650838976, -0.9238795325112892920 ) ) ;
#44224 = CARTESIAN_POINT ( 'NONE',  ( 755.1538015810308480, -62.19088175424416676, -343.0433043558613804 ) ) ;
#44225 = CARTESIAN_POINT ( 'NONE',  ( 779.4763451958990572, -440.7363362996975980, 365.0264073115438919 ) ) ;
#44226 = CARTESIAN_POINT ( 'NONE',  ( 768.9521613784389729, -369.8272453906068904, 373.2346286133773106 ) ) ;
#44227 = CARTESIAN_POINT ( 'NONE',  ( 763.2154366446407039, -429.6237781080499190, -321.4292242960311228 ) ) ;
#44228 = CARTESIAN_POINT ( 'NONE',  ( 751.6929314249750860, -270.9982390220561115, -318.8095938919659034 ) ) ;
#44229 = CARTESIAN_POINT ( 'NONE',  ( 786.5483106153019435, -247.6454272087890160, 364.1601925771022366 ) ) ;
#44230 = FACE_OUTER_BOUND ( 'NONE', #5714, .T. ) ;
#44231 = DIRECTION ( 'NONE',  ( -0.000000000000000000, -0.000000000000000000, 1.000000000000000000 ) ) ;
#44232 = CARTESIAN_POINT ( 'NONE',  ( 762.1405469898971887, -49.54369356751129061, -357.8594530101015607 ) ) ;
#44233 = AXIS2_PLACEMENT_3D ( 'NONE', #19729, #36207, #14974 ) ;
#44234 = CARTESIAN_POINT ( 'NONE',  ( 762.1177392798416577, -210.5545181178800647, 309.8865473780659272 ) ) ;
#44235 = CARTESIAN_POINT ( 'NONE',  ( 783.7566961878529810, -144.8965053807781089, -305.1792804349288417 ) ) ;
#44236 = CARTESIAN_POINT ( 'NONE',  ( 745.7998596910086917, -149.3618753856928265, 332.5602148656461168 ) ) ;
#44237 = CARTESIAN_POINT ( 'NONE',  ( 805.0032342141412300, -397.5436935675100472, -314.9967657858571783 ) ) ;
#44238 = DIRECTION ( 'NONE',  ( -1.000000000000000000, -0.000000000000000000, -0.000000000000000000 ) ) ;
#44239 = CARTESIAN_POINT ( 'NONE',  ( 778.2165204200184689, -262.8164208402379245, 364.9363028652563230 ) ) ;
#44240 = CARTESIAN_POINT ( 'NONE',  ( 790.0220218866281812, -7.099972663335241130, 363.2186876482849129 ) ) ;
#44241 = CARTESIAN_POINT ( 'NONE',  ( 785.3141322388236176, -405.7255117493283478, -364.4286716492789537 ) ) ;
#44242 = CARTESIAN_POINT ( 'NONE',  ( 939.9999999999992042, 74.99999999999984368, 360.0000000000000000 ) ) ;
#44243 = EDGE_CURVE ( 'NONE', #35615, #43930, #242, .T. ) ;
#44244 = CARTESIAN_POINT ( 'NONE',  ( 757.7880784355613741, -18.00906357242611477, -312.4576283171834916 ) ) ;
#44245 = LINE ( 'NONE', #19523, #25480 ) ;
#44246 = CARTESIAN_POINT ( 'NONE',  ( 776.9566956441375396, -84.89650538077830788, 364.8461984189686405 ) ) ;
#44247 = ORIENTED_EDGE ( 'NONE', *, *, #42455, .T. ) ;
#44248 = CARTESIAN_POINT ( 'NONE',  ( 755.0488828828309806, -233.8055962898687028, -344.1219089521771934 ) ) ;
#44249 = CARTESIAN_POINT ( 'NONE',  ( 764.8639956371174549, -128.0891481129655176, -319.7806653035542013 ) ) ;
#44250 = CARTESIAN_POINT ( 'NONE',  ( 762.1405469898971887, -49.54369356751129061, 357.8594530101015607 ) ) ;
#44251 = CARTESIAN_POINT ( 'NONE',  ( 803.8556311672234642, -225.6237781080506011, -365.6418435158340117 ) ) ;
#44252 = CARTESIAN_POINT ( 'NONE',  ( 784.4999999999993179, -365.3551492539851893, -8.132432514707076621 ) ) ;
#44253 = CARTESIAN_POINT ( 'NONE',  ( 814.8230680027162407, -389.8055962898682765, 333.7305795820267917 ) ) ;
#44254 = EDGE_LOOP ( 'NONE', ( #17050, #28713, #5636, #3366, #16719, #17916 ) ) ;
#44255 = CARTESIAN_POINT ( 'NONE',  ( 745.4481719005789273, -3.725511749329622813, 347.5162901302853129 ) ) ;
#44256 = CARTESIAN_POINT ( 'NONE',  ( 804.4286716492782716, -185.3618753856926844, -345.3141322388244703 ) ) ;
#44257 = CARTESIAN_POINT ( 'NONE',  ( 778.2165204200184689, -382.8164208402374697, 364.9363028652563230 ) ) ;
#44258 = EDGE_CURVE ( 'NONE', #12793, #10247, #34146, .T. ) ;
#44259 = CARTESIAN_POINT ( 'NONE',  ( 796.7737145352015204, -68.63460265842033436, -370.7187646348536987 ) ) ;
#44260 = CARTESIAN_POINT ( 'NONE',  ( 756.3353852180820240, -77.90732993114757221, -331.1735550268787733 ) ) ;
#44261 = ORIENTED_EDGE ( 'NONE', *, *, #19848, .F. ) ;
#44262 = CARTESIAN_POINT ( 'NONE',  ( 802.5472867521000353, -4.372699936062523385, -350.8726784830461156 ) ) ;
#44263 = ORIENTED_EDGE ( 'NONE', *, *, #4417, .T. ) ;
#44264 = CARTESIAN_POINT ( 'NONE',  ( 769.0155153010367712, -370.3726999360613377, -362.7791456095907279 ) ) ;
#44266 = CARTESIAN_POINT ( 'NONE',  ( 793.0897708529556667, -390.5545181178794678, 361.3366627262616362 ) ) ;
#44265 = CARTESIAN_POINT ( 'NONE',  ( 804.9363028652555840, -88.27096629478390355, 338.2165204200192079 ) ) ;
#44269 = CARTESIAN_POINT ( 'NONE',  ( 798.0661480581538854, -338.5328690171411381, 309.5768839229118043 ) ) ;
#44268 = CARTESIAN_POINT ( 'NONE',  ( 989.9999999999992042, -431.4567479753240491, 350.0000000000000000 ) ) ;
#44267 = CARTESIAN_POINT ( 'NONE',  ( 808.0189434323515343, -422.0891481129647218, 319.0252816721025511 ) ) ;
#44270 = CARTESIAN_POINT ( 'NONE',  ( 798.0661480581538854, -122.5328690171417918, 309.5768839229118043 ) ) ;
#44271 = CARTESIAN_POINT ( 'NONE',  ( 804.1105419155481968, -339.8272453906069472, -347.6308680596136469 ) ) ;
#44272 = CARTESIAN_POINT ( 'NONE',  ( 754.8072714833581358, -316.8164208402377540, -338.1981804954720587 ) ) ;
#44273 = CARTESIAN_POINT ( 'NONE',  ( 781.8018195045266339, -166.2709662947835909, -365.1927285166406705 ) ) ;
#44274 = CARTESIAN_POINT ( 'NONE',  ( 746.4236121716829757, -15.82724539060794200, 328.8385539511384650 ) ) ;
#44276 = LINE ( 'NONE', #12414, #44773 ) ;
#44275 = DIRECTION ( 'NONE',  ( -1.880165489482579047E-16, -1.000000000000000000, -0.000000000000000000 ) ) ;
#44277 = CARTESIAN_POINT ( 'NONE',  ( 764.0069404352550464, -255.0783235625958980, -359.2566176426627180 ) ) ;
#44278 = CARTESIAN_POINT ( 'NONE',  ( 748.6759233522253680, -112.3726999360621761, -324.3348316497537098 ) ) ;
#44279 = CARTESIAN_POINT ( 'NONE',  ( -180.7583438952258348, 394.6698570112193920, -274.9999999999999432 ) ) ;
#44280 = LINE ( 'NONE', #2464, #33371 ) ;
#44281 = CARTESIAN_POINT ( 'NONE',  ( 798.5707757039680246, -317.4636090269706301, 356.7845633553585003 ) ) ;
#44282 = CARTESIAN_POINT ( 'NONE',  ( 756.5762568750052424, -171.1800572038745543, 348.7366044899774238 ) ) ;
#44283 = EDGE_LOOP ( 'NONE', ( #34481, #44787, #2807, #34075 ) ) ;
#44284 = CARTESIAN_POINT ( 'NONE',  ( 773.7305795820266212, -297.2817908451526137, 374.8230680027170365 ) ) ;
#44285 = CARTESIAN_POINT ( 'NONE',  ( 787.5162901302840055, -155.3618753856927697, -305.4481719005793252 ) ) ;
#44286 = DIRECTION ( 'NONE',  ( 0.000000000000000000, 0.000000000000000000, 1.000000000000000000 ) ) ;
#44287 = CARTESIAN_POINT ( 'NONE',  ( 799.9636004259356241, -70.91815448151683654, 311.2241431872006956 ) ) ;
#44288 = CARTESIAN_POINT ( 'NONE',  ( 811.0346526505616112, -254.6346026584196238, -323.0537975583477532 ) ) ;
#44289 = FACE_OUTER_BOUND ( 'NONE', #19818, .T. ) ;
#44290 = CARTESIAN_POINT ( 'NONE',  ( 767.7687537140311633, -215.9073299311471317, 372.7932403749916830 ) ) ;
#44291 = CARTESIAN_POINT ( 'NONE',  ( 803.4237431249931660, -159.1800572038746111, 331.2633955100225194 ) ) ;
#44292 = ORIENTED_EDGE ( 'NONE', *, *, #16579, .F. ) ;
#44293 = CARTESIAN_POINT ( 'NONE',  ( 744.8212110874229666, -354.8965053807774552, -336.2046728542121627 ) ) ;
#44294 = CARTESIAN_POINT ( 'NONE',  ( 812.7932403749906598, -87.18005720387481006, -327.7687537140311633 ) ) ;
#44295 = CARTESIAN_POINT ( 'NONE',  ( 769.9779781133707957, -67.09997266333506616, 316.7813123517150871 ) ) ;
#44296 = CARTESIAN_POINT ( 'NONE',  ( 777.4774526936600978, -346.2709662947830793, -304.7301800767027657 ) ) ;
#44297 = LINE ( 'NONE', #5052, #40192 ) ;
#44298 = CARTESIAN_POINT ( 'NONE',  ( 758.6633372737375112, -428.5328690171409107, 326.9102291470432533 ) ) ;
#44299 = ORIENTED_EDGE ( 'NONE', *, *, #4000, .T. ) ;
#44300 = CARTESIAN_POINT ( 'NONE',  ( 802.7791456095903868, -76.71468719896012090, 329.0155153010375102 ) ) ;
#44301 = CARTESIAN_POINT ( 'NONE',  ( 744.8212110874229666, -114.8965053807782226, -336.2046728542121627 ) ) ;
#44302 = DIRECTION ( 'NONE',  ( -1.000000000000000000, -0.000000000000000000, -0.000000000000000000 ) ) ;
#44303 = CARTESIAN_POINT ( 'NONE',  ( 788.7631598425961101, -289.4419599262321299, 305.7194118038759143 ) ) ;
#44304 = CARTESIAN_POINT ( 'NONE',  ( 756.3353852180820240, -77.90732993114757221, 331.1735550268787733 ) ) ;
#44305 = ORIENTED_EDGE ( 'NONE', *, *, #29910, .T. ) ;
#44306 = ORIENTED_EDGE ( 'NONE', *, *, #17642, .F. ) ;
#44307 = CARTESIAN_POINT ( 'NONE',  ( 757.2208543904082489, -16.71468719896031985, -350.9844846989624330 ) ) ;
#44308 = CARTESIAN_POINT ( 'NONE',  ( 804.6798772138708955, -279.7255117493288026, 334.6312213355107019 ) ) ;
#44309 = CARTESIAN_POINT ( 'NONE',  ( 746.7653713866222915, -425.2601417444136018, -351.0478386215610271 ) ) ;
#44310 = DIRECTION ( 'NONE',  ( 0.000000000000000000, -1.000000000000000000, 0.000000000000000000 ) ) ;
#44311 = ORIENTED_EDGE ( 'NONE', *, *, #21483, .T. ) ;
#44312 = ORIENTED_EDGE ( 'NONE', *, *, #35742, .T. ) ;
#44313 = CARTESIAN_POINT ( 'NONE',  ( 810.4231160770870019, -360.5545181178796383, -321.9338519418446936 ) ) ;
#44315 = CARTESIAN_POINT ( 'NONE',  ( 754.0944755984390895, -207.6237781080506295, 364.1009440267246760 ) ) ;
#44314 = CARTESIAN_POINT ( 'NONE',  ( 810.7187646348534145, -330.4527844766013231, 356.7737145352016341 ) ) ;
#44316 = CARTESIAN_POINT ( 'NONE',  ( 748.3538107759620743, -40.71468719896024879, 355.8262568251490165 ) ) ;
#44317 = CARTESIAN_POINT ( 'NONE',  ( 757.4527132478984868, -208.3726999360619061, -329.1273215169538844 ) ) ;
#44318 = CARTESIAN_POINT ( 'NONE',  ( 800.0135310231082713, -230.0891481129652618, -325.0180583372163028 ) ) ;
#44319 = CARTESIAN_POINT ( 'NONE',  ( 805.1927285166399315, -424.8164208402373561, -341.8018195045277707 ) ) ;
#44320 = VERTEX_POINT ( 'NONE', #45673 ) ;
#44321 = CARTESIAN_POINT ( 'NONE',  ( 781.8018195045266339, -214.2709662947834488, 365.1927285166406705 ) ) ;
#44322 = CARTESIAN_POINT ( 'NONE',  ( 756.5762568750052424, -99.18005720387478164, -348.7366044899774238 ) ) ;
#44323 = VERTEX_POINT ( 'NONE', #30886 ) ;
#44324 = CARTESIAN_POINT ( 'NONE',  ( 800.9747183278959710, -372.9982390220557704, 311.9810565676471583 ) ) ;
#44325 = CARTESIAN_POINT ( 'NONE',  ( 793.2534793918160858, 16.75597696963228955, -312.9842977579731382 ) ) ;
#44326 = CARTESIAN_POINT ( 'NONE',  ( 792.4730984305310812, 16.45630643248850333, 314.5980907654948169 ) ) ;
#44327 = CARTESIAN_POINT ( 'NONE',  ( 879.9999999999992042, 239.9999999999998295, 350.0000000000000000 ) ) ;
#44328 = CARTESIAN_POINT ( 'NONE',  ( 769.9779781133707957, -187.0999726633346825, 316.7813123517150871 ) ) ;
#44329 = CARTESIAN_POINT ( 'NONE',  ( 758.0580252608178853, -78.45278447660211896, 328.0187753319985404 ) ) ;
#44330 = VERTEX_POINT ( 'NONE', #24615 ) ;
#44331 = CARTESIAN_POINT ( 'NONE',  ( 794.5607502887775127, -462.9631818684622999, -371.8524697363486666 ) ) ;
#44332 = CARTESIAN_POINT ( 'NONE',  ( 747.2067596250078623, -27.18005720387500901, -352.2312462859687230 ) ) ;
#44333 = CARTESIAN_POINT ( 'NONE',  ( 772.3691319403857278, -263.2601417444141134, 315.8894580844506663 ) ) ;
#44334 = CARTESIAN_POINT ( 'NONE',  ( 764.8639956371174549, -392.0891481129648355, -319.7806653035542013 ) ) ;
#44335 = CARTESIAN_POINT ( 'NONE',  ( 778.1981804954715471, -10.27096629478415046, -314.8072714833591021 ) ) ;
#44336 = CARTESIAN_POINT ( 'NONE',  ( 808.3070685750230950, -426.9982390220554862, 361.1904061080339261 ) ) ;
#44337 = DIRECTION ( 'NONE',  ( -1.000000000000000000, -0.000000000000000000, 0.000000000000000000 ) ) ;
#44338 = CARTESIAN_POINT ( 'NONE',  ( 780.5236548040995785, -284.7363362996979390, -314.9735926884559944 ) ) ;
#44339 = CARTESIAN_POINT ( 'NONE',  ( 772.4837098697144029, -167.3618753856927412, -374.5518280994205611 ) ) ;
#44340 = CARTESIAN_POINT ( 'NONE',  ( 767.6429770376289525, -81.18005720387481006, 306.8695393053162093 ) ) ;
#44341 = CARTESIAN_POINT ( 'NONE',  ( 746.8695393053150156, -149.9073299311473875, 327.6429770376306010 ) ) ;
#44342 = DIRECTION ( 'NONE',  ( -0.000000000000000000, 1.000000000000000000, -0.000000000000000000 ) ) ;
#44343 = CARTESIAN_POINT ( 'NONE',  ( -728.8365100919714905, 256.5000000000001705, -206.1189999999890574 ) ) ;
#44344 = CARTESIAN_POINT ( 'NONE',  ( 791.1614460488616487, -227.2601417444141987, -373.5763878283158874 ) ) ;
#44345 = DIRECTION ( 'NONE',  ( -1.000000000000000000, 0.000000000000000000, 0.000000000000000000 ) ) ;
#44346 = CARTESIAN_POINT ( 'NONE',  ( 758.8095938919642549, -392.0891481129648355, 311.6929314249763365 ) ) ;
#44347 = CARTESIAN_POINT ( 'NONE',  ( 796.7737145352015204, -20.63460265842048003, 370.7187646348536987 ) ) ;
#44348 = CARTESIAN_POINT ( 'NONE',  ( 804.4286716492782716, -353.3618753856922012, -345.3141322388244703 ) ) ;
#44349 = CARTESIAN_POINT ( 'NONE',  ( 770.0799878456142551, 10.01258552831232329, 362.9823548866085616 ) ) ;
#44350 = CARTESIAN_POINT ( 'NONE',  ( 757.7880784355613741, -114.0090635724258163, -312.4576283171834916 ) ) ;
#44351 = CARTESIAN_POINT ( 'NONE',  ( 804.9511171171677688, -149.8055962898689870, -335.8780910478229202 ) ) ;
#44352 = CARTESIAN_POINT ( 'NONE',  ( 812.6845335610512393, -151.9874144716871740, 353.5525998758768651 ) ) ;
#44353 = CARTESIAN_POINT ( 'NONE',  ( 181.1634899080285948, 240.0000000000000284, -199.9999999999953957 ) ) ;
#44354 = CARTESIAN_POINT ( 'NONE',  ( 800.0135310231082713, -62.08914811296580183, -325.0180583372163028 ) ) ;
#44355 = CARTESIAN_POINT ( 'NONE',  ( 780.5290396650775619, -156.3510508353235480, -365.2837595273619513 ) ) ;
#44356 = CARTESIAN_POINT ( 'NONE',  ( 754.8072714833581358, -124.8164208402383508, -338.1981804954720587 ) ) ;
#44357 = CARTESIAN_POINT ( 'NONE',  ( 804.9363028652555840, -160.2709662947836762, 338.2165204200192079 ) ) ;
#44358 = CARTESIAN_POINT ( 'NONE',  ( 812.6845335610512393, -7.987414471687621642, -353.5525998758768651 ) ) ;
#44360 = CARTESIAN_POINT ( 'NONE',  ( 800.2193346964446619, -306.9982390220558841, 355.1360043628816925 ) ) ;
#44359 = CARTESIAN_POINT ( 'NONE',  ( 795.1360043628807261, -284.0891481129650629, 360.2193346964456282 ) ) ;
#44361 = CIRCLE ( 'NONE', #24443, 8.025000000000003908 ) ;
#44362 = CARTESIAN_POINT ( 'NONE',  ( -115.7583438952258774, 290.0000000000001137, -320.0000000000000568 ) ) ;
#44363 = ORIENTED_EDGE ( 'NONE', *, *, #13974, .T. ) ;
#44364 = CARTESIAN_POINT ( 'NONE',  ( 803.2186876482843445, -7.987414471687621642, 350.0220218866286928 ) ) ;
#44365 = CARTESIAN_POINT ( 'NONE',  ( 810.4231160770870019, -264.5545181178798657, -321.9338519418446936 ) ) ;
#44366 = ORIENTED_EDGE ( 'NONE', *, *, #42448, .F. ) ;
#44367 = APPLICATION_PROTOCOL_DEFINITION ( 'draft international standard', 'automotive_design', 1998, #10433 ) ;
#44368 = CARTESIAN_POINT ( 'NONE',  ( 748.9653473494365699, -218.6346026584198228, 356.9462024416520762 ) ) ;
#44369 = CARTESIAN_POINT ( 'NONE',  ( 801.5560724626406000, -288.5545181178798657, 326.7756240680316182 ) ) ;
#44370 = CARTESIAN_POINT ( 'NONE',  ( 793.2243759319678702, -410.5328690171408539, 318.4439275373583200 ) ) ;
#44371 = ORIENTED_EDGE ( 'NONE', *, *, #7195, .F. ) ;
#44372 = CARTESIAN_POINT ( 'NONE',  ( 798.5707757039680246, -101.4636090269713264, -356.7845633553585003 ) ) ;
#44373 = CARTESIAN_POINT ( 'NONE',  ( 805.1927285166397041, -112.8164208402383508, -341.8018195045277707 ) ) ;
#44374 = CARTESIAN_POINT ( 'NONE',  ( 762.3223304703356007, -319.5436935675104451, -322.3223304703362828 ) ) ;
#44375 = ORIENTED_EDGE ( 'NONE', *, *, #31981, .F. ) ;
#44376 = CARTESIAN_POINT ( 'NONE',  ( 765.0180583372156207, -432.9982390220555999, -360.0135310231089534 ) ) ;
#44377 = CARTESIAN_POINT ( 'NONE',  ( 804.4286716492782716, -89.36187538569299704, -345.3141322388244703 ) ) ;
#44378 = CARTESIAN_POINT ( 'NONE',  ( 803.2186876482843445, -295.9874144716866908, 350.0220218866286928 ) ) ;
#44379 = DIRECTION ( 'NONE',  ( 0.000000000000000000, -0.000000000000000000, -1.000000000000000000 ) ) ;
#44380 = CARTESIAN_POINT ( 'NONE',  ( -78.83651009197140525, 260.0000000000000568, -202.7499999999934346 ) ) ;
#44381 = CARTESIAN_POINT ( 'NONE',  ( 789.9999999999992042, 240.0000000000000568, -319.9999999999999432 ) ) ;
#44382 = ORIENTED_EDGE ( 'NONE', *, *, #402, .T. ) ;
#44383 = CARTESIAN_POINT ( 'NONE',  ( 807.2620300519052989, -336.0090635724251911, -318.0141637701419768 ) ) ;
#44384 = CARTESIAN_POINT ( 'NONE',  ( 809.0717654672305343, -196.9181544815164386, 360.1688906516309885 ) ) ;
#44385 = CARTESIAN_POINT ( 'NONE',  ( 788.8264449731200330, -285.1800572038740711, -363.6646147819171233 ) ) ;
#44386 = LINE ( 'NONE', #9295, #9716 ) ;
#44387 = CARTESIAN_POINT ( 'NONE',  ( 804.1105419155481968, -171.8272453906074304, -347.6308680596136469 ) ) ;
#44388 = EDGE_CURVE ( 'NONE', #8835, #2741, #9860, .T. ) ;
#44389 = CARTESIAN_POINT ( 'NONE',  ( 759.0252816721024374, -48.99823902205675807, 368.0189434323527280 ) ) ;
#44390 = VECTOR ( 'NONE', #4980, 1000.000000000000000 ) ;
#44391 = PLANE ( 'NONE',  #43180 ) ;
#44392 = CARTESIAN_POINT ( 'NONE',  ( 810.7187646348534145, -378.4527844766011526, -356.7737145352016341 ) ) ;
#44393 = PLANE ( 'NONE',  #18784 ) ;
#44394 = CARTESIAN_POINT ( 'NONE',  ( 797.8594530101008786, -37.54369356751132614, 322.1405469898980982 ) ) ;
#44395 = CARTESIAN_POINT ( 'NONE',  ( 781.2370466360911223, -332.7363362996979390, 304.9990715423533629 ) ) ;
#44396 = CARTESIAN_POINT ( 'NONE',  ( 792.3570229623688874, -261.1800572038741848, 373.1304606946836202 ) ) ;
#44397 = CARTESIAN_POINT ( 'NONE',  ( 747.2067596250078623, -3.180057203875080063, -352.2312462859687230 ) ) ;
#44398 = EDGE_CURVE ( 'NONE', #41015, #37952, #37861, .T. ) ;
#44399 = CARTESIAN_POINT ( 'NONE',  ( 800.0135310231082713, -254.0891481129652334, -325.0180583372163028 ) ) ;
#44400 = DIRECTION ( 'NONE',  ( -0.000000000000000000, -0.000000000000000000, 1.000000000000000000 ) ) ;
#44401 = CARTESIAN_POINT ( 'NONE',  ( 803.6646147819161570, -353.9073299311467053, 348.8264449731210561 ) ) ;
#44402 = CARTESIAN_POINT ( 'NONE',  ( 804.8461984189677878, -122.1908817542439749, 336.9566956441385628 ) ) ;
#44403 = CARTESIAN_POINT ( 'NONE',  ( 766.7756240680305382, -38.53286901714206891, -361.5560724626415663 ) ) ;
#44404 = CARTESIAN_POINT ( 'NONE',  ( 756.1443688327750579, -45.62377810805114109, 314.3581564841659315 ) ) ;
#44405 = CARTESIAN_POINT ( 'NONE',  ( 781.8018195045267476, -382.2709662947829088, 365.1927285166407273 ) ) ;
#44406 = CARTESIAN_POINT ( 'NONE',  ( 879.9999999999992042, 239.9999999999998863, -219.9999999999999716 ) ) ;
#44407 = DIRECTION ( 'NONE',  ( -1.000000000000000000, -0.000000000000000000, -0.000000000000000000 ) ) ;
#44408 = CARTESIAN_POINT ( 'NONE',  ( 791.9812246680005501, -404.6346026584193396, 361.9419747391813189 ) ) ;
#44409 = ORIENTED_EDGE ( 'NONE', *, *, #14757, .T. ) ;
#44410 = CARTESIAN_POINT ( 'NONE',  ( 798.7617431975189675, -315.6237781080503169, -323.0428371773161871 ) ) ;
#44412 = CARTESIAN_POINT ( 'NONE',  ( 792.1044303154646968, -204.4527844766016926, 317.8323909638837677 ) ) ;
#44411 = CARTESIAN_POINT ( 'NONE',  ( 757.8323909638827445, -194.6346026584198796, 352.1044303154654358 ) ) ;
#44413 = AXIS2_PLACEMENT_3D ( 'NONE', #18503, #3499, #21491 ) ;
#44414 = CARTESIAN_POINT ( 'NONE',  ( 744.9990715423526808, -354.3510508353228943, -341.2370466360926002 ) ) ;
#44415 = DIRECTION ( 'NONE',  ( -0.000000000000000000, 1.000000000000000000, -0.000000000000000000 ) ) ;
#44416 = EDGE_CURVE ( 'NONE', #21150, #17206, #31101, .T. ) ;
#44417 = ORIENTED_EDGE ( 'NONE', *, *, #16680, .T. ) ;
#44418 = CARTESIAN_POINT ( 'NONE',  ( 794.9819416627830151, -372.9982390220557704, 319.9864689768909898 ) ) ;
#44419 = EDGE_CURVE ( 'NONE', #33515, #31020, #43038, .T. ) ;
#44420 = ORIENTED_EDGE ( 'NONE', *, *, #29254, .T. ) ;
#44421 = CARTESIAN_POINT ( 'NONE',  ( 751.6929314249748586, -222.9982390220561399, -318.8095938919659034 ) ) ;
#44422 = CARTESIAN_POINT ( 'NONE',  ( 758.8095938919644823, -128.0891481129655745, 311.6929314249762797 ) ) ;
#44423 = ORIENTED_EDGE ( 'NONE', *, *, #24119, .F. ) ;
#44424 = CARTESIAN_POINT ( 'NONE',  ( 795.1360043628808398, -164.0891481129654892, -360.2193346964456282 ) ) ;
#44425 = ORIENTED_EDGE ( 'NONE', *, *, #32862, .F. ) ;
#44426 = CARTESIAN_POINT ( 'NONE',  ( 800.2193346964447755, -330.9982390220558273, -355.1360043628815788 ) ) ;
#44427 = CARTESIAN_POINT ( 'NONE',  ( 787.5531968255692163, -453.8272453906066630, -316.1348686366205811 ) ) ;
#44428 = CARTESIAN_POINT ( 'NONE',  ( 755.2512626584698410, -247.5436935675106724, 315.2512626584710915 ) ) ;
#44429 = CARTESIAN_POINT ( 'NONE',  ( 758.6633372737375112, -188.5328690171416497, 326.9102291470432533 ) ) ;
#44431 = DIRECTION ( 'NONE',  ( 1.000000000000000000, -0.000000000000000000, -0.000000000000000000 ) ) ;
#44430 = CARTESIAN_POINT ( 'NONE',  ( -468.8365100919714337, 260.0000000000001705, -199.9999999999908766 ) ) ;
#44432 = CYLINDRICAL_SURFACE ( 'NONE', #30214, 6.118999999999985562 ) ;
#44433 = ORIENTED_EDGE ( 'NONE', *, *, #15984, .T. ) ;
#44434 = CARTESIAN_POINT ( 'NONE',  ( 779.4763451958990572, -416.7363362996975980, -365.0264073115438919 ) ) ;
#44435 = DIRECTION ( 'NONE',  ( -0.000000000000000000, 1.000000000000000000, -1.110223024625155554E-15 ) ) ;
#44436 = CARTESIAN_POINT ( 'NONE',  ( 919.9999999999993179, 154.9999999999998863, -360.0000000000000000 ) ) ;
#44437 = EDGE_LOOP ( 'NONE', ( #16538, #43529, #45333, #6063 ) ) ;
#44438 = CARTESIAN_POINT ( 'NONE',  ( 773.7305795820266212, -249.2817908451526421, -374.8230680027170365 ) ) ;
#44439 = CARTESIAN_POINT ( 'NONE',  ( 744.6391490659812007, -110.7363362996985501, 338.7502325331110455 ) ) ;
#44441 = CARTESIAN_POINT ( 'NONE',  ( 755.0636971347428243, -196.2709662947835909, -341.7834795799807353 ) ) ;
#44440 = LINE ( 'NONE', #12129, #23387 ) ;
#44442 = EDGE_CURVE ( 'NONE', #44330, #21264, #43073, .T. ) ;
#44443 = CARTESIAN_POINT ( 'NONE',  ( 795.9930595647434757, -363.0783235625955854, -320.7433823573372820 ) ) ;
#44444 = DIRECTION ( 'NONE',  ( 0.000000000000000000, 0.000000000000000000, 1.000000000000000000 ) ) ;
#44445 = CARTESIAN_POINT ( 'NONE',  ( 771.3260364891663130, -235.6454272087890729, -306.0683387631859773 ) ) ;
#44446 = DIRECTION ( 'NONE',  ( 0.000000000000000000, 0.000000000000000000, -1.000000000000000000 ) ) ;
#44447 = DIRECTION ( 'NONE',  ( 8.659560562354807133E-17, 0.7071067811865578978, -0.7071067811865372477 ) ) ;
#44448 = CARTESIAN_POINT ( 'NONE',  ( 763.8424801807145741, -90.00906357242590161, -320.5453621957614700 ) ) ;
#44449 = CARTESIAN_POINT ( 'NONE',  ( 757.0176451133909268, -421.0999726633340288, 349.9200121543848354 ) ) ;
#44450 = EDGE_CURVE ( 'NONE', #13136, #23168, #22413, .T. ) ;
#44451 = CONICAL_SURFACE ( 'NONE', #34090, 8.024999999999948841, 0.7853981633974337351 ) ;
#44452 = DIRECTION ( 'NONE',  ( -1.000000000000000000, 0.000000000000000000, -0.000000000000000000 ) ) ;
#44453 = CARTESIAN_POINT ( 'NONE',  ( 784.0799538623451781, -419.8055962898681059, -364.6971507214555572 ) ) ;
#44454 = CARTESIAN_POINT ( 'NONE',  ( 796.9462024416508257, -276.4527844766014368, -308.9653473494370246 ) ) ;
#44455 = LINE ( 'NONE', #37759, #11466 ) ;
#44456 = DIRECTION ( 'NONE',  ( -1.000000000000000000, -0.000000000000000000, -0.000000000000000000 ) ) ;
#44457 = CARTESIAN_POINT ( 'NONE',  ( 778.1981804954714335, -34.27096629478407408, -314.8072714833589885 ) ) ;
#44458 = CARTESIAN_POINT ( 'NONE',  ( 749.5768839229115201, -204.5545181178800931, 358.0661480581553064 ) ) ;
#44459 = CARTESIAN_POINT ( 'NONE',  ( 744.8212110874229666, -162.8965053807780521, -336.2046728542121627 ) ) ;
#44460 = CARTESIAN_POINT ( 'NONE',  ( 759.0252816721024374, -168.9982390220563673, 368.0189434323527280 ) ) ;
#44461 = CARTESIAN_POINT ( 'NONE',  ( 744.7301800767019131, -412.8164208402372992, -337.4774526936615757 ) ) ;
#44462 = EDGE_CURVE ( 'NONE', #9555, #44320, #41510, .T. ) ;
#44463 = FACE_OUTER_BOUND ( 'NONE', #2621, .T. ) ;
#44464 = CARTESIAN_POINT ( 'NONE',  ( 781.8018195045266339, -262.2709662947831930, 365.1927285166406705 ) ) ;
#44465 =( GEOMETRIC_REPRESENTATION_CONTEXT ( 3 ) GLOBAL_UNCERTAINTY_ASSIGNED_CONTEXT ( ( #1022 ) ) GLOBAL_UNIT_ASSIGNED_CONTEXT ( ( #11175, #4013, #4259 ) ) REPRESENTATION_CONTEXT ( 'NONE', 'WORKASPACE' ) );
#44466 = CARTESIAN_POINT ( 'NONE',  ( 790.9844846989617508, -46.37269993606239638, 317.2208543904092721 ) ) ;
#44467 = CARTESIAN_POINT ( 'NONE',  ( 794.9819416627830151, -396.9982390220556567, -319.9864689768909898 ) ) ;
#44468 = DIRECTION ( 'NONE',  ( 0.000000000000000000, 0.000000000000000000, 1.000000000000000000 ) ) ;
#44469 = CARTESIAN_POINT ( 'NONE',  ( -338.8365100919713200, 240.0000000000001421, -197.2499999999919282 ) ) ;
#44470 = CARTESIAN_POINT ( 'NONE',  ( 803.8651313633788504, -101.2601417444146250, 332.4468031744301015 ) ) ;
#44471 = ORIENTED_EDGE ( 'NONE', *, *, #43665, .F. ) ;
#44472 = CARTESIAN_POINT ( 'NONE',  ( 796.7845633553578182, -225.6237781080506011, -358.5707757039688204 ) ) ;
#44473 = CARTESIAN_POINT ( 'NONE',  ( 765.0180583372156207, -120.9982390220565378, -360.0135310231089534 ) ) ;
#44474 = CARTESIAN_POINT ( 'NONE',  ( 795.1360043628807261, -68.08914811296575920, 360.2193346964456282 ) ) ;
#44475 = CARTESIAN_POINT ( 'NONE',  ( 773.7943932421234194, -263.8055962898686175, -305.5313806188329409 ) ) ;
#44476 = SURFACE_SIDE_STYLE ('',( #22988 ) ) ;
#44477 = CARTESIAN_POINT ( 'NONE',  ( 814.8230680027162407, -365.8055962898682765, 333.7305795820267917 ) ) ;
#44478 = VERTEX_POINT ( 'NONE', #2937 ) ;
#44479 = CARTESIAN_POINT ( 'NONE',  ( 792.3570229623688874, 2.819942796124898177, 373.1304606946836202 ) ) ;
#44480 = EDGE_CURVE ( 'NONE', #2099, #1769, #17495, .T. ) ;
#44481 = CARTESIAN_POINT ( 'NONE',  ( 800.2193346964447755, -186.9982390220563104, -355.1360043628815788 ) ) ;
#44482 = CARTESIAN_POINT ( 'NONE',  ( 765.0180583372156207, -384.9982390220556567, 360.0135310231089534 ) ) ;
#44483 = CARTESIAN_POINT ( 'NONE',  ( 782.5225473063381969, -94.27096629478386092, -375.2698199232970637 ) ) ;
#44484 = AXIS2_PLACEMENT_3D ( 'NONE', #2875, #16276, #30355 ) ;
#44485 = CARTESIAN_POINT ( 'NONE',  ( 794.9819416627830151, -84.99823902205663728, -319.9864689768909898 ) ) ;
#44486 = VERTEX_POINT ( 'NONE', #31334 ) ;
#44487 = CARTESIAN_POINT ( 'NONE',  ( 802.9823548866075953, -25.09997266333519050, -330.0799878456151077 ) ) ;
#44488 = VERTEX_POINT ( 'NONE', #10098 ) ;
#44489 = CARTESIAN_POINT ( 'NONE',  ( 804.6971507214547046, -363.2817908451523294, -344.0799538623459739 ) ) ;
#44491 = CARTESIAN_POINT ( 'NONE',  ( 755.8894580844503253, -399.8272453906067767, 332.3691319403863531 ) ) ;
#44490 = CARTESIAN_POINT ( 'NONE',  ( 754.8072714833581358, -100.8164208402383792, 338.1981804954720587 ) ) ;
#44492 = CARTESIAN_POINT ( 'NONE',  ( 798.7617431975189675, -99.62377810805098477, 323.0428371773161871 ) ) ;
#44495 = CARTESIAN_POINT ( 'NONE',  ( 749.8865473780648472, -356.5328690171410813, 322.1177392798429082 ) ) ;
#44494 = CARTESIAN_POINT ( 'NONE',  ( 789.5584187865343893, -452.9681489794450613, -363.1011989789364520 ) ) ;
#44493 = CARTESIAN_POINT ( 'NONE',  ( 749.2812353651451076, -438.4527844766009821, 323.2262854647983090 ) ) ;
#44496 = CARTESIAN_POINT ( 'NONE',  ( 796.1575198192839480, -318.0090635724251911, -359.4546378042384163 ) ) ;
#44497 = CARTESIAN_POINT ( 'NONE',  ( 791.0478386215596629, -117.8272453906076151, -306.7653713866226326 ) ) ;
#44498 = CARTESIAN_POINT ( 'NONE',  ( 786.2694204179717872, 2.718209154846545683, 305.1769319972829067 ) ) ;
#44499 = ADVANCED_FACE ( 'NONE', ( #17024 ), #38495, .F. ) ;
#44500 =( GEOMETRIC_REPRESENTATION_CONTEXT ( 3 ) GLOBAL_UNCERTAINTY_ASSIGNED_CONTEXT ( ( #17326 ) ) GLOBAL_UNIT_ASSIGNED_CONTEXT ( ( #40357, #5437, #33629 ) ) REPRESENTATION_CONTEXT ( 'NONE', 'WORKASPACE' ) );
#44502 = LINE ( 'NONE', #37347, #7894 ) ;
#44501 = CARTESIAN_POINT ( 'NONE',  ( 311.1634899080286232, 260.0000000000000000, -199.9999999999963336 ) ) ;
#44503 = ADVANCED_FACE ( 'NONE', ( #21176 ), #6628, .F. ) ;
#44504 = CARTESIAN_POINT ( 'NONE',  ( 803.8651313633788504, -269.2601417444139997, -332.4468031744301015 ) ) ;
#44505 = CARTESIAN_POINT ( 'NONE',  ( 747.6481478633932056, -109.0999726633349241, -353.4146539503763620 ) ) ;
#44506 = DIRECTION ( 'NONE',  ( 0.000000000000000000, 0.000000000000000000, 1.000000000000000000 ) ) ;
#44507 = LINE ( 'NONE', #26949, #31163 ) ;
#44508 = CARTESIAN_POINT ( 'NONE',  ( 779.4763451958990572, -344.7363362996978253, 365.0264073115438919 ) ) ;
#44509 = EDGE_CURVE ( 'NONE', #12675, #4037, #26071, .T. ) ;
#44510 = CARTESIAN_POINT ( 'NONE',  ( 764.8639956371174549, -176.0891481129653755, 319.7806653035542013 ) ) ;
#44511 = ORIENTED_EDGE ( 'NONE', *, *, #15390, .T. ) ;
#44512 = CARTESIAN_POINT ( 'NONE',  ( 788.6739635108323228, -295.6454272087888739, 373.9316612368139090 ) ) ;
#44513 = CARTESIAN_POINT ( 'NONE',  ( 804.7487373415286811, -163.5436935675109567, -364.7487373415288516 ) ) ;
#44514 = FACE_OUTER_BOUND ( 'NONE', #10932, .T. ) ;
#44515 = CARTESIAN_POINT ( 'NONE',  ( 747.6481478633932056, -109.0999726633349241, 353.4146539503763620 ) ) ;
#44516 = CARTESIAN_POINT ( 'NONE',  ( 744.7301800767019131, -292.8164208402376971, -337.4774526936615757 ) ) ;
#44517 = DIRECTION ( 'NONE',  ( -0.000000000000000000, 1.000000000000000000, -0.000000000000000000 ) ) ;
#44518 = PRODUCT_DEFINITION ( 'UNKNOWN', '', #12056, #20563 ) ;
#44519 = CARTESIAN_POINT ( 'NONE',  ( 804.4286716492782716, -137.3618753856928265, 345.3141322388244703 ) ) ;
#44520 = VECTOR ( 'NONE', #19569, 1000.000000000000000 ) ;
#44521 = ORIENTED_EDGE ( 'NONE', *, *, #31077, .F. ) ;
#44522 = CARTESIAN_POINT ( 'NONE',  ( 799.9636004259356241, -406.9181544815157849, 311.2241431872006956 ) ) ;
#44523 = CARTESIAN_POINT ( 'NONE',  ( 766.5853460496234675, -325.9874144716865771, -372.3518521366060554 ) ) ;
#44524 = VECTOR ( 'NONE', #29571, 1000.000000000000000 ) ;
#44525 = CARTESIAN_POINT ( 'NONE',  ( 751.6929314249748586, -102.9982390220565520, -318.8095938919659034 ) ) ;
#44526 = CARTESIAN_POINT ( 'NONE',  ( 800.9840315886518738, -52.91815448151692891, 354.1144889064786412 ) ) ;
#44527 = CARTESIAN_POINT ( 'NONE',  ( 759.0252816721024374, -384.9982390220556567, -368.0189434323527280 ) ) ;
#44528 = FACE_OUTER_BOUND ( 'NONE', #30853, .T. ) ;
#44529 = CARTESIAN_POINT ( 'NONE',  ( 790.8726784830453198, -442.7146871989589840, 362.5472867521010585 ) ) ;
#44530 = ORIENTED_EDGE ( 'NONE', *, *, #11726, .F. ) ;
#44531 = CARTESIAN_POINT ( 'NONE',  ( 803.2186876482843445, -79.98741447168740137, 350.0220218866286928 ) ) ;
#44532 = CARTESIAN_POINT ( 'NONE',  ( 783.7566961878529810, -168.8965053807780237, -305.1792804349288417 ) ) ;
#44533 = CARTESIAN_POINT ( 'NONE',  ( 51.16348990802859475, 256.5000000000000568, -199.9999999999945146 ) ) ;
#44534 = CARTESIAN_POINT ( 'NONE',  ( 758.0141637701419768, -279.0783235625958127, 367.2620300519063790 ) ) ;
#44535 = CARTESIAN_POINT ( 'NONE',  ( 765.0180583372156207, -72.99823902205667991, 360.0135310231089534 ) ) ;
#44536 = ORIENTED_EDGE ( 'NONE', *, *, #21274, .T. ) ;
#44537 = VECTOR ( 'NONE', #14656, 1000.000000000000000 ) ;
#44538 = CARTESIAN_POINT ( 'NONE',  ( 754.8983024940795303, 5.103494619221427442, -336.9254006560228163 ) ) ;
#44539 = CARTESIAN_POINT ( 'NONE',  ( 756.5762568750052424, -267.1800572038742985, 348.7366044899774238 ) ) ;
#44540 = CARTESIAN_POINT ( 'NONE',  ( 778.7502325331095108, -432.3510508353226669, -304.6391490659818828 ) ) ;
#44541 = LINE ( 'NONE', #33033, #6213 ) ;
#44542 = VERTEX_POINT ( 'NONE', #42190 ) ;
#44543 = ORIENTED_EDGE ( 'NONE', *, *, #4374, .F. ) ;
#44544 = CARTESIAN_POINT ( 'NONE',  ( 814.4686193811664907, -387.2817908451522726, -346.2056067578752732 ) ) ;
#44545 = CARTESIAN_POINT ( 'NONE',  ( 759.9864689768902508, -242.0891481129652618, -354.9819416627836404 ) ) ;
#44547 = CARTESIAN_POINT ( 'NONE',  ( 776.2433038121456548, -204.8965053807779100, 374.8207195650711014 ) ) ;
#44546 = CARTESIAN_POINT ( 'NONE',  ( 746.8695393053151292, -317.9073299311467622, 327.6429770376306578 ) ) ;
#44548 = CARTESIAN_POINT ( 'NONE',  ( 755.3028492785439312, -231.2817908451527558, -335.9200461376539693 ) ) ;
#44549 = CARTESIAN_POINT ( 'NONE',  ( 800.2193346964447755, -234.9982390220561683, -355.1360043628815788 ) ) ;
#44550 = VECTOR ( 'NONE', #44231, 1000.000000000000000 ) ;
#44551 = CARTESIAN_POINT ( 'NONE',  ( 785.3687786644885591, -419.3618753856918602, -315.3201227861280813 ) ) ;
#44552 = AXIS2_PLACEMENT_3D ( 'NONE', #13966, #7033, #37993 ) ;
#44553 = ORIENTED_EDGE ( 'NONE', *, *, #29187, .T. ) ;
#44554 = CARTESIAN_POINT ( 'NONE',  ( 754.8072714833581358, -220.8164208402379529, 338.1981804954720587 ) ) ;
#44555 = CARTESIAN_POINT ( 'NONE',  ( 755.0636971347428243, -100.2709662947838609, -341.7834795799807353 ) ) ;
#44556 = ORIENTED_EDGE ( 'NONE', *, *, #37672, .T. ) ;
#44557 = CARTESIAN_POINT ( 'NONE',  ( 767.6429770376289525, -345.1800572038739006, 306.8695393053162093 ) ) ;
#44558 = CARTESIAN_POINT ( 'NONE',  ( 999.9999999999992042, 249.9999999999998863, -360.0000000000000000 ) ) ;
#44559 = CARTESIAN_POINT ( 'NONE',  ( 763.3756531158825283, 16.45630643248848912, 321.2690078247891847 ) ) ;
#44560 = DIRECTION ( 'NONE',  ( 0.000000000000000000, 1.000000000000000000, 0.000000000000000000 ) ) ;
#44561 = CARTESIAN_POINT ( 'NONE',  ( 790.9844846989617508, -214.3726999360618493, 317.2208543904092721 ) ) ;
#44562 = CARTESIAN_POINT ( 'NONE',  ( 771.2633955100217236, -95.90732993114751537, 363.4237431249939618 ) ) ;
#44563 = ORIENTED_EDGE ( 'NONE', *, *, #36243, .F. ) ;
#44564 = CARTESIAN_POINT ( 'NONE',  ( 797.8822607201568644, -438.5545181178793541, -370.1134526219340160 ) ) ;
#44565 = CARTESIAN_POINT ( 'NONE',  ( 796.7737145352015204, -68.63460265842033436, -370.7187646348536987 ) ) ;
#44566 = CARTESIAN_POINT ( 'NONE',  ( 794.1144889064781864, -274.1692326535049915, 360.9840315886528401 ) ) ;
#44567 = CARTESIAN_POINT ( 'NONE',  ( 797.8594530101008786, -421.5436935675101040, -322.1405469898980982 ) ) ;
#44568 = CARTESIAN_POINT ( 'NONE',  ( 785.3141322388236176, -45.72551174932949181, -364.4286716492789537 ) ) ;
#44569 = AXIS2_PLACEMENT_3D ( 'NONE', #36017, #35781, #32328 ) ;
#44570 = CARTESIAN_POINT ( 'NONE',  ( 744.6391490659812007, -14.73633629969885384, 338.7502325331110455 ) ) ;
#44571 = CARTESIAN_POINT ( 'NONE',  ( -786.4999999999993179, -110.5936016518799221, 750.6326042729449455 ) ) ;
#44572 = CARTESIAN_POINT ( 'NONE',  ( 800.9840315886518738, -292.9181544815162397, -354.1144889064786412 ) ) ;
#44573 = CARTESIAN_POINT ( 'NONE',  ( 772.5602148656447525, -201.7255117493290015, -305.7998596910095443 ) ) ;
#44574 = VECTOR ( 'NONE', #27366, 1000.000000000000000 ) ;
#44575 = CARTESIAN_POINT ( 'NONE',  ( 758.8095938919642549, -80.08914811296574499, 311.6929314249763365 ) ) ;
#44576 = CARTESIAN_POINT ( 'NONE',  ( 767.6429770376289525, -129.1800572038746111, 306.8695393053162093 ) ) ;
#44577 = LINE ( 'NONE', #37639, #29171 ) ;
#44578 = CARTESIAN_POINT ( 'NONE',  ( 701.1634899080286232, 239.9999999999999147, -197.2499999999991758 ) ) ;
#44579 = CARTESIAN_POINT ( 'NONE',  ( 746.7653713866222915, -233.2601417444141987, -351.0478386215610271 ) ) ;
#44580 = CARTESIAN_POINT ( 'NONE',  ( 812.3518521366052028, -409.0999726633340288, 326.5853460496235243 ) ) ;
#44581 = CARTESIAN_POINT ( 'NONE',  ( 746.8695393053150156, -293.9073299311468759, -327.6429770376306010 ) ) ;
#44582 = DIRECTION ( 'NONE',  ( 0.000000000000000000, 1.000000000000000000, 3.700743415417198493E-16 ) ) ;
#44583 = CARTESIAN_POINT ( 'NONE',  ( 792.3570229623688874, -405.1800572038737300, 373.1304606946836202 ) ) ;
#44584 = CARTESIAN_POINT ( 'NONE',  ( 814.9108240113580450, -16.27096629478413092, 337.5031285880265273 ) ) ;
#44585 = CARTESIAN_POINT ( 'NONE',  ( 805.1927285166397041, -352.8164208402374129, -341.8018195045277707 ) ) ;
#44586 = AXIS2_PLACEMENT_3D ( 'NONE', #1334, #16731, #29516 ) ;
#44587 = CARTESIAN_POINT ( 'NONE',  ( 755.0488828828309806, -17.80559628986940979, 344.1219089521771934 ) ) ;
#44588 = CIRCLE ( 'NONE', #9177, 10.00000000000000888 ) ;
#44589 = CARTESIAN_POINT ( 'NONE',  ( 776.2046728542105711, -92.19088175424406018, -304.8212110874238761 ) ) ;
#44590 = CARTESIAN_POINT ( 'NONE',  ( 786.6156483768007774, -169.4419599262325562, -315.5913626894246136 ) ) ;
#44591 = CARTESIAN_POINT ( 'NONE',  ( 781.2497674668890113, -156.3510508353235480, 375.3608509340180603 ) ) ;
#44592 = CARTESIAN_POINT ( 'NONE',  ( 792.1044303154646968, 11.54721552339759860, 317.8323909638837677 ) ) ;
#44593 = EDGE_LOOP ( 'NONE', ( #29425, #21551, #44788, #24995, #7261, #14204, #35970, #5223, #28479, #21696, #9451, #10756, #30927, #16765, #13414, #43907, #42000, #43600 ) ) ;
#44594 = CARTESIAN_POINT ( 'NONE',  ( 759.7806653035534055, -54.99823902205672255, -324.8639956371180801 ) ) ;
#44595 = CARTESIAN_POINT ( 'NONE',  ( 801.3366627262608972, -152.5328690171416781, -353.0897708529566899 ) ) ;
#44596 = CARTESIAN_POINT ( 'NONE',  ( 785.3141322388236176, -165.7255117493291152, 364.4286716492789537 ) ) ;
#44597 = CARTESIAN_POINT ( 'NONE',  ( 754.0944755984390895, 8.376221891948691933, -364.1009440267246760 ) ) ;
#44598 = CARTESIAN_POINT ( 'NONE',  ( 801.9419747391806368, -306.4527844766013800, 351.9812246680014027 ) ) ;
#44599 = DIRECTION ( 'NONE',  ( -1.000000000000000000, -0.000000000000000000, -0.000000000000000000 ) ) ;
#44600 = EDGE_LOOP ( 'NONE', ( #30674, #36004, #4663, #43631 ) ) ;
#44601 = CARTESIAN_POINT ( 'NONE',  ( 801.3366627262608972, -8.532869017142163059, 353.0897708529566899 ) ) ;
#44602 = CARTESIAN_POINT ( 'NONE',  ( 757.7880784355613741, -282.0090635724253048, -312.4576283171834916 ) ) ;
#44603 = AXIS2_PLACEMENT_3D ( 'NONE', #33677, #26732, #13128 ) ;
#44604 = ORIENTED_EDGE ( 'NONE', *, *, #29307, .T. ) ;
#44605 = DIRECTION ( 'NONE',  ( -1.000000000000000000, 0.000000000000000000, 0.000000000000000000 ) ) ;
#44606 = CARTESIAN_POINT ( 'NONE',  ( 763.2262854647970016, -224.6346026584198228, 309.2812353651462445 ) ) ;
#44607 = CARTESIAN_POINT ( 'NONE',  ( 793.9708237608222134, -286.9181544815161828, 319.2295555964448681 ) ) ;
#44608 = CARTESIAN_POINT ( 'NONE',  ( 793.2243759319678702, -434.5328690171407970, 318.4439275373583200 ) ) ;
#44609 = VERTEX_POINT ( 'NONE', #4085 ) ;
#44610 = CARTESIAN_POINT ( 'NONE',  ( 772.4468031744293057, -105.8272453906076578, -363.8651313633793620 ) ) ;
#44611 = CARTESIAN_POINT ( 'NONE',  ( 754.8072714833581358, -100.8164208402383792, -338.1981804954720587 ) ) ;
#44612 = CARTESIAN_POINT ( 'NONE',  ( 803.6646147819162707, -329.9073299311467622, -348.8264449731211130 ) ) ;
#44613 = VERTEX_POINT ( 'NONE', #8226 ) ;
#44614 = CARTESIAN_POINT ( 'NONE',  ( 771.1735550268778070, -441.1800572038735027, -316.3353852180827630 ) ) ;
#44615 = CARTESIAN_POINT ( 'NONE',  ( 758.6633372737375112, -308.5328690171412518, 326.9102291470432533 ) ) ;
#44616 = CARTESIAN_POINT ( 'NONE',  ( 799.9999999999993179, -365.3551492539851893, -1.867567485292990437 ) ) ;
#44617 = DIRECTION ( 'NONE',  ( 0.000000000000000000, 0.3826834323650836200, 0.9238795325112892920 ) ) ;
#44618 = CARTESIAN_POINT ( 'NONE',  ( 804.4086373105744769, -121.6454272087894282, 333.3843516231986541 ) ) ;
#44619 = CARTESIAN_POINT ( 'NONE',  ( 1820.038553321469863, -589.9999999999998863, -210.0000000000000000 ) ) ;
#44620 = EDGE_LOOP ( 'NONE', ( #20798, #20023, #13489, #33341 ) ) ;
#44621 = CARTESIAN_POINT ( 'NONE',  ( 744.6391490659812007, -350.7363362996978253, -338.7502325331110455 ) ) ;
#44622 = CARTESIAN_POINT ( 'NONE',  ( 807.2620300519052989, -192.0090635724255606, 318.0141637701419768 ) ) ;
#44623 = CIRCLE ( 'NONE', #35025, 30.00000000000008171 ) ;
#44624 = CARTESIAN_POINT ( 'NONE',  ( 781.8018195045266339, -334.2709662947829656, -365.1927285166406705 ) ) ;
#44625 = CARTESIAN_POINT ( 'NONE',  ( 805.2837595273609850, -170.7363362996983938, -340.5290396650784714 ) ) ;
#44626 = CARTESIAN_POINT ( 'NONE',  ( 800.9747183278959710, -60.99823902205671544, 311.9810565676471583 ) ) ;
#44627 = FACE_BOUND ( 'NONE', #44193, .T. ) ;
#44628 = CARTESIAN_POINT ( 'NONE',  ( 804.7487373415286811, -379.5436935675102745, -364.7487373415288516 ) ) ;
#44629 = DIRECTION ( 'NONE',  ( -1.000000000000000000, -0.000000000000000000, -0.000000000000000000 ) ) ;
#44630 = AXIS2_PLACEMENT_3D ( 'NONE', #41703, #11194, #31965 ) ;
#44631 = CARTESIAN_POINT ( 'NONE',  ( 783.7953271457878373, -320.1908817542434349, 375.1787889125761239 ) ) ;
#44632 = DIRECTION ( 'NONE',  ( 8.659560562354932858E-17, 0.7071067811865474617, -0.7071067811865474617 ) ) ;
#44633 = CARTESIAN_POINT ( 'NONE',  ( 745.4481719005789273, -291.7255117493285752, 347.5162901302853129 ) ) ;
#44634 = CARTESIAN_POINT ( 'NONE',  ( 772.5602148656447525, -9.725511749329603717, -305.7998596910095443 ) ) ;
#44635 = CARTESIAN_POINT ( 'NONE',  ( 788.7366044899766848, -251.9073299311470748, -316.5762568750059813 ) ) ;
#44636 = AXIS2_PLACEMENT_3D ( 'NONE', #12332, #40506, #15780 ) ;
#44637 = DIRECTION ( 'NONE',  ( 1.000000000000000000, 0.000000000000000000, 0.000000000000000000 ) ) ;
#44638 = VECTOR ( 'NONE', #18618, 1000.000000000000000 ) ;
#44639 = EDGE_CURVE ( 'NONE', #39336, #33570, #20934, .T. ) ;
#44640 = CARTESIAN_POINT ( 'NONE',  ( 788.8264449731200330, -357.1800572038739006, 363.6646147819171233 ) ) ;
#44641 = CARTESIAN_POINT ( 'NONE',  ( 793.9708237608222134, -118.9181544815167229, 319.2295555964448681 ) ) ;
#44642 = CARTESIAN_POINT ( 'NONE',  ( 755.8398074228967971, -67.44195992623289726, -333.4516893846970333 ) ) ;
#44643 = CARTESIAN_POINT ( 'NONE',  ( 798.0661480581538854, -50.53286901714203339, 309.5768839229118043 ) ) ;
#44644 = CARTESIAN_POINT ( 'NONE',  ( 755.5713283507202505, -365.3618753856920875, 334.6858677611754729 ) ) ;
#44645 = LINE ( 'NONE', #42090, #2594 ) ;
#44646 = CARTESIAN_POINT ( 'NONE',  ( 757.8323909638827445, -434.6346026584190554, 352.1044303154654358 ) ) ;
#44647 = ORIENTED_EDGE ( 'NONE', *, *, #45466, .F. ) ;
#44648 = CARTESIAN_POINT ( 'NONE',  ( 767.8955696845333705, -72.45278447660213317, -362.1676090361162323 ) ) ;
#44649 = CARTESIAN_POINT ( 'NONE',  ( 775.9200461376533440, -359.8055962898683333, -315.3028492785443291 ) ) ;
#44651 = CARTESIAN_POINT ( 'NONE',  ( 767.8955696845334842, -192.4527844766017211, 362.1676090361161755 ) ) ;
#44650 = CARTESIAN_POINT ( 'NONE',  ( 800.0135310231082713, -182.0891481129654323, 325.0180583372163028 ) ) ;
#44652 = AXIS2_PLACEMENT_3D ( 'NONE', #39709, #35992, #32302 ) ;
#44653 = CARTESIAN_POINT ( 'NONE',  ( 752.4576283171824116, -357.0783235625956422, -317.7880784355627952 ) ) ;
#44654 = DIRECTION ( 'NONE',  ( 0.000000000000000000, 0.000000000000000000, 1.000000000000000000 ) ) ;
#44655 = ORIENTED_EDGE ( 'NONE', *, *, #7791, .T. ) ;
#44656 = CARTESIAN_POINT ( 'NONE',  ( 781.7834795799800531, -394.8164208402374697, 315.0636971347436202 ) ) ;
#44657 = AXIS2_PLACEMENT_3D ( 'NONE', #31086, #45183, #10082 ) ;
#44658 = ORIENTED_EDGE ( 'NONE', *, *, #18752, .T. ) ;
#44659 = CARTESIAN_POINT ( 'NONE',  ( 805.0032342141412300, -205.5436935675108430, -314.9967657858571783 ) ) ;
#44660 = CARTESIAN_POINT ( 'NONE',  ( 792.2312462859673587, -107.9073299311474727, 307.2067596250082602 ) ) ;
#44661 = ORIENTED_EDGE ( 'NONE', *, *, #21559, .T. ) ;
#44662 = CARTESIAN_POINT ( 'NONE',  ( 785.3687786644885591, -203.3618753856926276, -315.3201227861280813 ) ) ;
#44663 = ORIENTED_EDGE ( 'NONE', *, *, #17866, .T. ) ;
#44664 = CARTESIAN_POINT ( 'NONE',  ( 755.3201227861273992, -339.7255117493285184, -345.3687786644892981 ) ) ;
#44665 = CARTESIAN_POINT ( 'NONE',  ( 802.5472867521000353, -460.3726999360611103, -350.8726784830461156 ) ) ;
#44666 = PRESENTATION_LAYER_ASSIGNMENT (  '', '', ( #5588 ) ) ;
#44667 = CARTESIAN_POINT ( 'NONE',  ( 796.9462024416508257, -252.4527844766015789, 308.9653473494370246 ) ) ;
#44668 = CARTESIAN_POINT ( 'NONE',  ( 804.9511171171677688, -197.8055962898688733, 335.8780910478229202 ) ) ;
#44670 = DIRECTION ( 'NONE',  ( -0.000000000000000000, -1.110223024625155554E-15, 1.000000000000000000 ) ) ;
#44669 = CARTESIAN_POINT ( 'NONE',  ( 792.0613484971601110, -458.0032201311295807, 367.4685979341032294 ) ) ;
#44671 = ADVANCED_FACE ( 'NONE', ( #15165 ), #39884, .F. ) ;
#44672 = CARTESIAN_POINT ( 'NONE',  ( 571.1634899080285095, 239.9999999999999432, -199.9999999999981526 ) ) ;
#44673 = VECTOR ( 'NONE', #35004, 1000.000000000000114 ) ;
#44674 = PRODUCT_DEFINITION_SHAPE ( 'NONE', 'NONE',  #42550 ) ;
#44675 = ORIENTED_EDGE ( 'NONE', *, *, #13697, .F. ) ;
#44676 = CARTESIAN_POINT ( 'NONE',  ( 773.4516893846965786, -451.6454272087884192, -315.8398074228977066 ) ) ;
#44677 = LINE ( 'NONE', #5638, #12214 ) ;
#44678 = LINE ( 'NONE', #37514, #41072 ) ;
#44679 = EDGE_LOOP ( 'NONE', ( #39695, #29272, #3873, #11440 ) ) ;
#44680 = CARTESIAN_POINT ( 'NONE',  ( 783.7953271457878373, -224.1908817542436623, -375.1787889125761239 ) ) ;
#44681 = CARTESIAN_POINT ( 'NONE',  ( 752.7379699480933368, -108.0090635724258448, 361.9858362298580232 ) ) ;
#44683 = CARTESIAN_POINT ( 'NONE',  ( 794.9819416627830151, -180.9982390220563389, -319.9864689768909898 ) ) ;
#44682 = FACE_OUTER_BOUND ( 'NONE', #21890, .T. ) ;
#44684 = CARTESIAN_POINT ( 'NONE',  ( 776.9566956441375396, -372.8965053807773415, -364.8461984189686405 ) ) ;
#44685 = CARTESIAN_POINT ( 'NONE',  ( 814.8207195650702488, -242.1908817542435770, -336.2433038121456548 ) ) ;
#44686 = CARTESIAN_POINT ( 'NONE',  ( 787.4999999999992042, -512.9681489794448908, -339.9999999999999432 ) ) ;
#44687 = LINE ( 'NONE', #16741, #7606 ) ;
#44688 = CARTESIAN_POINT ( 'NONE',  ( 759.0159684113467620, -88.91815448151682233, -325.8855110935213020 ) ) ;
#44689 = CARTESIAN_POINT ( 'NONE',  ( 758.4439275373578084, -420.5545181178793541, 353.2243759319684386 ) ) ;
#44690 = CARTESIAN_POINT ( 'NONE',  ( -598.8365100919716042, 260.0000000000001705, -193.8809999999899674 ) ) ;
#44691 = AXIS2_PLACEMENT_3D ( 'NONE', #30343, #30814, #31034 ) ;
#44692 = CARTESIAN_POINT ( 'NONE',  ( 795.9930595647434757, -435.0783235625953580, -320.7433823573372820 ) ) ;
#44693 = CARTESIAN_POINT ( 'NONE',  ( 759.0252816721024374, -264.9982390220561115, -368.0189434323527280 ) ) ;
#44694 = LINE ( 'NONE', #34053, #15864 ) ;
#44695 = CARTESIAN_POINT ( 'NONE',  ( 764.8639956371174549, 15.91085188703394238, 319.7806653035542013 ) ) ;
#44696 = CARTESIAN_POINT ( 'NONE',  ( 802.1676090361156639, -38.63460265842041252, -327.8955696845344505 ) ) ;
#44697 = CARTESIAN_POINT ( 'NONE',  ( 755.8990559732751535, -203.4636090269709996, 365.9055244015606831 ) ) ;
#44698 = CARTESIAN_POINT ( 'NONE',  ( 744.9990715423526808, -162.3510508353235196, -341.2370466360926002 ) ) ;
#44699 = CARTESIAN_POINT ( 'NONE',  ( 767.6429770376289525, -177.1800572038744690, 306.8695393053162093 ) ) ;
#44700 = CARTESIAN_POINT ( 'NONE',  ( 758.8095938919642549, -392.0891481129648355, -311.6929314249763365 ) ) ;
#44701 = CONICAL_SURFACE ( 'NONE', #1914, 8.024999999999948841, 0.7853981633963380560 ) ;
#44702 = LINE ( 'NONE', #3107, #14346 ) ;
#44703 = CARTESIAN_POINT ( 'NONE',  ( 795.1360043628807261, -260.0891481129650060, 360.2193346964456282 ) ) ;
#44704 = CARTESIAN_POINT ( 'NONE',  ( 773.4516893846965786, -67.64542720878958448, 315.8398074228977066 ) ) ;
#44705 = CARTESIAN_POINT ( 'NONE',  ( 804.9363028652555840, -424.2709662947829088, -338.2165204200192079 ) ) ;
#44706 = VECTOR ( 'NONE', #33448, 1000.000000000000000 ) ;
#44707 = CARTESIAN_POINT ( 'NONE',  ( 799.9999999999993179, -365.3551492539851893, -18.13243251470705886 ) ) ;
#44708 = PLANE ( 'NONE',  #11484 ) ;
#44710 = CARTESIAN_POINT ( 'NONE',  ( 759.7806653035534055, -318.9982390220557704, 324.8639956371180801 ) ) ;
#44709 = CARTESIAN_POINT ( 'NONE',  ( 770.0799878456142551, -85.98741447168738716, 362.9823548866085616 ) ) ;
#44711 = ORIENTED_EDGE ( 'NONE', *, *, #6377, .T. ) ;
#44712 = AXIS2_PLACEMENT_3D ( 'NONE', #28662, #34500, #24721 ) ;
#44713 = CARTESIAN_POINT ( 'NONE',  ( 757.2208543904082489, -256.7146871989595525, -350.9844846989624330 ) ) ;
#44714 = CARTESIAN_POINT ( 'NONE',  ( 801.9419747391806368, -42.45278447660223264, 351.9812246680014027 ) ) ;
#44715 = CARTESIAN_POINT ( 'NONE',  ( 788.7631598425961101, -265.4419599262323004, -305.7194118038759143 ) ) ;
#44716 = CARTESIAN_POINT ( 'NONE',  ( 767.9999999999992042, 205.0000000000000568, 339.9999999999999432 ) ) ;
#44717 = CARTESIAN_POINT ( 'NONE',  ( 764.3348316497523456, -382.7146871989591546, 308.6759233522265617 ) ) ;
#44718 = ORIENTED_EDGE ( 'NONE', *, *, #6964, .F. ) ;
#44719 = CARTESIAN_POINT ( 'NONE',  ( 797.6776695296629214, -283.5436935675105019, 357.6776695296636603 ) ) ;
#44720 = CARTESIAN_POINT ( 'NONE',  ( 763.2262854647970016, 15.36539734157940629, 309.2812353651462445 ) ) ;
#44721 = CARTESIAN_POINT ( 'NONE',  ( 774.6858677611749044, -177.7255117493290868, -315.5713283507209894 ) ) ;
#44722 = CARTESIAN_POINT ( 'NONE',  ( 756.3353852180819104, -389.9073299311465348, 331.1735550268788302 ) ) ;
#44723 = ADVANCED_FACE ( 'NONE', ( #8013 ), #32947, .F. ) ;
#44724 = CARTESIAN_POINT ( 'NONE',  ( 804.7487373415286811, -115.5436935675110988, -364.7487373415288516 ) ) ;
#44725 = CARTESIAN_POINT ( 'NONE',  ( 788.7366044899766848, -107.9073299311474727, -316.5762568750059813 ) ) ;
#44726 = ORIENTED_EDGE ( 'NONE', *, *, #8298, .F. ) ;
#44727 = CARTESIAN_POINT ( 'NONE',  ( 754.7162404726377645, -38.73633629969877035, -339.4709603349214717 ) ) ;
#44728 = CIRCLE ( 'NONE', #24061, 10.00000000000000888 ) ;
#44729 = CARTESIAN_POINT ( 'NONE',  ( 798.5707757039680246, -365.4636090269705164, -356.7845633553585003 ) ) ;
#44731 = CARTESIAN_POINT ( 'NONE',  ( 798.5707757039680246, -389.4636090269704027, 356.7845633553585003 ) ) ;
#44730 = CARTESIAN_POINT ( 'NONE',  ( 759.9864689768902508, -98.08914811296568814, 354.9819416627836404 ) ) ;
#44732 = CARTESIAN_POINT ( 'NONE',  ( 800.7704444035546203, -100.1692326535055315, 326.0291762391768771 ) ) ;
#44733 = ADVANCED_FACE ( 'NONE', ( #18857 ), #11470, .T. ) ;
#44734 = AXIS2_PLACEMENT_3D ( 'NONE', #6779, #13492, #27346 ) ;
#44737 = CARTESIAN_POINT ( 'NONE',  ( 815.0009284576459549, -342.3510508353228943, 338.7629533639073429 ) ) ;
#44736 = CARTESIAN_POINT ( 'NONE',  ( 989.9999999999992042, -416.7569064942979935, 212.5753187112032947 ) ) ;
#44735 = CARTESIAN_POINT ( 'NONE',  ( 808.3070685750232087, -450.9982390220554294, 361.1904061080339829 ) ) ;
#44738 = ADVANCED_FACE ( 'NONE', ( #32485 ), #36391, .T. ) ;
#44739 = CARTESIAN_POINT ( 'NONE',  ( 746.7653713866222915, -113.2601417444145682, 351.0478386215610271 ) ) ;
#44740 = CARTESIAN_POINT ( 'NONE',  ( 799.2566176426618085, -360.0090635724250774, -324.0069404352559559 ) ) ;
#44741 = CARTESIAN_POINT ( 'NONE',  ( 778.2165204200184689, -334.8164208402376403, -364.9363028652563230 ) ) ;
#44742 = CARTESIAN_POINT ( 'NONE',  ( 791.0478386215596629, -141.8272453906075157, -306.7653713866226326 ) ) ;
#44743 = CARTESIAN_POINT ( 'NONE',  ( 813.5763878283155464, -3.827245390607979303, 351.1614460488615350 ) ) ;
#44745 = DIRECTION ( 'NONE',  ( -1.000000000000000000, -0.000000000000000000, -0.000000000000000000 ) ) ;
#44744 = DIRECTION ( 'NONE',  ( -0.000000000000000000, 1.000000000000000000, -0.000000000000000000 ) ) ;
#44746 = CARTESIAN_POINT ( 'NONE',  ( 780.5290396650775619, -252.3510508353232353, -365.2837595273619513 ) ) ;
#44747 = CARTESIAN_POINT ( 'NONE',  ( 814.2805881961230625, -121.6454272087894282, -331.2368401574024119 ) ) ;
#44748 = DIRECTION ( 'NONE',  ( -0.000000000000000000, 1.000000000000000000, -0.000000000000000000 ) ) ;
#44749 = CARTESIAN_POINT ( 'NONE',  ( -26.63011601220122060, -494.6608068873671300, -357.6536686473015720 ) ) ;
#44750 = AXIS2_PLACEMENT_3D ( 'NONE', #38095, #31144, #16850 ) ;
#44751 = CARTESIAN_POINT ( 'NONE',  ( 776.9254006560222479, -332.1908817542433781, 314.8983024940802125 ) ) ;
#44752 = VERTEX_POINT ( 'NONE', #36172 ) ;
#44753 = CARTESIAN_POINT ( 'NONE',  ( 793.5525998758768083, -295.0999726633343698, 372.6845335610516941 ) ) ;
#44754 = CARTESIAN_POINT ( 'NONE',  ( 811.0346526505617248, -158.6346026584200217, -323.0537975583478101 ) ) ;
#44755 = EDGE_CURVE ( 'NONE', #34810, #10697, #18405, .T. ) ;
#44756 = DIRECTION ( 'NONE',  ( 0.000000000000000000, 0.000000000000000000, -1.000000000000000000 ) ) ;
#44757 = CARTESIAN_POINT ( 'NONE',  ( 786.2694204179717872, -93.28179084515315367, 305.1769319972829067 ) ) ;
#44758 = EDGE_CURVE ( 'NONE', #36817, #6928, #4532, .T. ) ;
#44759 = CARTESIAN_POINT ( 'NONE',  ( 746.8695393053150156, -293.9073299311468759, -327.6429770376306010 ) ) ;
#44760 = CARTESIAN_POINT ( 'NONE',  ( 799.9999999999993179, 205.0000000000000568, -350.0000000000000000 ) ) ;
#44761 = DIRECTION ( 'NONE',  ( 1.000000000000000000, 0.000000000000000000, 0.000000000000000000 ) ) ;
#44762 = CARTESIAN_POINT ( 'NONE',  ( 794.9819416627830151, -132.9982390220564810, 319.9864689768909898 ) ) ;
#44763 = ORIENTED_EDGE ( 'NONE', *, *, #23454, .F. ) ;
#44764 = CARTESIAN_POINT ( 'NONE',  ( 814.4686193811664907, -411.2817908451521589, 346.2056067578752732 ) ) ;
#44765 = CARTESIAN_POINT ( 'NONE',  ( 798.0661480581538854, -386.5328690171409676, -309.5768839229118043 ) ) ;
#44766 = CARTESIAN_POINT ( 'NONE',  ( 777.5031285880264704, -118.8164208402383508, -374.9108240113588408 ) ) ;
#44767 = CARTESIAN_POINT ( 'NONE',  ( 758.4439275373578084, -36.55451811788061178, 353.2243759319684386 ) ) ;
#44768 = CARTESIAN_POINT ( 'NONE',  ( 814.5518280994195948, -375.7255117493283478, -332.4837098697145734 ) ) ;
#44769 = DIRECTION ( 'NONE',  ( 0.000000000000000000, -1.000000000000000000, 0.000000000000000000 ) ) ;
#44770 = CARTESIAN_POINT ( 'NONE',  ( 756.7813123517142913, -427.9874144716862929, 329.9779781133712504 ) ) ;
#44771 = VERTEX_POINT ( 'NONE', #29017 ) ;
#44772 = VECTOR ( 'NONE', #39477, 1000.000000000000000 ) ;
#44773 = VECTOR ( 'NONE', #12633, 1000.000000000000000 ) ;
#44774 = CARTESIAN_POINT ( 'NONE',  ( 808.7758568127978833, -172.1692326535052757, -320.0363995740631822 ) ) ;
#44775 = PLANE ( 'NONE',  #34374 ) ;
#44776 = CARTESIAN_POINT ( 'NONE',  ( 808.7758568127978833, -292.1692326535048210, 320.0363995740631822 ) ) ;
#44777 = CARTESIAN_POINT ( 'NONE',  ( 800.2193346964446619, -90.99823902205662307, 355.1360043628816925 ) ) ;
#44778 = ORIENTED_EDGE ( 'NONE', *, *, #15389, .F. ) ;
#44779 = AXIS2_PLACEMENT_3D ( 'NONE', #25017, #8163, #25705 ) ;
#44780 = ADVANCED_FACE ( 'NONE', ( #17943 ), #31984, .F. ) ;
#44781 = CARTESIAN_POINT ( 'NONE',  ( 756.1348686366196716, -17.26014174441486659, -347.5531968255698416 ) ) ;
#44782 = CARTESIAN_POINT ( 'NONE',  ( 768.0187753319979720, -272.6346026584196807, 318.0580252608186242 ) ) ;
#44783 = CIRCLE ( 'NONE', #43291, 2.749999999999919176 ) ;
#44784 = ADVANCED_FACE ( 'NONE', ( #384 ), #10784, .T. ) ;
#44785 = CARTESIAN_POINT ( 'NONE',  ( 751.6929314249748586, -6.998239022056885972, -318.8095938919659034 ) ) ;
#44786 = DIRECTION ( 'NONE',  ( -1.000000000000000000, -0.000000000000000000, -0.000000000000000000 ) ) ;
#44787 = ORIENTED_EDGE ( 'NONE', *, *, #1300, .T. ) ;
#44788 = ORIENTED_EDGE ( 'NONE', *, *, #43347, .T. ) ;
#44789 = CARTESIAN_POINT ( 'NONE',  ( 781.2370466360911223, -428.7363362996975980, -304.9990715423533629 ) ) ;
#44791 = CARTESIAN_POINT ( 'NONE',  ( 783.7566961878529810, -264.8965053807776826, 305.1792804349288417 ) ) ;
#44790 = CARTESIAN_POINT ( 'NONE',  ( 782.4968714119720516, -322.8164208402377540, 305.0891759886411023 ) ) ;
#44792 = CARTESIAN_POINT ( 'NONE',  ( 801.5560724626406000, -216.5545181178800931, -326.7756240680316182 ) ) ;
#44793 = CARTESIAN_POINT ( 'NONE',  ( 771.1735550268778070, -201.1800572038744690, -316.3353852180827630 ) ) ;
#44794 = CARTESIAN_POINT ( 'NONE',  ( 792.1044303154646968, -420.4527844766009821, -317.8323909638837677 ) ) ;
#44795 = CARTESIAN_POINT ( 'NONE',  ( 800.2193346964447755, -234.9982390220561683, 355.1360043628815788 ) ) ;
#44796 = EDGE_LOOP ( 'NONE', ( #17169, #44563, #7597, #36271, #21784, #40113, #8361 ) ) ;
#44797 = CARTESIAN_POINT ( 'NONE',  ( 808.3070685750230950, -354.9982390220557704, 361.1904061080339261 ) ) ;
#44798 = DIRECTION ( 'NONE',  ( -0.000000000000000000, -1.000000000000000000, 0.000000000000000000 ) ) ;
#44799 = CARTESIAN_POINT ( 'NONE',  ( 748.6759233522253680, -16.37269993606248519, -324.3348316497537098 ) ) ;
#44800 = LINE ( 'NONE', #33928, #19660 ) ;
#44801 = DIRECTION ( 'NONE',  ( 1.000000000000000000, 0.000000000000000000, 0.000000000000000000 ) ) ;
#44802 = CARTESIAN_POINT ( 'NONE',  ( 763.8424801807145741, -210.0090635724255321, 320.5453621957614700 ) ) ;
#44803 = CARTESIAN_POINT ( 'NONE',  ( 755.5713283507202505, -77.36187538569302546, 334.6858677611754729 ) ) ;
#44804 = ORIENTED_EDGE ( 'NONE', *, *, #41610, .F. ) ;
#44805 = CARTESIAN_POINT ( 'NONE',  ( 783.7953271457878373, -440.1908817542430370, -375.1787889125761239 ) ) ;
#44806 = CARTESIAN_POINT ( 'NONE',  ( 749.2812353651451076, -54.45278447660219001, -323.2262854647983090 ) ) ;
#44807 = CARTESIAN_POINT ( 'NONE',  ( 803.8651313633788504, -245.2601417444141987, 332.4468031744301015 ) ) ;
#44808 = CARTESIAN_POINT ( 'NONE',  ( 755.3201227861273992, -435.7255117493282341, -345.3687786644892981 ) ) ;
#44809 = CARTESIAN_POINT ( 'NONE',  ( 781.8018195045267476, -46.27096629478403855, -365.1927285166407273 ) ) ;
#44810 = CARTESIAN_POINT ( 'NONE',  ( 795.8262568251477660, -22.37269993606246743, 308.3538107759623585 ) ) ;
#44811 = DIRECTION ( 'NONE',  ( -0.000000000000000000, 1.000000000000000000, -0.000000000000000000 ) ) ;
#44812 = CARTESIAN_POINT ( 'NONE',  ( 772.4468031744293057, -297.8272453906070041, -363.8651313633793620 ) ) ;
#44813 = CARTESIAN_POINT ( 'NONE',  ( 796.7737145352015204, -212.6346026584198796, -370.7187646348536987 ) ) ;
#44814 = CARTESIAN_POINT ( 'NONE',  ( 814.5518280994195948, -87.72551174932937101, 332.4837098697145734 ) ) ;
#44815 = CARTESIAN_POINT ( 'NONE',  ( 759.0252816721024374, -144.9982390220564525, 368.0189434323527280 ) ) ;
#44816 = DIRECTION ( 'NONE',  ( -0.000000000000000000, -6.938893903907222461E-16, 1.000000000000000000 ) ) ;
#44817 = CYLINDRICAL_SURFACE ( 'NONE', #40925, 10.00000000000000888 ) ;
#44818 = CARTESIAN_POINT ( 'NONE',  ( 813.9316612368132837, -247.4419599262323004, -348.6739635108323228 ) ) ;
#44819 = CARTESIAN_POINT ( 'NONE',  ( 760.0363995740630116, -418.9181544815157849, 368.7758568127991907 ) ) ;
#44820 = CARTESIAN_POINT ( 'NONE',  ( 758.8095938919642549, -272.0891481129651197, -311.6929314249763365 ) ) ;
#44821 = DIRECTION ( 'NONE',  ( 0.000000000000000000, 0.000000000000000000, -1.000000000000000000 ) ) ;
#44822 = CARTESIAN_POINT ( 'NONE',  ( 759.0252816721024374, -408.9982390220556567, 368.0189434323527280 ) ) ;
#44823 = CARTESIAN_POINT ( 'NONE',  ( 759.0252816721024374, -24.99823902205683268, 368.0189434323527280 ) ) ;
#44824 = CARTESIAN_POINT ( 'NONE',  ( 759.9864689768902508, -362.0891481129648923, -354.9819416627836404 ) ) ;
#44825 = CARTESIAN_POINT ( 'NONE',  ( 754.8983024940795303, -18.89650538077849617, 336.9254006560228163 ) ) ;
#44826 = CARTESIAN_POINT ( 'NONE',  ( 754.0944755984390895, -63.62377810805107714, -364.1009440267246760 ) ) ;
#44827 = CARTESIAN_POINT ( 'NONE',  ( 757.2208543904082489, -160.7146871989598651, -350.9844846989624330 ) ) ;
#44828 = CARTESIAN_POINT ( 'NONE',  ( 798.0661480581538854, -170.5328690171416781, 309.5768839229118043 ) ) ;
#44829 = CARTESIAN_POINT ( 'NONE',  ( 800.2193346964446619, 5.001760977943074948, 355.1360043628816925 ) ) ;
#44830 = ORIENTED_EDGE ( 'NONE', *, *, #44887, .T. ) ;
#44831 = CARTESIAN_POINT ( 'NONE',  ( 771.1735550268778070, -57.18005720387489532, -316.3353852180827630 ) ) ;
#44832 = CARTESIAN_POINT ( 'NONE',  ( 799.4546378042377910, -177.0783235625961538, -356.1575198192848006 ) ) ;
#44833 = CARTESIAN_POINT ( 'NONE',  ( 755.5713283507202505, -149.3618753856928265, 334.6858677611754729 ) ) ;
#44834 = CARTESIAN_POINT ( 'NONE',  ( 815.1787889125755555, 17.10349461922139369, -343.7953271457877804 ) ) ;
#44835 = CARTESIAN_POINT ( 'NONE',  ( 757.8323909638828582, -290.6346026584196238, 352.1044303154654358 ) ) ;
#44836 = DIRECTION ( 'NONE',  ( -0.000000000000000000, 1.000000000000000000, -0.000000000000000000 ) ) ;
#44837 = ORIENTED_EDGE ( 'NONE', *, *, #5410, .F. ) ;
#44838 = CARTESIAN_POINT ( 'NONE',  ( 805.1016975059191054, -6.896505380778533478, 343.0745993439771837 ) ) ;
#44839 = CARTESIAN_POINT ( 'NONE',  ( 762.1177392798416577, -282.5545181178798657, -309.8865473780659272 ) ) ;
#44840 = CIRCLE ( 'NONE', #26395, 2.749999999999919176 ) ;
#44841 = APPLICATION_PROTOCOL_DEFINITION ( 'draft international standard', 'automotive_design', 1998, #43487 ) ;
#44842 = CARTESIAN_POINT ( 'NONE',  ( 759.0252816721024374, -216.9982390220562252, 368.0189434323527280 ) ) ;
#44843 = CARTESIAN_POINT ( 'NONE',  ( 757.4527132478984868, -352.3726999360614514, 329.1273215169538844 ) ) ;
#44844 = CARTESIAN_POINT ( 'NONE',  ( 786.6156483768007774, -433.4419599262316183, 315.5913626894246136 ) ) ;
#44845 = VERTEX_POINT ( 'NONE', #7327 ) ;
#44846 = CARTESIAN_POINT ( 'NONE',  ( 796.1575198192839480, -102.0090635724258448, -359.4546378042384163 ) ) ;
#44847 = CARTESIAN_POINT ( 'NONE',  ( 756.3353852180819104, -101.9073299311474727, -331.1735550268788302 ) ) ;
#44848 = CARTESIAN_POINT ( 'NONE',  ( 797.6776695296629214, -331.5436935675104451, -357.6776695296636603 ) ) ;
#44849 = VERTEX_POINT ( 'NONE', #21403 ) ;
#44850 = CARTESIAN_POINT ( 'NONE',  ( 774.6858677611749044, -441.7255117493282910, -315.5713283507209894 ) ) ;
#44851 = CARTESIAN_POINT ( 'NONE',  ( 795.9930595647434757, -291.0783235625957559, 320.7433823573372820 ) ) ;
#44852 = DIRECTION ( 'NONE',  ( 0.000000000000000000, 0.7517448203044204691, -0.6594541114781790059 ) ) ;
#44853 = LINE ( 'NONE', #19906, #24114 ) ;
#44854 = CARTESIAN_POINT ( 'NONE',  ( 775.8780910478218402, -129.2817908451530400, 364.9511171171680530 ) ) ;
#44855 = LINE ( 'NONE', #5822, #6418 ) ;
#44856 = ORIENTED_EDGE ( 'NONE', *, *, #28934, .F. ) ;
#44857 = CARTESIAN_POINT ( 'NONE',  ( 746.4236121716829757, -351.8272453906068336, -328.8385539511384650 ) ) ;
#44858 = CARTESIAN_POINT ( 'NONE',  ( 788.6739635108323228, -199.6454272087891582, 373.9316612368139090 ) ) ;
#44859 = CARTESIAN_POINT ( 'NONE',  ( 781.7834795799800531, -322.8164208402377540, -315.0636971347436202 ) ) ;
#44860 = LINE ( 'NONE', #9741, #39246 ) ;
#44861 = CARTESIAN_POINT ( 'NONE',  ( 804.6971507214547046, -195.2817908451528410, -344.0799538623459739 ) ) ;
#44862 = CARTESIAN_POINT ( 'NONE',  ( 763.0537975583475827, -48.45278447660219712, 371.0346526505627480 ) ) ;
#44863 = DIRECTION ( 'NONE',  ( -0.000000000000000000, -0.000000000000000000, 1.000000000000000000 ) ) ;
#44864 = CARTESIAN_POINT ( 'NONE',  ( 777.4774526936600978, -370.2709662947830793, -304.7301800767028226 ) ) ;
#44865 = CARTESIAN_POINT ( 'NONE',  ( -773.4999999999993179, -365.3551492539851893, -8.132432514707076621 ) ) ;
#44866 = VECTOR ( 'NONE', #38057, 1000.000000000000000 ) ;
#44867 = CARTESIAN_POINT ( 'NONE',  ( 814.4686193811664907, -315.2817908451525000, 346.2056067578752732 ) ) ;
#44868 = CARTESIAN_POINT ( 'NONE',  ( -26.63011601220122060, -365.3551492539851893, -18.13243251470705886 ) ) ;
#44869 = CARTESIAN_POINT ( 'NONE',  ( 745.0891759886404770, -292.2709662947831930, 342.4968714119734159 ) ) ;
#44870 = CARTESIAN_POINT ( 'NONE',  ( 792.2312462859673587, -11.90732993114778182, -307.2067596250082602 ) ) ;
#44871 = CARTESIAN_POINT ( 'NONE',  ( 754.8072714833581358, -244.8164208402378961, -338.1981804954720587 ) ) ;
#44872 = CARTESIAN_POINT ( 'NONE',  ( -39.63011601220123481, -110.5936016518799221, 750.6326042729449455 ) ) ;
#44873 = CARTESIAN_POINT ( 'NONE',  ( 788.8264449731200330, -381.1800572038737869, 363.6646147819171233 ) ) ;
#44874 = CARTESIAN_POINT ( 'NONE',  ( 804.1105419155481968, -171.8272453906074304, 347.6308680596136469 ) ) ;
#44875 = CARTESIAN_POINT ( 'NONE',  ( 765.8855110935204493, -46.16923265350568784, -319.0159684113471599 ) ) ;
#44876 = CARTESIAN_POINT ( 'NONE',  ( 812.6845335610512393, -55.98741447168748664, 353.5525998758768651 ) ) ;
#44877 = CARTESIAN_POINT ( 'NONE',  ( 804.6798772138710092, -375.7255117493284047, 334.6312213355106451 ) ) ;
#44878 = DIRECTION ( 'NONE',  ( 0.000000000000000000, -1.000000000000000000, 0.000000000000000000 ) ) ;
#44879 = LINE ( 'NONE', #16462, #9293 ) ;
#44880 = CARTESIAN_POINT ( 'NONE',  ( 746.7653713866222915, -137.2601417444144829, 351.0478386215610271 ) ) ;
#44881 = CARTESIAN_POINT ( 'NONE',  ( 759.9864689768902508, -434.0891481129646081, 354.9819416627836404 ) ) ;
#44882 = ORIENTED_EDGE ( 'NONE', *, *, #43518, .T. ) ;
#44883 = CARTESIAN_POINT ( 'NONE',  ( 762.1405469898971887, -73.54369356751118403, -357.8594530101015607 ) ) ;
#44884 = CARTESIAN_POINT ( 'NONE',  ( 773.3843516231979720, -373.4419599262319593, -364.4086373105754433 ) ) ;
#44886 = CARTESIAN_POINT ( 'NONE',  ( 804.9363028652555840, -208.2709662947835341, 338.2165204200192079 ) ) ;
#44885 = CARTESIAN_POINT ( 'NONE',  ( 785.3687786644884454, -203.3618753856925991, 315.3201227861279676 ) ) ;
#44887 = EDGE_CURVE ( 'NONE', #31705, #16263, #14486, .T. ) ;
#44888 = CARTESIAN_POINT ( 'NONE',  ( 814.8230680027162407, -365.8055962898682765, -333.7305795820267917 ) ) ;
#44889 = LINE ( 'NONE', #38411, #17515 ) ;
#44890 = VERTEX_POINT ( 'NONE', #4314 ) ;
#44891 = CARTESIAN_POINT ( 'NONE',  ( 771.1735550268778070, -393.1800572038737300, 316.3353852180827630 ) ) ;
#44892 = VERTEX_POINT ( 'NONE', #1058 ) ;
#44893 = SHAPE_REPRESENTATION_RELATIONSHIP ( 'NONE' , 'NONE' ,  #4721, #39222 ) ;
#44894 = CARTESIAN_POINT ( 'NONE',  ( 767.6429770376289525, -225.1800572038743269, -306.8695393053162093 ) ) ;
#44895 = CARTESIAN_POINT ( 'NONE',  ( 805.0032342141413437, -109.5436935675110988, 314.9967657858572352 ) ) ;
#44896 = VERTEX_POINT ( 'NONE', #11700 ) ;
#44897 = CARTESIAN_POINT ( 'NONE',  ( 804.9363028652555840, -208.2709662947835341, -338.2165204200192079 ) ) ;
#44898 = EDGE_LOOP ( 'NONE', ( #4952, #28807, #34672, #23442 ) ) ;
#44899 = CIRCLE ( 'NONE', #32381, 9.999999999999982236 ) ;
#44900 = CARTESIAN_POINT ( 'NONE',  ( 755.0636971347428243, -316.2709662947832499, -341.7834795799807353 ) ) ;
#44901 = CARTESIAN_POINT ( 'NONE',  ( 768.0187753319979720, 15.36539734157940629, -318.0580252608186242 ) ) ;
#44902 = CARTESIAN_POINT ( 'NONE',  ( 755.8398074228967971, -187.4419599262325278, 333.4516893846970333 ) ) ;
#44904 = CARTESIAN_POINT ( 'NONE',  ( 794.9999999999993179, 205.0000000000000568, -255.0000000000000000 ) ) ;
#44903 = CARTESIAN_POINT ( 'NONE',  ( 181.9156952255813735, 290.0000000000001137, -274.9999999999999432 ) ) ;
#44905 = CARTESIAN_POINT ( 'NONE',  ( 799.9999999999993179, -512.9681489794448908, -350.0000000000000000 ) ) ;
#44906 = ORIENTED_EDGE ( 'NONE', *, *, #6658, .F. ) ;
#44907 = CARTESIAN_POINT ( 'NONE',  ( 763.8424801807145741, -450.0090635724248500, -320.5453621957614700 ) ) ;
#44908 = CARTESIAN_POINT ( 'NONE',  ( 919.9999999999993179, 154.9999999999998863, 360.0000000000000000 ) ) ;
#44909 = CARTESIAN_POINT ( 'NONE',  ( 787.4999999999992042, -462.9681489794448339, 369.0473750965555837 ) ) ;
#44910 = EDGE_LOOP ( 'NONE', ( #43575, #36945 ) ) ;
#44911 = CARTESIAN_POINT ( 'NONE',  ( 749.5768839229115201, -252.5545181178799226, -358.0661480581553064 ) ) ;
#44912 = CARTESIAN_POINT ( 'NONE',  ( 811.3240766477731540, -100.3726999360622187, 355.6651683502462902 ) ) ;
#44914 = CARTESIAN_POINT ( 'NONE',  ( 756.5762568750052424, -219.1800572038744122, -348.7366044899774238 ) ) ;
#44913 = CARTESIAN_POINT ( 'NONE',  ( 879.9999999999992042, 239.9999999999998295, -350.0000000000000000 ) ) ;
#44915 = CARTESIAN_POINT ( 'NONE',  ( 761.2382568024794409, -351.6237781080502032, -356.9571628226838129 ) ) ;
#44916 = CARTESIAN_POINT ( 'NONE',  ( 778.7629533639073998, -248.7363362996981380, -375.0009284576466371 ) ) ;
#44917 = LINE ( 'NONE', #31042, #36327 ) ;
#44918 = CARTESIAN_POINT ( 'NONE',  ( -879.9999999999992042, 240.0000000000002274, -179.9999999999999716 ) ) ;
#44919 = CARTESIAN_POINT ( 'NONE',  ( 769.9779781133707957, -91.09997266333496668, -316.7813123517150871 ) ) ;
#44920 = CARTESIAN_POINT ( 'NONE',  ( 800.9840315886518738, -436.9181544815157281, 354.1144889064786412 ) ) ;
#44921 = CARTESIAN_POINT ( 'NONE',  ( 999.5857864376259840, 479.9999999999999432, 360.0000000000000000 ) ) ;
#44922 = CARTESIAN_POINT ( 'NONE',  ( 761.2382568024794409, -423.6237781080499190, -356.9571628226838129 ) ) ;
#44923 = CARTESIAN_POINT ( 'NONE',  ( 796.7737145352015204, -260.6346026584197375, -370.7187646348536987 ) ) ;
#44924 = DIRECTION ( 'NONE',  ( 0.000000000000000000, -0.6594541114781790059, -0.7517448203044204691 ) ) ;
#44925 = DIRECTION ( 'NONE',  ( 0.000000000000000000, 0.000000000000000000, -1.000000000000000000 ) ) ;
#44926 = CARTESIAN_POINT ( 'NONE',  ( 800.0135310231082713, -38.08914811296587999, -325.0180583372163028 ) ) ;
#44927 = CARTESIAN_POINT ( 'NONE',  ( 768.9521613784389729, -225.8272453906072599, 373.2346286133773106 ) ) ;
#44928 = CARTESIAN_POINT ( 'NONE',  ( 795.6651683502461765, -178.7146871989598083, -371.3240766477733814 ) ) ;
#44929 = CARTESIAN_POINT ( 'NONE',  ( 777.4774526936600978, -178.2709662947835625, 304.7301800767027657 ) ) ;
#44930 = CARTESIAN_POINT ( 'NONE',  ( 772.4837098697144029, -407.3618753856920307, -374.5518280994205611 ) ) ;
#44931 = DIRECTION ( 'NONE',  ( -1.000000000000000000, 0.000000000000000000, 0.000000000000000000 ) ) ;
#44932 = CARTESIAN_POINT ( 'NONE',  ( 774.6312213355099630, -287.3618753856923718, 364.6798772138717482 ) ) ;
#44933 = CARTESIAN_POINT ( 'NONE',  ( 772.4468031744293057, -57.82724539060780700, 363.8651313633793620 ) ) ;
#44934 = EDGE_CURVE ( 'NONE', #45022, #42263, #616, .T. ) ;
#44935 = CARTESIAN_POINT ( 'NONE',  ( 803.6646147819161570, -425.9073299311463074, -348.8264449731210561 ) ) ;
#44936 = AXIS2_PLACEMENT_3D ( 'NONE', #41350, #37180, #40886 ) ;
#44937 = DIRECTION ( 'NONE',  ( -1.000000000000000000, -0.000000000000000000, -0.000000000000000000 ) ) ;
#44938 = DIRECTION ( 'NONE',  ( 0.000000000000000000, 0.000000000000000000, 1.000000000000000000 ) ) ;
#44940 = CARTESIAN_POINT ( 'NONE',  ( 755.3201227861273992, -315.7255117493286320, 345.3687786644892981 ) ) ;
#44939 = CARTESIAN_POINT ( 'NONE',  ( 790.8726784830453198, -82.71468719896012090, 362.5472867521010585 ) ) ;
#44941 = ORIENTED_EDGE ( 'NONE', *, *, #43879, .T. ) ;
#44942 = ADVANCED_FACE ( 'NONE', ( #39198 ), #7548, .F. ) ;
#44943 = CARTESIAN_POINT ( 'NONE',  ( 780.5290396650775619, -276.3510508353231785, -365.2837595273619513 ) ) ;
#44944 = CARTESIAN_POINT ( 'NONE',  ( 762.3223304703356007, -127.5436935675110561, -322.3223304703362828 ) ) ;
#44945 = CARTESIAN_POINT ( 'NONE',  ( 802.1676090361156639, -62.63460265842031305, 327.8955696845344505 ) ) ;
#44946 = CARTESIAN_POINT ( 'NONE',  ( 815.0009284576459549, -270.3510508353231216, -338.7629533639073429 ) ) ;
#44947 = DIRECTION ( 'NONE',  ( 0.000000000000000000, 0.000000000000000000, 1.000000000000000000 ) ) ;
#44948 = CARTESIAN_POINT ( 'NONE',  ( 807.5423716828161105, -393.0783235625954717, 362.2119215644372048 ) ) ;
#44949 = ORIENTED_EDGE ( 'NONE', *, *, #7247, .F. ) ;
#44950 = CARTESIAN_POINT ( 'NONE',  ( 804.6798772138708955, -279.7255117493288026, 334.6312213355107019 ) ) ;
#44951 = CARTESIAN_POINT ( 'NONE',  ( 796.9462024416508257, 11.54721552339760038, 308.9653473494370246 ) ) ;
#44952 = CARTESIAN_POINT ( 'NONE',  ( 755.3201227861273992, -171.7255117493291152, -345.3687786644892981 ) ) ;
#44953 = CARTESIAN_POINT ( 'NONE',  ( 794.9819416627830151, -372.9982390220557704, 319.9864689768909898 ) ) ;
#44954 = CARTESIAN_POINT ( 'NONE',  ( 763.0537975583475827, -120.4527844766019484, -371.0346526505627480 ) ) ;
#44955 = CARTESIAN_POINT ( 'NONE',  ( 788.8264449731201466, -117.1800572038747106, -363.6646147819170665 ) ) ;
#44956 = VERTEX_POINT ( 'NONE', #42871 ) ;
#44957 = CARTESIAN_POINT ( 'NONE',  ( 758.4439275373578084, -36.55451811788061178, -353.2243759319684386 ) ) ;
#44958 = CARTESIAN_POINT ( 'NONE',  ( 758.4439275373578084, -348.5545181178796383, -353.2243759319684386 ) ) ;
#44960 = CARTESIAN_POINT ( 'NONE',  ( 787.5531968255692163, -405.8272453906067199, 316.1348686366205811 ) ) ;
#44959 = CARTESIAN_POINT ( 'NONE',  ( 774.6858677611749044, -105.7255117493293000, 315.5713283507209894 ) ) ;
#44961 = CARTESIAN_POINT ( 'NONE',  ( 759.2295555964440155, -88.16923265350555994, 353.9708237608231229 ) ) ;
#44964 = CARTESIAN_POINT ( 'NONE',  ( 811.6461892240364477, -364.7146871989592114, 324.1737431748509835 ) ) ;
#44963 = FACE_OUTER_BOUND ( 'NONE', #25122, .T. ) ;
#44962 = LINE ( 'NONE', #7074, #35840 ) ;
#44965 = ADVANCED_FACE ( 'NONE', ( #11238 ), #14934, .F. ) ;
#44966 = CARTESIAN_POINT ( 'NONE',  ( 754.7162404726377645, -374.7363362996978253, -339.4709603349214717 ) ) ;
#44967 = CARTESIAN_POINT ( 'NONE',  ( 781.7834795799800531, -370.8164208402375834, -315.0636971347436202 ) ) ;
#44968 = CARTESIAN_POINT ( 'NONE',  ( 811.3240766477731540, -124.3726999360621619, -355.6651683502462902 ) ) ;
#44969 = AXIS2_PLACEMENT_3D ( 'NONE', #24089, #35185, #27121 ) ;
#44970 = CARTESIAN_POINT ( 'NONE',  ( 807.2620300519052989, -0.009063572426172561425, 318.0141637701419768 ) ) ;
#44972 = DIRECTION ( 'NONE',  ( -0.000000000000000000, 1.000000000000000000, -0.000000000000000000 ) ) ;
#44971 = CARTESIAN_POINT ( 'NONE',  ( -858.8365100919713768, 256.5000000000002274, -199.9999999999881481 ) ) ;
#44973 = CARTESIAN_POINT ( 'NONE',  ( 773.3843516231979720, -253.4419599262323572, -364.4086373105754433 ) ) ;
#44974 = CARTESIAN_POINT ( 'NONE',  ( 749.5768839229115201, -156.5545181178802636, -358.0661480581553064 ) ) ;
#44975 = LINE ( 'NONE', #36895, #13843 ) ;
#44976 = CARTESIAN_POINT ( 'NONE',  ( 187.1337867209877857, -184.9457194955397199, -62.92409052808242365 ) ) ;
#44977 = CARTESIAN_POINT ( 'NONE',  ( 786.5483106153019435, -343.6454272087887603, 364.1601925771022366 ) ) ;
#44978 = ORIENTED_EDGE ( 'NONE', *, *, #15141, .T. ) ;
#44979 = CARTESIAN_POINT ( 'NONE',  ( 815.3608509340175488, -314.7363362996979959, 341.2497674668889545 ) ) ;
#44980 = CARTESIAN_POINT ( 'NONE',  ( 767.7687537140311633, -167.9073299311473022, -372.7932403749916830 ) ) ;
#44981 = CARTESIAN_POINT ( 'NONE',  ( 919.9999999999993179, 154.9999999999998863, -350.0000000000000000 ) ) ;
#44982 = CARTESIAN_POINT ( 'NONE',  ( 748.6759233522253680, -112.3726999360621761, 324.3348316497537098 ) ) ;
#44983 = CARTESIAN_POINT ( 'NONE',  ( 787.5162901302840055, -299.3618753856922581, -305.4481719005792684 ) ) ;
#44984 = EDGE_CURVE ( 'NONE', #45600, #24990, #33607, .T. ) ;
#44985 = DIRECTION ( 'NONE',  ( 0.000000000000000000, -0.6594541114781790059, 0.7517448203044204691 ) ) ;
#44986 = DIRECTION ( 'NONE',  ( -1.000000000000000000, -0.000000000000000000, -0.000000000000000000 ) ) ;
#44987 = CARTESIAN_POINT ( 'NONE',  ( 755.0636971347428243, -172.2709662947836478, 341.7834795799807353 ) ) ;
#44988 = ORIENTED_EDGE ( 'NONE', *, *, #29752, .T. ) ;
#44989 = CARTESIAN_POINT ( 'NONE',  ( 795.8262568251477660, -430.3726999360611671, 308.3538107759623585 ) ) ;
#44990 = CARTESIAN_POINT ( 'NONE',  ( 747.3154664389472828, -379.9874144716865203, -326.4474001241230781 ) ) ;
#44991 = CARTESIAN_POINT ( 'NONE',  ( 767.6429770376289525, -129.1800572038746111, -306.8695393053162093 ) ) ;
#44992 = CARTESIAN_POINT ( 'NONE',  ( 804.8461984189677878, -50.19088175424420939, 336.9566956441385628 ) ) ;
#44993 = CARTESIAN_POINT ( 'NONE',  ( 787.4397851343537695, -381.7255117493284615, -374.2001403089903988 ) ) ;
#44994 = DIRECTION ( 'NONE',  ( 0.000000000000000000, 1.000000000000000000, 0.000000000000000000 ) ) ;
#44995 = CARTESIAN_POINT ( 'NONE',  ( 780.5290396650775619, -420.3510508353225532, 365.2837595273619513 ) ) ;
#44996 = VERTEX_POINT ( 'NONE', #5658 ) ;
#44997 = EDGE_CURVE ( 'NONE', #38426, #23858, #22521, .T. ) ;
#44998 = CARTESIAN_POINT ( 'NONE',  ( 764.3348316497523456, -142.7146871989599219, -308.6759233522265617 ) ) ;
#44999 = CARTESIAN_POINT ( 'NONE',  ( 914.9999999999992042, 56.60618624968562074, 350.0000000000000000 ) ) ;
#45000 = CARTESIAN_POINT ( 'NONE',  ( 793.4146539503750546, -289.9874144716866908, 307.6481478633938877 ) ) ;
#45001 = CARTESIAN_POINT ( 'NONE',  ( 785.3141322388236176, -93.72551174932934259, 364.4286716492789537 ) ) ;
#45002 = ORIENTED_EDGE ( 'NONE', *, *, #36874, .T. ) ;
#45003 = CARTESIAN_POINT ( 'NONE',  ( 755.8398074228967971, 4.558040073766884248, -333.4516893846970333 ) ) ;
#45004 = CARTESIAN_POINT ( 'NONE',  ( 785.3687786644884454, -275.3618753856923149, 315.3201227861279676 ) ) ;
#45005 = CARTESIAN_POINT ( 'NONE',  ( 751.9810565676468741, -2.089148112965993231, -360.9747183278973921 ) ) ;
#45006 = DIRECTION ( 'NONE',  ( -0.000000000000000000, 1.000000000000000000, -0.000000000000000000 ) ) ;
#45007 = EDGE_CURVE ( 'NONE', #8754, #27855, #8451, .T. ) ;
#45008 = ORIENTED_EDGE ( 'NONE', *, *, #4964, .T. ) ;
#45009 = ORIENTED_EDGE ( 'NONE', *, *, #41702, .F. ) ;
#45010 = CARTESIAN_POINT ( 'NONE',  ( 788.7366044899766848, -179.9073299311472454, -316.5762568750059813 ) ) ;
#45011 = CARTESIAN_POINT ( 'NONE',  ( 768.9521613784389729, -417.8272453906067199, -373.2346286133773106 ) ) ;
#45012 = EDGE_CURVE ( 'NONE', #38205, #36984, #7667, .T. ) ;
#45013 = CARTESIAN_POINT ( 'NONE',  ( 785.3687786644884454, -299.3618753856922581, 315.3201227861279676 ) ) ;
#45014 = CARTESIAN_POINT ( 'NONE',  ( 762.1405469898971887, -265.5436935675106156, -357.8594530101015607 ) ) ;
#45016 = CARTESIAN_POINT ( 'NONE',  ( 811.6461892240364477, -268.7146871989595525, 324.1737431748509835 ) ) ;
#45015 = CARTESIAN_POINT ( 'NONE',  ( 763.2262854647970016, -368.6346026584193964, 309.2812353651462445 ) ) ;
#45017 = CARTESIAN_POINT ( 'NONE',  ( 808.7758568127978833, -52.16923265350567362, 320.0363995740631822 ) ) ;
#45018 = CARTESIAN_POINT ( 'NONE',  ( 757.4527132478984868, -256.3726999360617924, -329.1273215169538844 ) ) ;
#45019 = CARTESIAN_POINT ( 'NONE',  ( 788.7366044899766848, -227.9073299311471033, -316.5762568750059813 ) ) ;
#45020 = CARTESIAN_POINT ( 'NONE',  ( 759.9864689768902508, -434.0891481129646081, -354.9819416627836404 ) ) ;
#45021 = CARTESIAN_POINT ( 'NONE',  ( 762.1405469898971887, -241.5436935675106156, 357.8594530101015607 ) ) ;
#45022 = VERTEX_POINT ( 'NONE', #25982 ) ;
#45023 = CARTESIAN_POINT ( 'NONE',  ( 777.5031285880264704, -358.8164208402375834, 374.9108240113588408 ) ) ;
#45024 = CARTESIAN_POINT ( 'NONE',  ( -78.83651009197140525, 260.0000000000000568, -199.9999999999936051 ) ) ;
#45025 = CARTESIAN_POINT ( 'NONE',  ( 757.7880784355613741, -66.00906357242595845, -312.4576283171834916 ) ) ;
#45026 = CARTESIAN_POINT ( 'NONE',  ( 795.2725662613897839, 16.45630643248849267, 314.1785221222716586 ) ) ;
#45027 = DIRECTION ( 'NONE',  ( 1.000000000000000000, 0.000000000000000000, 0.000000000000000000 ) ) ;
#45028 = CARTESIAN_POINT ( 'NONE',  ( 796.9571628226829034, -215.4636090269709712, 321.2382568024804641 ) ) ;
#45029 = CARTESIAN_POINT ( 'NONE',  ( 794.9819416627830151, -132.9982390220564810, 319.9864689768909898 ) ) ;
#45030 = CARTESIAN_POINT ( 'NONE',  ( 799.2566176426618085, -24.00906357242609346, -324.0069404352559559 ) ) ;
#45031 = CARTESIAN_POINT ( 'NONE',  ( 787.5162901302840055, -83.36187538569299704, -305.4481719005793252 ) ) ;
#45032 = CARTESIAN_POINT ( 'NONE',  ( 763.2154366446407039, -309.6237781080502600, 321.4292242960311228 ) ) ;
#45033 = CARTESIAN_POINT ( 'NONE',  ( 774.6858677611749044, -417.7255117493283478, -315.5713283507209894 ) ) ;
#45034 = CARTESIAN_POINT ( 'NONE',  ( 804.9363028652555840, -40.27096629478405987, -338.2165204200192079 ) ) ;
#45035 = EDGE_CURVE ( 'NONE', #39971, #45077, #43761, .T. ) ;
#45036 = CARTESIAN_POINT ( 'NONE',  ( 808.3070685750230950, -450.9982390220554294, 361.1904061080339261 ) ) ;
#45037 = CARTESIAN_POINT ( 'NONE',  ( 797.8594530101008786, 10.45630643248850866, -322.1405469898980982 ) ) ;
#45038 = CARTESIAN_POINT ( 'NONE',  ( 813.1304606946830518, -185.9073299311472454, -352.3570229623690580 ) ) ;
#45039 = EDGE_CURVE ( 'NONE', #11223, #2103, #34054, .T. ) ;
#45040 = CARTESIAN_POINT ( 'NONE',  ( 787.5162901302840055, -83.36187538569296862, 305.4481719005792684 ) ) ;
#45041 = CARTESIAN_POINT ( 'NONE',  ( 747.2067596250078623, -171.1800572038745543, 352.2312462859687230 ) ) ;
#45042 = CARTESIAN_POINT ( 'NONE',  ( 786.4999999999993179, -544.8427095258973623, -350.0000000000000000 ) ) ;
#45043 = DIRECTION ( 'NONE',  ( 1.000000000000000000, 0.000000000000000000, 0.000000000000000000 ) ) ;
#45044 = CARTESIAN_POINT ( 'NONE',  ( 748.3538107759620743, -256.7146871989595525, -355.8262568251490165 ) ) ;
#45045 = CARTESIAN_POINT ( 'NONE',  ( 750.9282345327678740, -424.9181544815158986, 319.8311093483690115 ) ) ;
#45046 = CARTESIAN_POINT ( 'NONE',  ( 813.1304606946830518, -281.9073299311468759, -352.3570229623690580 ) ) ;
#45047 = DIRECTION ( 'NONE',  ( 0.000000000000000000, 0.000000000000000000, 1.000000000000000000 ) ) ;
#45048 = CARTESIAN_POINT ( 'NONE',  ( 754.9967657858570647, -409.5436935675101040, 365.0032342141425374 ) ) ;
#45049 = CARTESIAN_POINT ( 'NONE',  ( 767.7687537140311633, -23.90732993114773919, 372.7932403749916830 ) ) ;
#45050 = CARTESIAN_POINT ( 'NONE',  ( 764.8639956371174549, -344.0891481129647786, -319.7806653035542013 ) ) ;
#45051 = EDGE_CURVE ( 'NONE', #22547, #11840, #12141, .T. ) ;
#45052 = CARTESIAN_POINT ( 'NONE',  ( 804.1601925771018387, -7.441959926233078448, 346.5483106153029098 ) ) ;
#45053 = CARTESIAN_POINT ( 'NONE',  ( 759.8311093483677041, -46.16923265350568784, -310.9282345327691814 ) ) ;
#45054 = CARTESIAN_POINT ( 'NONE',  ( 758.6633372737375112, -140.5328690171417634, -326.9102291470432533 ) ) ;
#45055 = CARTESIAN_POINT ( 'NONE',  ( 768.8385539511368734, -167.2601417444143976, 306.4236121716840557 ) ) ;
#45056 = CARTESIAN_POINT ( 'NONE',  ( 781.8018195045267476, 1.729033705215812233, 365.1927285166407273 ) ) ;
#45057 = ORIENTED_EDGE ( 'NONE', *, *, #10834, .F. ) ;
#45058 = CARTESIAN_POINT ( 'NONE',  ( 758.0580252608178853, -78.45278447660211896, -328.0187753319985404 ) ) ;
#45059 = CARTESIAN_POINT ( 'NONE',  ( 798.7617431975189675, -171.6237781080507432, -323.0428371773161871 ) ) ;
#45060 = UNCERTAINTY_MEASURE_WITH_UNIT (LENGTH_MEASURE( 1.000000000000000082E-05 ), #37692, 'distance_accuracy_value', 'NONE');
#45061 = CARTESIAN_POINT ( 'NONE',  ( 759.9864689768902508, -170.0891481129654608, 354.9819416627836404 ) ) ;
#45062 = PRODUCT_DEFINITION_SHAPE ( 'NONE', 'NONE',  #45736 ) ;
#45063 = CARTESIAN_POINT ( 'NONE',  ( 776.2433038121456548, 11.10349461922141145, -374.8207195650711014 ) ) ;
#45065 = CARTESIAN_POINT ( 'NONE',  ( 774.6312213355098493, -311.3618753856923149, 364.6798772138717482 ) ) ;
#45064 = CARTESIAN_POINT ( 'NONE',  ( 756.3353852180819104, -293.9073299311468759, 331.1735550268788302 ) ) ;
#45066 = LINE ( 'NONE', #10397, #25680 ) ;
#45067 = VERTEX_POINT ( 'NONE', #23189 ) ;
#45068 = CARTESIAN_POINT ( 'NONE',  ( 761.2382568024794409, -15.62377810805123524, 356.9571628226838129 ) ) ;
#45069 = CARTESIAN_POINT ( 'NONE',  ( 810.4231160770870019, -312.5545181178797520, -321.9338519418446936 ) ) ;
#45070 =( BOUNDED_CURVE ( )  B_SPLINE_CURVE ( 2, ( #27534, #13006, #27318, #9761, #3060, #31235, #45330, #24294, #38400, #6750, #20824, #17384, #31467, #38626, #34007, #2361, #41186, #21070, #35153, #17616, #6985, #31685, #3531, #12945, #19639, #9702, #20090, #23545, #37648, #6227, #23766, #27031, #31171, #12703, #19873, #5545, #23323, #41130, #9482, #9926, #16401, #41815, #16641, #30481, #30255, #10161, #13181, #27262, #24237, #5997, #34165, #45268, #20319, #2082, #2536, #41352, #33733, #23999, #37427, #2781, #44584, #17092, #27476, #26783, #16174, #16873, #30955, #27711, #44347, #37879, #41574, #30729, #5784, #38121, #45049, #34412, #44823, #13404, #6474, #3004, #33951, #40888, #9255, #20550, #2302, #34647, #13627, #10614, #7388, #28387, #39039, #42035, #35091, #14558, #14315, #42256, #7165, #18256, #31631, #11078, #3466, #10381, #4162, #32084, #17559, #31849, #6868, #6691, #42490, #21239, #24690, #38809, #21464, #10856, #14088, #32330, #45510, #6918, #38346, #24457, #28163, #42937, #35319, #31405, #20769, #3697, #17784, #14784, #221, #27939, #38564, #34860, #21690, #684, #13863, #24925, #35542, #20998, #3917, #18012, #455, #3224, #28635, #42714, #25146, #39258, #7613, #35783, #28856, #11304, #17314, #411, #28341, #12346, #22724, #26422, #28816, #26193, #21426, #21200, #7574, #12113, #35502, #43971, #40309, #19259, #39221, #3877, #5173, #14515, #28593, #10812, #33347, #1477, #32041, #641, #42677, #35281, #11263, #21650, #25107, #19050, #35737, #8662, #179, #1690, #36820, #15794, #4116, #18211, #14742, #7121, #11040, #14272, #3658, #32285, #42897, #29884, #25338, #42441, #24885, #17746, #31810, #39454, #21889, #38999, #36604, #4958, #33141, #15577, #29658, #7349, #43735, #17969, #30802, #41426, #34243, #26635, #16031, #13255, #5386, #12559, #30558, #9558, #30112, #40731, #23618, #2618, #44660, #40522, #45122, #44895, #9088, #27333, #5625, #23155, #37264, #22937, #19719, #37726, #33806, #2378, #13480, #2159, #9328, #34492, #41201, #37033, #12776, #16479, #8873, #9775, #16251, #6078, #30328, #20166, #16718, #13021, #19480, #27111, #33576, #16945, #1928, #23844, #37956, #44422, #26855, #6315, #20397, #2852, #40966, #31024, #44201, #23397, #37499, #5859, #19947, #34023, #31487, #24081, #41888, #6541, #24776, #38195, #17164, #10934, #10456, #17637, #41655, #31701, #42106, #45588, #13936, #28232, #68, #3307, #7463, #34715, #10231, #27551, #45350, #21091, #32170, #20842, #20621, #10011, #34941, #28011, #3990, #24533, #13712, #27790, #3073, #25003, #35618, #24311, #35176, #7003, #38416, #6767, #38646, #3552, #14161, #42327, #10691, #17856, #28474, #21318, #38892, #7246, #294, #35393, #3766, #31922, #533, #42575, #14393, #39114, #21536, #18087, #28710, #19210, #18997, #28935, #33089, #25458, #32409, #11376, #42790, #39578, #11833, #43012, #758, #36539, #8152, #29394, #11152, #43686, #25221, #40247, #29609, #33297, #1426, #14858, #25904, #7935, #40013, #15312, #18768, #39333, #4669, #7688, #11616, #8365, #32854, #32626, #29160, #21767, #971, #35862, #36308, #25693, #36766, #4239, #5122, #18329, #15074, #22002, #43245, #39804, #1204, #43465, #36092, #22433, #4457, #18546, #12059, #22215, #4898, #14637, #15528, #26133, #8605, #22670, #20112, #12505, #19429, #23567, #1642, #34187, #8821, #9503, #40679, #9033, #5334, #13204, #41152, #26581, #40909, #23103, #15743, #16663, #23788, #22889, #12967, #30275, #6021, #40469, #44842, #30748, #27282, #44368, #2105, #9276, #6253, #37205, #36981, #29831, #5569, #19661, #37900, #41375, #44606, #33754, #2558, #20341, #19894, #23345, #9723, #12723, #37448, #27056, #16195, #26803, #43912, #5807, #15976, #37671, #12290, #26367, #33521, #1869, #30059, #44141, #33972, #2323, #16421, #30503, #6492, #3489, #28180, #24478, #34435, #39059, #38832, #3025, #7184, #45290, #20570, #31193, #16892, #13426, #24943, #42053, #10401, #7407, #41834, #3246, #28413, #35111, #30973, #6710, #38584, #2801, #21259, #34666, #31647, #13650, #15, #17577, #6940, #45071, #14106, #42272, #10876, #27495, #21022, #10633, #24256, #17112, #35338, #24713, #3714, #27731, #17801, #31867, #238, #10180, #38141, #24022, #9951, #31424, #14335, #42511, #41595, #38364, #20787, #34882, #17336, #45530, #13882, #27957, #25855, #33038, #7877, #35805, #18943, #4402, #21953, #15016, #26067, #29105, #18492, #43189, #4181, #11558, #36039, #1377, #18706, #14800, #39965, #43634, #39753, #25640, #15480, #32568, #8101, #32796, #28875, #25400, #21481, #1150, #43417, #29560, #39522, #35559, #914, #12003, #21708, #11096, #39275, #22163, #36252, #25166, #7630, #4609, #15255, #29344, #3934, #40180, #8310, #11784, #18029, #32110, #475, #22373, #704, #14580, #28654, #36479, #4843, #42731, #42955, #18276, #32350, #11322, #5070, #26531, #30223, #13145, #12907, #5507, #5964, #36710, #20053, #30444, #15689, #22610, #19834, #5746, #30693, #1590, #16140, #44546, #44086, #26311, #26994, #2268, #40852, #1809, #37391, #19161, #44790, #29771, #40629, #33461, #8981, #19603, #12669, #26749, #33245, #33917, #43849, #12231, #37610, #37148, #44314, #27226, #41091, #34131, #23050, #15916, #9446, #19377, #40417, #23510, #8546, #2499, #8769, #16365, #33696, #2045, #16606, #22836, #36930, #5284, #9215, #29999, #12452, #23290, #10577, #41318, #13368, #31368, #10349, #30919, #27440, #24424, #35057, #45476, #9667, #187, #45706, #9890, #14057, #6441, #41539, #38086, #23733, #20520, #38528, #23964, #17528, #34826, #6882, #37844, #24654, #6192, #21207, #38771, #35288, #3431, #2746, #38312, #7129, #20284, #3666, #31601, #16841, #34377, #20958, #6659, #28128, #13832, #13592, #10129, #45015, #27674, #34613, #17277, #17057, #20732, #17753, #2969, #31817, #31134, #41780, #45231, #24203, #3190, #27909, #42006, #42224, #14279, #18440, #29054, #32047, #25114, #4567, #4349, #32294, #42904, #8260, #21658, #1094, #39228, #419, #18658, #28349, #15208, #35509, #35746, #42452, #32518, #11271, #649, #14751, #43140, #866, #4126, #22326, #3884, #42682, #10820, #14524, #18219, #28824, #39462, #35984, #25347, #14969, #7820, #4790, #21899, #17977, #28600, #24892, #11736, #36427, #21433, #11507, #25592, #11049, #7581, #39702, #36203, #32747, #8050, #22114, #29296, #18894, #43371, #25805, #39918, #32989, #39006, #1327, #7357, #19326, #15431, #8932, #29719, #5699, #16317, #9158, #1540, #36665, #33870, #26016, #8725, #5025, #30176, #19115, #33203, #44267, #23231, #5453, #29508, #20009, #19786, #43797, #2223, #26261, #15636, #12178, #43581, #40374, #12625, #22790, #36885, #37337, #5236, #29952, #9395, #16092, #11949, #33410, #37097, #34085, #30399, #1754, #26703, #15861, #40801, #44493, #19547, #40127, #33644, #8490, #12405, #12851, #23003, #26933, #44035, #26485, #41035, #23463, #1997, #40586, #37562, #5919, #22561, #2692, #6144, #37795, #23684, #6390, #44735, #16788, #9843, #20472, #13095, #20234 ),
 .UNSPECIFIED., .F., .T. ) 
 B_SPLINE_CURVE_WITH_KNOTS ( ( 3, 2, 2, 2, 2, 2, 2, 2, 2, 2, 2, 2, 2, 2, 2, 2, 2, 2, 2, 2, 2, 2, 2, 2, 2, 2, 2, 2, 2, 2, 2, 2, 2, 2, 2, 2, 2, 2, 2, 2, 2, 2, 2, 2, 2, 2, 2, 2, 2, 2, 2, 2, 2, 2, 2, 2, 2, 2, 2, 2, 2, 2, 2, 2, 2, 2, 2, 2, 2, 2, 2, 2, 2, 2, 2, 2, 2, 2, 2, 2, 2, 2, 2, 2, 2, 2, 2, 2, 2, 2, 2, 2, 2, 2, 2, 2, 2, 2, 2, 2, 2, 2, 2, 2, 2, 2, 2, 2, 2, 2, 2, 2, 2, 2, 2, 2, 2, 2, 2, 2, 2, 2, 2, 2, 2, 2, 2, 2, 2, 2, 2, 2, 2, 2, 2, 2, 2, 2, 2, 2, 2, 2, 2, 2, 2, 2, 2, 2, 2, 2, 2, 2, 2, 2, 2, 2, 2, 2, 2, 2, 2, 2, 2, 2, 2, 2, 2, 2, 2, 2, 2, 2, 2, 2, 2, 2, 2, 2, 2, 2, 2, 2, 2, 2, 2, 2, 2, 2, 2, 2, 2, 2, 2, 2, 2, 2, 2, 2, 2, 2, 2, 2, 2, 2, 2, 2, 2, 2, 2, 2, 2, 2, 2, 2, 2, 2, 2, 2, 2, 2, 2, 2, 2, 2, 2, 2, 2, 2, 2, 2, 2, 2, 2, 2, 2, 2, 2, 2, 2, 2, 2, 2, 2, 2, 2, 2, 2, 2, 2, 2, 2, 2, 2, 2, 2, 2, 2, 2, 2, 2, 2, 2, 2, 2, 2, 2, 2, 2, 2, 2, 2, 2, 2, 2, 2, 2, 2, 2, 2, 2, 2, 2, 2, 2, 2, 2, 2, 2, 2, 2, 2, 2, 2, 2, 2, 2, 2, 2, 2, 2, 2, 2, 2, 2, 2, 2, 2, 2, 2, 2, 2, 2, 2, 2, 2, 2, 2, 2, 2, 2, 2, 2, 2, 2, 2, 2, 2, 2, 2, 2, 2, 2, 2, 2, 2, 2, 2, 2, 2, 2, 2, 2, 2, 2, 2, 2, 2, 2, 2, 2, 2, 2, 2, 2, 2, 2, 2, 2, 2, 2, 2, 2, 2, 2, 2, 2, 2, 2, 2, 2, 2, 2, 2, 2, 2, 2, 2, 2, 2, 2, 2, 2, 2, 2, 2, 2, 2, 2, 2, 2, 2, 2, 2, 2, 2, 2, 2, 2, 2, 2, 2, 2, 2, 2, 2, 2, 2, 2, 2, 2, 2, 2, 2, 2, 2, 2, 2, 2, 2, 2, 2, 2, 2, 2, 2, 2, 2, 2, 2, 2, 2, 3 ),
 ( 8.755858387967423303E-18, 0.002272727272727281290, 0.004545454545454553907, 0.006818181818181826524, 0.009090909090909099141, 0.01136363636363637263, 0.01363636363636364437, 0.01590909090909091786, 0.01818181818181819134, 0.02045454545454546483, 0.02272727272727273831, 0.02500000000000001180, 0.02727272727272728181, 0.02954545454545455530, 0.03181818181818182184, 0.03409090909090909532, 0.03636363636363636881, 0.03863636363636364229, 0.04090909090909091578, 0.04318181818181818926, 0.04545454545454546275, 0.04772727272727273623, 0.05000000000000000971, 0.05227272727272727626, 0.05454545454545454974, 0.05681818181818182323, 0.05909090909090909671, 0.06136363636363637020, 0.06363636363636364368, 0.06590909090909091717, 0.06818181818181819065, 0.07045454545454546413, 0.07272727272727273762, 0.07500000000000001110, 0.07727272727272728459, 0.07954545454545455807, 0.08181818181818183155, 0.08409090909090910504, 0.08636363636363637852, 0.08863636363636365201, 0.09090909090909092549, 0.09318181818181819898, 0.09545454545454547246, 0.09772727272727274594, 0.1000000000000000194, 0.1022727272727272929, 0.1045454545454545525, 0.1068181818181818260, 0.1090909090909090995, 0.1113636363636363730, 0.1136363636363636465, 0.1159090909090909199, 0.1181818181818181934, 0.1204545454545454669, 0.1227272727272727404, 0.1250000000000000000, 0.1272727272727272596, 0.1295454545454545470, 0.1318181818181818066, 0.1340909090909090939, 0.1363636363636363535, 0.1386363636363636409, 0.1409090909090909005, 0.1431818181818181879, 0.1454545454545454475, 0.1477272727272727348, 0.1499999999999999944, 0.1522727272727272818, 0.1545454545454545414, 0.1568181818181818288, 0.1590909090909090884, 0.1613636363636363757, 0.1636363636363636354, 0.1659090909090909227, 0.1681818181818181823, 0.1704545454545454419, 0.1727272727272727293, 0.1749999999999999889, 0.1772727272727272763, 0.1795454545454545359, 0.1818181818181818232, 0.1840909090909090828, 0.1863636363636363702, 0.1886363636363636298, 0.1909090909090909172, 0.1931818181818181768, 0.1954545454545454641, 0.1977272727272727237, 0.2000000000000000111, 0.2022727272727272707, 0.2045454545454545581, 0.2068181818181818177, 0.2090909090909090773, 0.2113636363636363646, 0.2136363636363636243, 0.2159090909090909116, 0.2181818181818181712, 0.2204545454545454586, 0.2227272727272727182, 0.2250000000000000056, 0.2272727272727272652, 0.2295454545454545525, 0.2318181818181818121, 0.2340909090909090995, 0.2363636363636363591, 0.2386363636363636465, 0.2409090909090909061, 0.2431818181818181934, 0.2454545454545454530, 0.2477272727272727404, 0.2500000000000000000, 0.2522727272727272596, 0.2545454545454545192, 0.2568181818181818343, 0.2590909090909090939, 0.2613636363636363535, 0.2636363636363636131, 0.2659090909090909283, 0.2681818181818181879, 0.2704545454545454475, 0.2727272727272727071, 0.2750000000000000222, 0.2772727272727272818, 0.2795454545454545414, 0.2818181818181818010, 0.2840909090909091161, 0.2863636363636363757, 0.2886363636363636354, 0.2909090909090908950, 0.2931818181818181546, 0.2954545454545454697, 0.2977272727272727293, 0.2999999999999999889, 0.3022727272727272485, 0.3045454545454545636, 0.3068181818181818232, 0.3090909090909090828, 0.3113636363636363424, 0.3136363636363636576, 0.3159090909090909172, 0.3181818181818181768, 0.3204545454545454364, 0.3227272727272727515, 0.3250000000000000111, 0.3272727272727272707, 0.3295454545454545303, 0.3318181818181818454, 0.3340909090909091050, 0.3363636363636363646, 0.3386363636363636243, 0.3409090909090908839, 0.3431818181818181990, 0.3454545454545454586, 0.3477272727272727182, 0.3499999999999999778, 0.3522727272727272929, 0.3545454545454545525, 0.3568181818181818121, 0.3590909090909090717, 0.3613636363636363869, 0.3636363636363636465, 0.3659090909090909061, 0.3681818181818181657, 0.3704545454545454808, 0.3727272727272727404, 0.3749999999999999445, 0.3772727272727272596, 0.3795454545454545192, 0.3818181818181818343, 0.3840909090909090939, 0.3863636363636363535, 0.3886363636363636131, 0.3909090909090909283, 0.3931818181818181879, 0.3954545454545454475, 0.3977272727272727071, 0.4000000000000000222, 0.4022727272727272818, 0.4045454545454545414, 0.4068181818181818010, 0.4090909090909091161, 0.4113636363636363757, 0.4136363636363636354, 0.4159090909090908950, 0.4181818181818181546, 0.4204545454545454697, 0.4227272727272727293, 0.4249999999999999889, 0.4272727272727272485, 0.4295454545454545636, 0.4318181818181818232, 0.4340909090909090828, 0.4363636363636363424, 0.4386363636363636576, 0.4409090909090909172, 0.4431818181818181768, 0.4454545454545454364, 0.4477272727272727515, 0.4500000000000000111, 0.4522727272727272707, 0.4545454545454545303, 0.4568181818181818454, 0.4590909090909091050, 0.4613636363636363646, 0.4636363636363636243, 0.4659090909090908839, 0.4681818181818181990, 0.4704545454545454586, 0.4727272727272727182, 0.4749999999999999778, 0.4772727272727272929, 0.4795454545454545525, 0.4818181818181818121, 0.4840909090909090717, 0.4863636363636363869, 0.4886363636363636465, 0.4909090909090909061, 0.4931818181818181657, 0.4954545454545454808, 0.4977272727272727404, 0.5000000000000000000, 0.5022727272727273151, 0.5045454545454545192, 0.5068181818181818343, 0.5090909090909090384, 0.5113636363636363535, 0.5136363636363636687, 0.5159090909090908728, 0.5181818181818181879, 0.5204545454545455030, 0.5227272727272727071, 0.5250000000000000222, 0.5272727272727272263, 0.5295454545454545414, 0.5318181818181818565, 0.5340909090909090606, 0.5363636363636363757, 0.5386363636363636909, 0.5409090909090908950, 0.5431818181818182101, 0.5454545454545454142, 0.5477272727272727293, 0.5500000000000000444, 0.5522727272727272485, 0.5545454545454545636, 0.5568181818181817677, 0.5590909090909090828, 0.5613636363636363980, 0.5636363636363636020, 0.5659090909090909172, 0.5681818181818182323, 0.5704545454545454364, 0.5727272727272727515, 0.5749999999999999556, 0.5772727272727272707, 0.5795454545454545858, 0.5818181818181817899, 0.5840909090909091050, 0.5863636363636363091, 0.5886363636363636243, 0.5909090909090909394, 0.5931818181818181435, 0.5954545454545454586, 0.5977272727272727737, 0.5999999999999999778, 0.6022727272727272929, 0.6045454545454544970, 0.6068181818181818121, 0.6090909090909091272, 0.6113636363636362203, 0.6136363636363636465, 0.6159090909090909616, 0.6181818181818181657, 0.6204545454545454808, 0.6227272727272726849, 0.6250000000000000000, 0.6272727272727273151, 0.6295454545454546302, 0.6318181818181818343, 0.6340909090909090384, 0.6363636363636363535, 0.6386363636363636687, 0.6409090909090908728, 0.6431818181818181879, 0.6454545454545455030, 0.6477272727272727071, 0.6500000000000000222, 0.6522727272727272263, 0.6545454545454545414, 0.6568181818181818565, 0.6590909090909090606, 0.6613636363636363757, 0.6636363636363636909, 0.6659090909090908950, 0.6681818181818182101, 0.6704545454545454142, 0.6727272727272727293, 0.6750000000000000444, 0.6772727272727272485, 0.6795454545454545636, 0.6818181818181817677, 0.6840909090909090828, 0.6863636363636363980, 0.6886363636363636020, 0.6909090909090909172, 0.6931818181818182323, 0.6954545454545454364, 0.6977272727272727515, 0.6999999999999999556, 0.7022727272727272707, 0.7045454545454545858, 0.7068181818181817899, 0.7090909090909091050, 0.7113636363636363091, 0.7136363636363636243, 0.7159090909090909394, 0.7181818181818181435, 0.7204545454545454586, 0.7227272727272727737, 0.7249999999999999778, 0.7272727272727272929, 0.7295454545454544970, 0.7318181818181818121, 0.7340909090909091272, 0.7363636363636363313, 0.7386363636363636465, 0.7409090909090909616, 0.7431818181818181657, 0.7454545454545454808, 0.7477272727272726849, 0.7499999999999998890, 0.7522727272727273151, 0.7545454545454545192, 0.7568181818181818343, 0.7590909090909090384, 0.7613636363636363535, 0.7636363636363636687, 0.7659090909090908728, 0.7681818181818181879, 0.7704545454545455030, 0.7727272727272727071, 0.7750000000000000222, 0.7772727272727272263, 0.7795454545454545414, 0.7818181818181818565, 0.7840909090909090606, 0.7863636363636363757, 0.7886363636363636909, 0.7909090909090908950, 0.7931818181818182101, 0.7954545454545454142, 0.7977272727272727293, 0.8000000000000000444, 0.8022727272727272485, 0.8045454545454545636, 0.8068181818181817677, 0.8090909090909090828, 0.8113636363636363980, 0.8136363636363636020, 0.8159090909090909172, 0.8181818181818182323, 0.8204545454545454364, 0.8227272727272727515, 0.8249999999999999556, 0.8272727272727272707, 0.8295454545454545858, 0.8318181818181817899, 0.8340909090909091050, 0.8363636363636363091, 0.8386363636363636243, 0.8409090909090909394, 0.8431818181818181435, 0.8454545454545454586, 0.8477272727272727737, 0.8499999999999999778, 0.8522727272727272929, 0.8545454545454544970, 0.8568181818181818121, 0.8590909090909091272, 0.8613636363636363313, 0.8636363636363636465, 0.8659090909090909616, 0.8681818181818181657, 0.8704545454545453698, 0.8727272727272726849, 0.8750000000000000000, 0.8772727272727273151, 0.8795454545454545192, 0.8818181818181818343, 0.8840909090909090384, 0.8863636363636363535, 0.8886363636363637797, 0.8909090909090908728, 0.8931818181818181879, 0.8954545454545455030, 0.8977272727272727071, 0.9000000000000000222, 0.9022727272727272263, 0.9045454545454545414, 0.9068181818181818565, 0.9090909090909090606, 0.9113636363636363757, 0.9136363636363636909, 0.9159090909090908950, 0.9181818181818182101, 0.9204545454545454142, 0.9227272727272727293, 0.9250000000000000444, 0.9272727272727272485, 0.9295454545454545636, 0.9318181818181817677, 0.9340909090909090828, 0.9363636363636363980, 0.9386363636363636020, 0.9409090909090909172, 0.9431818181818182323, 0.9454545454545454364, 0.9477272727272727515, 0.9499999999999999556, 0.9522727272727272707, 0.9545454545454545858, 0.9568181818181817899, 0.9590909090909091050, 0.9613636363636363091, 0.9636363636363636243, 0.9659090909090909394, 0.9681818181818181435, 0.9704545454545454586, 0.9727272727272727737, 0.9749999999999999778, 0.9772727272727272929, 0.9781254700864302487 ),
 .UNSPECIFIED. ) 
 CURVE ( )  GEOMETRIC_REPRESENTATION_ITEM ( )  RATIONAL_B_SPLINE_CURVE ( ( 1.000000000000000000, 0.9898214418809326842, 1.000000000000000000, 0.9898214418809326842, 1.000000000000000000, 0.9898214418809326842, 1.000000000000000000, 0.9898214418809326842, 1.000000000000000000, 0.9898214418809326842, 1.000000000000000000, 0.9898214418809326842, 1.000000000000000000, 0.9898214418809326842, 1.000000000000000000, 0.9898214418809326842, 1.000000000000000000, 0.9898214418809326842, 1.000000000000000000, 0.9898214418809326842, 1.000000000000000000, 0.9898214418809326842, 1.000000000000000000, 0.9898214418809326842, 1.000000000000000000, 0.9898214418809326842, 1.000000000000000000, 0.9898214418809326842, 1.000000000000000000, 0.9898214418809326842, 1.000000000000000000, 0.9898214418809326842, 1.000000000000000000, 0.9898214418809326842, 1.000000000000000000, 0.9898214418809326842, 1.000000000000000000, 0.9898214418809326842, 1.000000000000000000, 0.9898214418809326842, 1.000000000000000000, 0.9898214418809326842, 1.000000000000000000, 0.9898214418809326842, 1.000000000000000000, 0.9898214418809326842, 1.000000000000000000, 0.9898214418809326842, 1.000000000000000000, 0.9898214418809326842, 1.000000000000000000, 0.9898214418809326842, 1.000000000000000000, 0.9898214418809326842, 1.000000000000000000, 0.9898214418809326842, 1.000000000000000000, 0.9898214418809326842, 1.000000000000000000, 0.9898214418809326842, 1.000000000000000000, 0.9898214418809326842, 1.000000000000000000, 0.9898214418809326842, 1.000000000000000000, 0.9898214418809326842, 1.000000000000000000, 0.9898214418809326842, 1.000000000000000000, 0.9898214418809326842, 1.000000000000000000, 0.9898214418809326842, 1.000000000000000000, 0.9898214418809326842, 1.000000000000000000, 0.9898214418809326842, 1.000000000000000000, 0.9898214418809326842, 1.000000000000000000, 0.9898214418809326842, 1.000000000000000000, 0.9898214418809326842, 1.000000000000000000, 0.9898214418809326842, 1.000000000000000000, 0.9898214418809326842, 1.000000000000000000, 0.9898214418809326842, 1.000000000000000000, 0.9898214418809326842, 1.000000000000000000, 0.9898214418809326842, 1.000000000000000000, 0.9898214418809326842, 1.000000000000000000, 0.9898214418809326842, 1.000000000000000000, 0.9898214418809326842, 1.000000000000000000, 0.9898214418809326842, 1.000000000000000000, 0.9898214418809326842, 1.000000000000000000, 0.9898214418809326842, 1.000000000000000000, 0.9898214418809326842, 1.000000000000000000, 0.9898214418809326842, 1.000000000000000000, 0.9898214418809326842, 1.000000000000000000, 0.9898214418809326842, 1.000000000000000000, 0.9898214418809326842, 1.000000000000000000, 0.9898214418809326842, 1.000000000000000000, 0.9898214418809326842, 1.000000000000000000, 0.9898214418809326842, 1.000000000000000000, 0.9898214418809326842, 1.000000000000000000, 0.9898214418809326842, 1.000000000000000000, 0.9898214418809326842, 1.000000000000000000, 0.9898214418809326842, 1.000000000000000000, 0.9898214418809326842, 1.000000000000000000, 0.9898214418809326842, 1.000000000000000000, 0.9898214418809326842, 1.000000000000000000, 0.9898214418809326842, 1.000000000000000000, 0.9898214418809326842, 1.000000000000000000, 0.9898214418809326842, 1.000000000000000000, 0.9898214418809326842, 1.000000000000000000, 0.9898214418809326842, 1.000000000000000000, 0.9898214418809326842, 1.000000000000000000, 0.9898214418809326842, 1.000000000000000000, 0.9898214418809326842, 1.000000000000000000, 0.9898214418809326842, 1.000000000000000000, 0.9898214418809326842, 1.000000000000000000, 0.9898214418809326842, 1.000000000000000000, 0.9898214418809326842, 1.000000000000000000, 0.9898214418809326842, 1.000000000000000000, 0.9898214418809326842, 1.000000000000000000, 0.9898214418809326842, 1.000000000000000000, 0.9898214418809326842, 1.000000000000000000, 0.9898214418809326842, 1.000000000000000000, 0.9898214418809326842, 1.000000000000000000, 0.9898214418809326842, 1.000000000000000000, 0.9898214418809326842, 1.000000000000000000, 0.9898214418809326842, 1.000000000000000000, 0.9898214418809326842, 1.000000000000000000, 0.9898214418809326842, 1.000000000000000000, 0.9898214418809326842, 1.000000000000000000, 0.9898214418809326842, 1.000000000000000000, 0.9898214418809326842, 1.000000000000000000, 0.9898214418809326842, 1.000000000000000000, 0.9898214418809326842, 1.000000000000000000, 0.9898214418809326842, 1.000000000000000000, 0.9898214418809326842, 1.000000000000000000, 0.9898214418809326842, 1.000000000000000000, 0.9898214418809326842, 1.000000000000000000, 0.9898214418809326842, 1.000000000000000000, 0.9898214418809326842, 1.000000000000000000, 0.9898214418809326842, 1.000000000000000000, 0.9898214418809326842, 1.000000000000000000, 0.9898214418809326842, 1.000000000000000000, 0.9898214418809326842, 1.000000000000000000, 0.9898214418809326842, 1.000000000000000000, 0.9898214418809326842, 1.000000000000000000, 0.9898214418809326842, 1.000000000000000000, 0.9898214418809326842, 1.000000000000000000, 0.9898214418809326842, 1.000000000000000000, 0.9898214418809326842, 1.000000000000000000, 0.9898214418809326842, 1.000000000000000000, 0.9898214418809326842, 1.000000000000000000, 0.9898214418809326842, 1.000000000000000000, 0.9898214418809326842, 1.000000000000000000, 0.9898214418809326842, 1.000000000000000000, 0.9898214418809326842, 1.000000000000000000, 0.9898214418809326842, 1.000000000000000000, 0.9898214418809326842, 1.000000000000000000, 0.9898214418809326842, 1.000000000000000000, 0.9898214418809326842, 1.000000000000000000, 0.9898214418809326842, 1.000000000000000000, 0.9898214418809326842, 1.000000000000000000, 0.9898214418809326842, 1.000000000000000000, 0.9898214418809326842, 1.000000000000000000, 0.9898214418809326842, 1.000000000000000000, 0.9898214418809326842, 1.000000000000000000, 0.9898214418809326842, 1.000000000000000000, 0.9898214418809326842, 1.000000000000000000, 0.9898214418809326842, 1.000000000000000000, 0.9898214418809326842, 1.000000000000000000, 0.9898214418809326842, 1.000000000000000000, 0.9898214418809326842, 1.000000000000000000, 0.9898214418809326842, 1.000000000000000000, 0.9898214418809326842, 1.000000000000000000, 0.9898214418809326842, 1.000000000000000000, 0.9898214418809326842, 1.000000000000000000, 0.9898214418809326842, 1.000000000000000000, 0.9898214418809326842, 1.000000000000000000, 0.9898214418809326842, 1.000000000000000000, 0.9898214418809326842, 1.000000000000000000, 0.9898214418809326842, 1.000000000000000000, 0.9898214418809326842, 1.000000000000000000, 0.9898214418809326842, 1.000000000000000000, 0.9898214418809326842, 1.000000000000000000, 0.9898214418809326842, 1.000000000000000000, 0.9898214418809326842, 1.000000000000000000, 0.9898214418809326842, 1.000000000000000000, 0.9898214418809326842, 1.000000000000000000, 0.9898214418809326842, 1.000000000000000000, 0.9898214418809326842, 1.000000000000000000, 0.9898214418809326842, 1.000000000000000000, 0.9898214418809326842, 1.000000000000000000, 0.9898214418809326842, 1.000000000000000000, 0.9898214418809326842, 1.000000000000000000, 0.9898214418809326842, 1.000000000000000000, 0.9898214418809326842, 1.000000000000000000, 0.9898214418809326842, 1.000000000000000000, 0.9898214418809326842, 1.000000000000000000, 0.9898214418809326842, 1.000000000000000000, 0.9898214418809326842, 1.000000000000000000, 0.9898214418809326842, 1.000000000000000000, 0.9898214418809326842, 1.000000000000000000, 0.9898214418809326842, 1.000000000000000000, 0.9898214418809326842, 1.000000000000000000, 0.9898214418809326842, 1.000000000000000000, 0.9898214418809326842, 1.000000000000000000, 0.9898214418809326842, 1.000000000000000000, 0.9898214418809326842, 1.000000000000000000, 0.9898214418809326842, 1.000000000000000000, 0.9898214418809326842, 1.000000000000000000, 0.9898214418809326842, 1.000000000000000000, 0.9898214418809326842, 1.000000000000000000, 0.9898214418809326842, 1.000000000000000000, 0.9898214418809326842, 1.000000000000000000, 0.9898214418809326842, 1.000000000000000000, 0.9898214418809326842, 1.000000000000000000, 0.9898214418809326842, 1.000000000000000000, 0.9898214418809326842, 1.000000000000000000, 0.9898214418809326842, 1.000000000000000000, 0.9898214418809326842, 1.000000000000000000, 0.9898214418809326842, 1.000000000000000000, 0.9898214418809326842, 1.000000000000000000, 0.9898214418809326842, 1.000000000000000000, 0.9898214418809326842, 1.000000000000000000, 0.9898214418809326842, 1.000000000000000000, 0.9898214418809326842, 1.000000000000000000, 0.9898214418809326842, 1.000000000000000000, 0.9898214418809326842, 1.000000000000000000, 0.9898214418809326842, 1.000000000000000000, 0.9898214418809326842, 1.000000000000000000, 0.9898214418809326842, 1.000000000000000000, 0.9898214418809326842, 1.000000000000000000, 0.9898214418809326842, 1.000000000000000000, 0.9898214418809326842, 1.000000000000000000, 0.9898214418809326842, 1.000000000000000000, 0.9898214418809326842, 1.000000000000000000, 0.9898214418809326842, 1.000000000000000000, 0.9898214418809326842, 1.000000000000000000, 0.9898214418809326842, 1.000000000000000000, 0.9898214418809326842, 1.000000000000000000, 0.9898214418809326842, 1.000000000000000000, 0.9898214418809326842, 1.000000000000000000, 0.9898214418809326842, 1.000000000000000000, 0.9898214418809326842, 1.000000000000000000, 0.9898214418809326842, 1.000000000000000000, 0.9898214418809326842, 1.000000000000000000, 0.9898214418809326842, 1.000000000000000000, 0.9898214418809326842, 1.000000000000000000, 0.9898214418809326842, 1.000000000000000000, 0.9898214418809326842, 1.000000000000000000, 0.9898214418809326842, 1.000000000000000000, 0.9898214418809326842, 1.000000000000000000, 0.9898214418809326842, 1.000000000000000000, 0.9898214418809326842, 1.000000000000000000, 0.9898214418809326842, 1.000000000000000000, 0.9898214418809326842, 1.000000000000000000, 0.9898214418809326842, 1.000000000000000000, 0.9898214418809326842, 1.000000000000000000, 0.9898214418809326842, 1.000000000000000000, 0.9898214418809326842, 1.000000000000000000, 0.9898214418809326842, 1.000000000000000000, 0.9898214418809326842, 1.000000000000000000, 0.9898214418809326842, 1.000000000000000000, 0.9898214418809326842, 1.000000000000000000, 0.9898214418809326842, 1.000000000000000000, 0.9898214418809326842, 1.000000000000000000, 0.9898214418809326842, 1.000000000000000000, 0.9898214418809326842, 1.000000000000000000, 0.9898214418809326842, 1.000000000000000000, 0.9898214418809326842, 1.000000000000000000, 0.9898214418809326842, 1.000000000000000000, 0.9898214418809326842, 1.000000000000000000, 0.9898214418809326842, 1.000000000000000000, 0.9898214418809326842, 1.000000000000000000, 0.9898214418809326842, 1.000000000000000000, 0.9898214418809326842, 1.000000000000000000, 0.9898214418809326842, 1.000000000000000000, 0.9898214418809326842, 1.000000000000000000, 0.9898214418809326842, 1.000000000000000000, 0.9898214418809326842, 1.000000000000000000, 0.9898214418809326842, 1.000000000000000000, 0.9898214418809326842, 1.000000000000000000, 0.9898214418809326842, 1.000000000000000000, 0.9898214418809326842, 1.000000000000000000, 0.9898214418809326842, 1.000000000000000000, 0.9898214418809326842, 1.000000000000000000, 0.9898214418809326842, 1.000000000000000000, 0.9898214418809326842, 1.000000000000000000, 0.9898214418809326842, 1.000000000000000000, 0.9898214418809326842, 1.000000000000000000, 0.9898214418809326842, 1.000000000000000000, 0.9898214418809326842, 1.000000000000000000, 0.9898214418809326842, 1.000000000000000000, 0.9898214418809326842, 1.000000000000000000, 0.9898214418809326842, 1.000000000000000000, 0.9898214418809326842, 1.000000000000000000, 0.9898214418809326842, 1.000000000000000000, 0.9898214418809326842, 1.000000000000000000, 0.9898214418809326842, 1.000000000000000000, 0.9898214418809326842, 1.000000000000000000, 0.9898214418809326842, 1.000000000000000000, 0.9898214418809326842, 1.000000000000000000, 0.9898214418809326842, 1.000000000000000000, 0.9898214418809326842, 1.000000000000000000, 0.9898214418809326842, 1.000000000000000000, 0.9898214418809326842, 1.000000000000000000, 0.9898214418809326842, 1.000000000000000000, 0.9898214418809326842, 1.000000000000000000, 0.9898214418809326842, 1.000000000000000000, 0.9898214418809326842, 1.000000000000000000, 0.9898214418809326842, 1.000000000000000000, 0.9898214418809326842, 1.000000000000000000, 0.9898214418809326842, 1.000000000000000000, 0.9898214418809326842, 1.000000000000000000, 0.9898214418809326842, 1.000000000000000000, 0.9898214418809326842, 1.000000000000000000, 0.9898214418809326842, 1.000000000000000000, 0.9898214418809326842, 1.000000000000000000, 0.9898214418809326842, 1.000000000000000000, 0.9898214418809326842, 1.000000000000000000, 0.9898214418809326842, 1.000000000000000000, 0.9898214418809326842, 1.000000000000000000, 0.9898214418809326842, 1.000000000000000000, 0.9898214418809326842, 1.000000000000000000, 0.9898214418809326842, 1.000000000000000000, 0.9898214418809326842, 1.000000000000000000, 0.9898214418809326842, 1.000000000000000000, 0.9898214418809326842, 1.000000000000000000, 0.9898214418809326842, 1.000000000000000000, 0.9898214418809326842, 1.000000000000000000, 0.9898214418809326842, 1.000000000000000000, 0.9898214418809326842, 1.000000000000000000, 0.9898214418809326842, 1.000000000000000000, 0.9898214418809326842, 1.000000000000000000, 0.9898214418809326842, 1.000000000000000000, 0.9898214418809326842, 1.000000000000000000, 0.9898214418809326842, 1.000000000000000000, 0.9898214418809326842, 1.000000000000000000, 0.9898214418809326842, 1.000000000000000000, 0.9898214418809326842, 1.000000000000000000, 0.9898214418809326842, 1.000000000000000000, 0.9898214418809326842, 1.000000000000000000, 0.9898214418809326842, 1.000000000000000000, 0.9898214418809326842, 1.000000000000000000, 0.9898214418809326842, 1.000000000000000000, 0.9898214418809326842, 1.000000000000000000, 0.9898214418809326842, 1.000000000000000000, 0.9898214418809326842, 1.000000000000000000, 0.9898214418809326842, 1.000000000000000000, 0.9898214418809326842, 1.000000000000000000, 0.9898214418809326842, 1.000000000000000000, 0.9898214418809326842, 1.000000000000000000, 0.9898214418809326842, 1.000000000000000000, 0.9898214418809326842, 1.000000000000000000, 0.9898214418809326842, 1.000000000000000000, 0.9898214418809326842, 1.000000000000000000, 0.9898214418809326842, 1.000000000000000000, 0.9898214418809326842, 1.000000000000000000, 0.9898214418809326842, 1.000000000000000000, 0.9898214418809326842, 1.000000000000000000, 0.9898214418809326842, 1.000000000000000000, 0.9898214418809326842, 1.000000000000000000, 0.9898214418809326842, 1.000000000000000000, 0.9898214418809326842, 1.000000000000000000, 0.9898214418809326842, 1.000000000000000000, 0.9898214418809326842, 1.000000000000000000, 0.9898214418809326842, 1.000000000000000000, 0.9898214418809326842, 1.000000000000000000, 0.9898214418809326842, 1.000000000000000000, 0.9898214418809326842, 1.000000000000000000, 0.9898214418809326842, 1.000000000000000000, 0.9898214418809326842, 1.000000000000000000, 0.9898214418809326842, 1.000000000000000000, 0.9898214418809326842, 1.000000000000000000, 0.9898214418809326842, 1.000000000000000000, 0.9898214418809326842, 1.000000000000000000, 0.9898214418809326842, 1.000000000000000000, 0.9898214418809326842, 1.000000000000000000, 0.9898214418809326842, 1.000000000000000000, 0.9898214418809326842, 1.000000000000000000, 0.9898214418809326842, 1.000000000000000000, 0.9898214418809326842, 1.000000000000000000, 0.9898214418809326842, 1.000000000000000000, 0.9898214418809326842, 1.000000000000000000, 0.9898214418809326842, 1.000000000000000000, 0.9898214418809326842, 1.000000000000000000, 0.9898214418809326842, 1.000000000000000000, 0.9898214418809326842, 1.000000000000000000, 0.9898214418809326842, 1.000000000000000000, 0.9898214418809326842, 1.000000000000000000, 0.9898214418809326842, 1.000000000000000000, 0.9898214418809326842, 1.000000000000000000, 0.9898214418809326842, 1.000000000000000000, 0.9898214418809326842, 1.000000000000000000, 0.9898214418809326842, 1.000000000000000000, 0.9898214418809326842, 1.000000000000000000, 0.9898214418809326842, 1.000000000000000000, 0.9898214418809326842, 1.000000000000000000, 0.9898214418809326842, 1.000000000000000000, 0.9898214418809326842, 1.000000000000000000, 0.9898214418809326842, 1.000000000000000000, 0.9898214418809326842, 1.000000000000000000, 0.9898214418809326842, 1.000000000000000000, 0.9898214418809326842, 1.000000000000000000, 0.9898214418809326842, 1.000000000000000000, 0.9898214418809326842, 1.000000000000000000, 0.9898214418809326842, 1.000000000000000000, 0.9898214418809326842, 1.000000000000000000, 0.9898214418809326842, 1.000000000000000000, 0.9898214418809326842, 1.000000000000000000, 0.9898214418809326842, 1.000000000000000000, 0.9898214418809326842, 1.000000000000000000, 0.9898214418809326842, 1.000000000000000000, 0.9898214418809326842, 1.000000000000000000, 0.9898214418809326842, 1.000000000000000000, 0.9898214418809326842, 1.000000000000000000, 0.9898214418809326842, 1.000000000000000000, 0.9898214418809326842, 1.000000000000000000, 0.9898214418809326842, 1.000000000000000000, 0.9898214418809326842, 1.000000000000000000, 0.9898214418809326842, 1.000000000000000000, 0.9898214418809326842, 1.000000000000000000, 0.9898214418809326842, 1.000000000000000000, 0.9898214418809326842, 1.000000000000000000, 0.9898214418809326842, 1.000000000000000000, 0.9898214418809326842, 1.000000000000000000, 0.9898214418809326842, 1.000000000000000000, 0.9898214418809326842, 1.000000000000000000, 0.9898214418809326842, 1.000000000000000000, 0.9898214418809326842, 1.000000000000000000, 0.9898214418809326842, 1.000000000000000000, 0.9898214418809326842, 1.000000000000000000, 0.9898214418809326842, 1.000000000000000000, 0.9898214418809326842, 1.000000000000000000, 0.9898214418809326842, 1.000000000000000000, 0.9898214418809326842, 1.000000000000000000, 0.9898214418809326842, 1.000000000000000000, 0.9898214418809326842, 1.000000000000000000, 0.9898214418809326842, 1.000000000000000000, 0.9898214418809326842, 1.000000000000000000, 0.9898214418809326842, 1.000000000000000000, 0.9898214418809326842, 1.000000000000000000, 0.9898214418809326842, 1.000000000000000000, 0.9898214418809326842, 1.000000000000000000, 0.9898214418809326842, 1.000000000000000000, 0.9898214418809326842, 1.000000000000000000, 0.9898214418809326842, 1.000000000000000000, 0.9898214418809326842, 1.000000000000000000, 0.9898214418809326842, 1.000000000000000000, 0.9898214418809326842, 1.000000000000000000, 0.9898214418809326842, 1.000000000000000000, 0.9898214418809326842, 1.000000000000000000, 0.9898214418809326842, 1.000000000000000000, 0.9898214418809326842, 1.000000000000000000, 0.9898214418809326842, 1.000000000000000000, 0.9898214418809326842, 1.000000000000000000, 0.9898214418809326842, 1.000000000000000000, 0.9898214418809326842, 1.000000000000000000, 0.9898214418809326842, 1.000000000000000000, 0.9898214418809326842, 1.000000000000000000, 0.9898214418809326842, 1.000000000000000000, 0.9898214418809326842, 1.000000000000000000, 0.9898214418809326842, 1.000000000000000000, 0.9898214418809326842, 1.000000000000000000, 0.9898214418809326842, 1.000000000000000000, 0.9898214418809326842, 1.000000000000000000, 0.9898214418809326842, 1.000000000000000000, 0.9898214418809326842, 1.000000000000000000, 0.9898214418809326842, 1.000000000000000000, 0.9961809353924466759, 0.9952277490961531914 ) ) 
 REPRESENTATION_ITEM ( '' )  );
#45071 = CARTESIAN_POINT ( 'NONE',  ( 815.2698199232962679, -256.8164208402379245, 342.5225473063383674 ) ) ;
#45072 = CARTESIAN_POINT ( 'NONE',  ( 804.1105419155481968, -339.8272453906069472, 347.6308680596136469 ) ) ;
#45073 = CARTESIAN_POINT ( 'NONE',  ( 757.2208543904082489, -424.7146871989589840, 350.9844846989624330 ) ) ;
#45074 = CARTESIAN_POINT ( 'NONE',  ( 787.5531968255692163, -165.8272453906074873, -316.1348686366205811 ) ) ;
#45075 = CARTESIAN_POINT ( 'NONE',  ( 768.0187753319979720, -128.6346026584201354, -318.0580252608186242 ) ) ;
#45076 = CARTESIAN_POINT ( 'NONE',  ( 804.6798772138710092, -327.7255117493285752, -334.6312213355106451 ) ) ;
#45077 = VERTEX_POINT ( 'NONE', #4986 ) ;
#45078 = CARTESIAN_POINT ( 'NONE',  ( 798.7617431975189675, -291.6237781080503169, 323.0428371773161871 ) ) ;
#45079 = CARTESIAN_POINT ( 'NONE',  ( 799.9999999999993179, -462.9681489794448339, 370.0000000000000568 ) ) ;
#45080 = DIRECTION ( 'NONE',  ( -0.000000000000000000, 1.000000000000000000, -0.000000000000000000 ) ) ;
#45081 = CARTESIAN_POINT ( 'NONE',  ( 755.8894580844503253, -135.8272453906076009, 332.3691319403863531 ) ) ;
#45082 = CARTESIAN_POINT ( 'NONE',  ( 756.3353852180819104, -29.90732993114771787, 331.1735550268788302 ) ) ;
#45083 = ORIENTED_EDGE ( 'NONE', *, *, #11477, .T. ) ;
#45084 = CARTESIAN_POINT ( 'NONE',  ( 755.8990559732751535, -347.4636090269705733, -365.9055244015606831 ) ) ;
#45085 = CARTESIAN_POINT ( 'NONE',  ( 814.2805881961230625, -241.6454272087890729, 331.2368401574024119 ) ) ;
#45086 = CARTESIAN_POINT ( 'NONE',  ( 795.1360043628807261, -332.0891481129649492, -360.2193346964456282 ) ) ;
#45087 = ADVANCED_FACE ( 'NONE', ( #16513 ), #19079, .T. ) ;
#45088 = FACE_OUTER_BOUND ( 'NONE', #8182, .T. ) ;
#45089 = CARTESIAN_POINT ( 'NONE',  ( 769.0155153010367712, -178.3726999360619629, -362.7791456095907279 ) ) ;
#45090 = CARTESIAN_POINT ( 'NONE',  ( 814.5518280994195948, -63.72551174932939233, 332.4837098697145734 ) ) ;
#45091 = CARTESIAN_POINT ( 'NONE',  ( 772.4999999999993179, -462.9681489794447771, 310.9526249034443026 ) ) ;
#45092 = CARTESIAN_POINT ( 'NONE',  ( 745.7998596910086917, -389.3618753856919739, -332.5602148656461168 ) ) ;
#45093 = CYLINDRICAL_SURFACE ( 'NONE', #16574, 10.00000000000000888 ) ;
#45094 = CARTESIAN_POINT ( 'NONE',  ( 814.8207195650702488, -314.1908817542433781, 336.2433038121456548 ) ) ;
#45095 = CARTESIAN_POINT ( 'NONE',  ( 794.9999999999993179, 205.0000000000000568, -265.0000000000000000 ) ) ;
#45096 = CARTESIAN_POINT ( 'NONE',  ( 800.9747183278959710, -300.9982390220559409, 311.9810565676471583 ) ) ;
#45097 = CARTESIAN_POINT ( 'NONE',  ( 746.8695393053150156, -5.907329931147798696, -327.6429770376306010 ) ) ;
#45098 = EDGE_CURVE ( 'NONE', #44320, #36156, #36632, .T. ) ;
#45099 = CARTESIAN_POINT ( 'NONE',  ( 803.4237431249931660, -255.1800572038742700, -331.2633955100225194 ) ) ;
#45100 = CARTESIAN_POINT ( 'NONE',  ( 799.9999999999993179, -365.3551492539851893, 18.13243251470705886 ) ) ;
#45101 = CARTESIAN_POINT ( 'NONE',  ( 804.9363028652555840, -400.2709662947828519, 338.2165204200192079 ) ) ;
#45102 = CARTESIAN_POINT ( 'NONE',  ( 776.9254006560222479, -140.1908817542438896, 314.8983024940802125 ) ) ;
#45103 = CARTESIAN_POINT ( 'NONE',  ( 760.0363995740630116, -34.91815448151697154, -368.7758568127991907 ) ) ;
#45104 = CARTESIAN_POINT ( 'NONE',  ( 755.0488828828309806, -41.80559628986934229, -344.1219089521771934 ) ) ;
#45105 = CARTESIAN_POINT ( 'NONE',  ( 778.7502325331095108, -72.35105083532378956, 304.6391490659818828 ) ) ;
#45106 = CARTESIAN_POINT ( 'NONE',  ( 803.4237431249931660, -375.1800572038739574, 331.2633955100225194 ) ) ;
#45107 = CARTESIAN_POINT ( 'NONE',  ( 769.9999999999992042, 205.0000000000000568, -350.0000000000000000 ) ) ;
#45108 =( NAMED_UNIT ( * ) PLANE_ANGLE_UNIT ( ) SI_UNIT ( $, .RADIAN. ) );
#45109 = CARTESIAN_POINT ( 'NONE',  ( 758.0580252608178853, -438.4527844766009821, 328.0187753319985404 ) ) ;
#45110 = ORIENTED_EDGE ( 'NONE', *, *, #3007, .F. ) ;
#45111 = CARTESIAN_POINT ( 'NONE',  ( 762.3223304703356007, -79.54369356751119824, -322.3223304703362828 ) ) ;
#45112 = CARTESIAN_POINT ( 'NONE',  ( 766.7756240680305382, -350.5328690171411381, -361.5560724626415663 ) ) ;
#45114 = CARTESIAN_POINT ( 'NONE',  ( 758.0580252608178853, -174.4527844766018063, 328.0187753319985404 ) ) ;
#45113 = CARTESIAN_POINT ( 'NONE',  ( 768.0187753319979720, -200.6346026584199365, 318.0580252608186242 ) ) ;
#45115 = VERTEX_POINT ( 'NONE', #15601 ) ;
#45116 = CARTESIAN_POINT ( 'NONE',  ( 783.7566961878529810, -360.8965053807773984, -305.1792804349288417 ) ) ;
#45117 = DIRECTION ( 'NONE',  ( 8.326672684688676025E-16, -1.000000000000000000, 0.000000000000000000 ) ) ;
#45118 = ORIENTED_EDGE ( 'NONE', *, *, #1487, .T. ) ;
#45119 = CARTESIAN_POINT ( 'NONE',  ( 791.9812246680005501, -404.6346026584193396, 361.9419747391813189 ) ) ;
#45120 = ORIENTED_EDGE ( 'NONE', *, *, #30109, .F. ) ;
#45121 = CARTESIAN_POINT ( 'NONE',  ( 805.0032342141412300, -229.5436935675106440, -314.9967657858571783 ) ) ;
#45122 = CARTESIAN_POINT ( 'NONE',  ( 800.9747183278959710, -108.9982390220565804, 311.9810565676471583 ) ) ;
#45123 = ORIENTED_EDGE ( 'NONE', *, *, #22178, .T. ) ;
#45124 = CARTESIAN_POINT ( 'NONE',  ( 804.6798772138710092, -207.7255117493289731, -334.6312213355106451 ) ) ;
#45125 = ORIENTED_EDGE ( 'NONE', *, *, #25197, .T. ) ;
#45126 = CARTESIAN_POINT ( 'NONE',  ( 781.8018195045266339, -310.2709662947832499, -365.1927285166406705 ) ) ;
#45127 = CARTESIAN_POINT ( 'NONE',  ( 801.9419747391806368, -18.45278447660230725, -351.9812246680014027 ) ) ;
#45128 = CARTESIAN_POINT ( 'NONE',  ( 773.3843516231979720, -205.4419599262324425, 364.4086373105754433 ) ) ;
#45129 = CARTESIAN_POINT ( 'NONE',  ( 791.7608162188021197, 205.0000000000000568, 339.9999999999999432 ) ) ;
#45130 = DIRECTION ( 'NONE',  ( 1.000000000000000000, 0.000000000000000000, 0.000000000000000000 ) ) ;
#45131 = VERTEX_POINT ( 'NONE', #43545 ) ;
#45132 = CARTESIAN_POINT ( 'NONE',  ( 771.1735550268778070, 14.81994279612486309, -316.3353852180827630 ) ) ;
#45133 = FACE_OUTER_BOUND ( 'NONE', #23554, .T. ) ;
#45134 = PLANE ( 'NONE',  #44734 ) ;
#45135 = CARTESIAN_POINT ( 'NONE',  ( 807.2620300519052989, -240.0090635724253900, -318.0141637701419768 ) ) ;
#45136 = CARTESIAN_POINT ( 'NONE',  ( 805.6418435158337843, -125.4636090269712412, 363.8556311672236916 ) ) ;
#45138 = CARTESIAN_POINT ( 'NONE',  ( 803.4237431249931660, -231.1800572038743553, -331.2633955100225194 ) ) ;
#45137 = DIRECTION ( 'NONE',  ( -1.000000000000000000, 0.000000000000000000, 0.000000000000000000 ) ) ;
#45139 = CARTESIAN_POINT ( 'NONE',  ( 805.0264073115434940, -414.3510508353227237, -339.4763451958999099 ) ) ;
#45140 = VECTOR ( 'NONE', #9417, 1000.000000000000000 ) ;
#45141 = CARTESIAN_POINT ( 'NONE',  ( 809.9999999999993179, -512.9681489794448908, -339.9999999999999432 ) ) ;
#45142 = CARTESIAN_POINT ( 'NONE',  ( 794.9819416627830151, 11.00176097794305541, -319.9864689768909898 ) ) ;
#45143 = CARTESIAN_POINT ( 'NONE',  ( 763.0428371773158460, -83.46360902697136908, -358.7617431975195359 ) ) ;
#45144 = CARTESIAN_POINT ( 'NONE',  ( 787.5531968255692163, -429.8272453906067199, 316.1348686366205811 ) ) ;
#45145 = PLANE ( 'NONE',  #1806 ) ;
#45146 = CARTESIAN_POINT ( 'NONE',  ( 812.6845335610512393, 16.01258552831230375, -353.5525998758768651 ) ) ;
#45147 = CARTESIAN_POINT ( 'NONE',  ( 745.0891759886404770, -292.2709662947831930, -342.4968714119734159 ) ) ;
#45148 =( LENGTH_UNIT ( ) NAMED_UNIT ( * ) SI_UNIT ( .MILLI., .METRE. ) );
#45149 = CARTESIAN_POINT ( 'NONE',  ( 797.8594530101008786, 10.45630643248850866, 322.1405469898980982 ) ) ;
#45150 = CARTESIAN_POINT ( 'NONE',  ( 755.0636971347428243, -76.27096629478394618, -341.7834795799807353 ) ) ;
#45151 = CARTESIAN_POINT ( 'NONE',  ( 783.7953271457878373, -200.1908817542436907, 375.1787889125761239 ) ) ;
#45152 = CARTESIAN_POINT ( 'NONE',  ( 813.2346286133761168, -173.2601417444143692, -328.9521613784389160 ) ) ;
#45153 = CARTESIAN_POINT ( 'NONE',  ( 747.2067596250078623, -195.1800572038744974, 352.2312462859687230 ) ) ;
#45154 = CARTESIAN_POINT ( 'NONE',  ( 810.7187646348534145, -426.4527844766010389, -356.7737145352016341 ) ) ;
#45155 = DIRECTION ( 'NONE',  ( 0.000000000000000000, -1.000000000000000000, 1.056348263647623421E-15 ) ) ;
#45156 = CARTESIAN_POINT ( 'NONE',  ( 797.8594530101008786, -277.5436935675105019, 322.1405469898980982 ) ) ;
#45157 = CARTESIAN_POINT ( 'NONE',  ( 802.9823548866075953, -73.09997266333502353, 330.0799878456151077 ) ) ;
#45158 = CARTESIAN_POINT ( 'NONE',  ( 774.6858677611749044, -441.7255117493282910, -315.5713283507209894 ) ) ;
#45159 = CARTESIAN_POINT ( 'NONE',  ( 799.9999999999993179, -512.9681489794448908, -339.9999999999999432 ) ) ;
#45160 = FACE_OUTER_BOUND ( 'NONE', #32980, .T. ) ;
#45162 = CARTESIAN_POINT ( 'NONE',  ( 759.7806653035534055, -342.9982390220557136, 324.8639956371180801 ) ) ;
#45161 = CARTESIAN_POINT ( 'NONE',  ( 804.9511171171677688, -125.8055962898690581, 335.8780910478229202 ) ) ;
#45163 = ORIENTED_EDGE ( 'NONE', *, *, #1735, .T. ) ;
#45164 = CARTESIAN_POINT ( 'NONE',  ( 759.2295555964440155, -256.1692326535049915, -353.9708237608231229 ) ) ;
#45165 = CARTESIAN_POINT ( 'NONE',  ( 781.7834795799800531, -106.8164208402383935, 315.0636971347436202 ) ) ;
#45166 = VECTOR ( 'NONE', #30823, 1000.000000000000000 ) ;
#45167 = VECTOR ( 'NONE', #24621, 1000.000000000000000 ) ;
#45168 = CARTESIAN_POINT ( 'NONE',  ( 814.8230680027162407, -245.8055962898686460, -333.7305795820267917 ) ) ;
#45169 = CARTESIAN_POINT ( 'NONE',  ( 773.4999999999993179, -110.5936016518799221, 750.6326042729449455 ) ) ;
#45170 = CARTESIAN_POINT ( 'NONE',  ( 811.6461892240364477, -364.7146871989592114, 324.1737431748509835 ) ) ;
#45171 = ORIENTED_EDGE ( 'NONE', *, *, #24906, .F. ) ;
#45172 = CARTESIAN_POINT ( 'NONE',  ( 781.7834795799800531, -274.8164208402378108, 315.0636971347436202 ) ) ;
#45173 = CARTESIAN_POINT ( 'NONE',  ( 800.0135310231082713, -158.0891481129655176, -325.0180583372163028 ) ) ;
#45174 = CARTESIAN_POINT ( 'NONE',  ( 792.1044303154645831, -396.4527844766010389, 317.8323909638837677 ) ) ;
#45175 = CARTESIAN_POINT ( 'NONE',  ( 792.3570229623688874, -117.1800572038746964, -373.1304606946836202 ) ) ;
#45176 = CARTESIAN_POINT ( 'NONE',  ( 771.2633955100217236, -95.90732993114751537, -363.4237431249939618 ) ) ;
#45177 = ORIENTED_EDGE ( 'NONE', *, *, #1955, .F. ) ;
#45178 = CARTESIAN_POINT ( 'NONE',  ( 757.0176451133909268, -61.09997266333506616, -349.9200121543848354 ) ) ;
#45179 = CARTESIAN_POINT ( 'NONE',  ( 769.0155153010367712, -346.3726999360614514, -362.7791456095907279 ) ) ;
#45180 = CARTESIAN_POINT ( 'NONE',  ( 805.1927285166397041, -112.8164208402383508, 341.8018195045277707 ) ) ;
#45181 = CARTESIAN_POINT ( 'NONE',  ( 758.6633372737375112, -92.53286901714190549, 326.9102291470432533 ) ) ;
#45184 = CARTESIAN_POINT ( 'NONE',  ( 805.9055244015594326, -339.6237781080502600, 315.8990559732753240 ) ) ;
#45183 = DIRECTION ( 'NONE',  ( 1.000000000000000000, 0.000000000000000000, -0.000000000000000000 ) ) ;
#45182 = DIRECTION ( 'NONE',  ( -1.084653538143406060E-16, 0.6594541114781790059, -0.7517448203044204691 ) ) ;
#45185 = CARTESIAN_POINT ( 'NONE',  ( 747.3154664389472828, -115.9874144716872877, 326.4474001241230781 ) ) ;
#45186 = CARTESIAN_POINT ( 'NONE',  ( 760.7433823573367135, -372.0090635724250205, -355.9930595647440441 ) ) ;
#45187 = CARTESIAN_POINT ( 'NONE',  ( 785.3141322388236176, -357.7255117493285184, -364.4286716492789537 ) ) ;
#45188 = CIRCLE ( 'NONE', #25261, 30.00000000000008171 ) ;
#45189 = CARTESIAN_POINT ( 'NONE',  ( 814.4686193811664907, -123.2817908451530542, -346.2056067578752732 ) ) ;
#45190 = CARTESIAN_POINT ( 'NONE',  ( 814.4686193811664907, -3.281790845153435221, 346.2056067578752732 ) ) ;
#45192 = CARTESIAN_POINT ( 'NONE',  ( 786.4999999999993179, -544.8427095258973623, -369.9999999999999432 ) ) ;
#45191 = DIRECTION ( 'NONE',  ( 1.000000000000000000, 0.000000000000000000, 0.000000000000000000 ) ) ;
#45193 = CARTESIAN_POINT ( 'NONE',  ( 755.0488828828309806, -281.8055962898686175, -344.1219089521771934 ) ) ;
#45194 = CARTESIAN_POINT ( 'NONE',  ( 809.0717654672305343, -148.9181544815166092, -360.1688906516309885 ) ) ;
#45195 = CARTESIAN_POINT ( 'NONE',  ( 831.1634899080286232, 259.9999999999998863, -199.9999999999999432 ) ) ;
#45196 = DIRECTION ( 'NONE',  ( -1.000000000000000000, -0.000000000000000000, -0.000000000000000000 ) ) ;
#45197 = CARTESIAN_POINT ( 'NONE',  ( 802.5472867521000353, -340.3726999360615082, 350.8726784830461156 ) ) ;
#45198 = CARTESIAN_POINT ( 'NONE',  ( 776.2046728542105711, -308.1908817542434349, 304.8212110874238761 ) ) ;
#45199 = CARTESIAN_POINT ( 'NONE',  ( 763.2262854647970016, -176.6346026584199933, -309.2812353651462445 ) ) ;
#45200 = CARTESIAN_POINT ( 'NONE',  ( -208.8365100919714052, 240.0000000000001137, -199.9999999999926956 ) ) ;
#45201 = CARTESIAN_POINT ( 'NONE',  ( 807.2620300519052989, -96.00906357242585898, 318.0141637701419768 ) ) ;
#45202 = CARTESIAN_POINT ( 'NONE',  ( 763.2262854647970016, -320.6346026584195670, -309.2812353651462445 ) ) ;
#45203 = DIRECTION ( 'NONE',  ( 0.000000000000000000, 0.000000000000000000, 1.000000000000000000 ) ) ;
#45204 = DIRECTION ( 'NONE',  ( 0.000000000000000000, 0.000000000000000000, 1.000000000000000000 ) ) ;
#45205 = CARTESIAN_POINT ( 'NONE',  ( 758.0580252608178853, -198.4527844766017495, 328.0187753319985404 ) ) ;
#45206 = ORIENTED_EDGE ( 'NONE', *, *, #114, .T. ) ;
#45207 = CARTESIAN_POINT ( 'NONE',  ( 813.5763878283155464, -411.8272453906067199, 351.1614460488615350 ) ) ;
#45208 = CARTESIAN_POINT ( 'NONE',  ( 783.7566961878529810, -360.8965053807773984, -305.1792804349288417 ) ) ;
#45209 = CARTESIAN_POINT ( 'NONE',  ( 812.7932403749906598, -135.1800572038746679, -327.7687537140311633 ) ) ;
#45210 = CARTESIAN_POINT ( 'NONE',  ( 754.7162404726377645, -62.73633629969871350, 339.4709603349214717 ) ) ;
#45211 = CARTESIAN_POINT ( 'NONE',  ( 811.0346526505616112, -398.6346026584193396, -323.0537975583477532 ) ) ;
#45212 = DIRECTION ( 'NONE',  ( 1.644774851296528363E-16, -1.000000000000000000, 0.000000000000000000 ) ) ;
#45213 = CARTESIAN_POINT ( 'NONE',  ( 775.9200461376533440, -431.8055962898681059, 315.3028492785443291 ) ) ;
#45214 = EDGE_LOOP ( 'NONE', ( #42571, #33142, #36872, #38525 ) ) ;
#45215 = AXIS2_PLACEMENT_3D ( 'NONE', #4981, #22516, #21850 ) ;
#45216 = CARTESIAN_POINT ( 'NONE',  ( 747.3154664389472828, -139.9874144716872024, -326.4474001241230781 ) ) ;
#45217 =( NAMED_UNIT ( * ) SI_UNIT ( $, .STERADIAN. ) SOLID_ANGLE_UNIT ( ) );
#45218 = CARTESIAN_POINT ( 'NONE',  ( 749.8865473780648472, -260.5328690171413086, 322.1177392798429082 ) ) ;
#45219 = CARTESIAN_POINT ( 'NONE',  ( 758.0580252608178853, -126.4527844766019626, 328.0187753319985404 ) ) ;
#45220 = PRODUCT_DEFINITION_FORMATION_WITH_SPECIFIED_SOURCE ( 'ANY', '', #26963, .NOT_KNOWN. ) ;
#45221 = ORIENTED_EDGE ( 'NONE', *, *, #16211, .T. ) ;
#45222 = CARTESIAN_POINT ( 'NONE',  ( 764.8639956371174549, -272.0891481129651197, 319.7806653035542013 ) ) ;
#45223 = CARTESIAN_POINT ( 'NONE',  ( 814.9108240113580450, 7.729033705215793582, -337.5031285880265273 ) ) ;
#45224 = DIRECTION ( 'NONE',  ( -1.000000000000000000, -0.000000000000000000, 0.000000000000000000 ) ) ;
#45225 = ORIENTED_EDGE ( 'NONE', *, *, #715, .F. ) ;
#45226 = ORIENTED_EDGE ( 'NONE', *, *, #27795, .F. ) ;
#45227 = CARTESIAN_POINT ( 'NONE',  ( 801.9419747391806368, -186.4527844766017779, -351.9812246680014027 ) ) ;
#45228 = CARTESIAN_POINT ( 'NONE',  ( 749.5768839229115201, -420.5545181178793541, -358.0661480581553064 ) ) ;
#45229 = CARTESIAN_POINT ( 'NONE',  ( 758.0580252608178853, -30.45278447660226817, 328.0187753319985404 ) ) ;
#45230 = CARTESIAN_POINT ( 'NONE',  ( 754.8072714833581358, -244.8164208402378961, -338.1981804954720587 ) ) ;
#45232 = CARTESIAN_POINT ( 'NONE',  ( 795.6651683502461765, -250.7146871989595809, 371.3240766477733814 ) ) ;
#45231 = CARTESIAN_POINT ( 'NONE',  ( 811.0346526505617248, -374.6346026584193396, 323.0537975583478101 ) ) ;
#45233 = EDGE_CURVE ( 'NONE', #22309, #34504, #2191, .T. ) ;
#45234 = CARTESIAN_POINT ( 'NONE',  ( 761.4292242960306112, -257.4636090269708575, -323.2154366446414429 ) ) ;
#45235 = CARTESIAN_POINT ( 'NONE',  ( 759.9864689768902508, -266.0891481129651197, -354.9819416627836404 ) ) ;
#45236 = CARTESIAN_POINT ( 'NONE',  ( 767.8955696845334842, -408.4527844766009821, -362.1676090361161755 ) ) ;
#45237 = CARTESIAN_POINT ( 'NONE',  ( 757.8323909638827445, -74.63460265842032015, -352.1044303154654358 ) ) ;
#45238 = CARTESIAN_POINT ( 'NONE',  ( 781.7834795799800531, -250.8164208402379245, 315.0636971347436202 ) ) ;
#45239 = VERTEX_POINT ( 'NONE', #26223 ) ;
#45240 = CARTESIAN_POINT ( 'NONE',  ( 767.7687537140311633, -359.9073299311467053, 372.7932403749916830 ) ) ;
#45241 = DIRECTION ( 'NONE',  ( 1.892425610156518354E-16, 1.000000000000000000, -0.000000000000000000 ) ) ;
#45242 = CARTESIAN_POINT ( 'NONE',  ( 813.5763878283155464, -51.82724539060782121, -351.1614460488615350 ) ) ;
#45243 = DIRECTION ( 'NONE',  ( 0.000000000000000000, 0.000000000000000000, 1.000000000000000000 ) ) ;
#45244 = CARTESIAN_POINT ( 'NONE',  ( -598.8365100919716042, 258.0940000000001646, -193.8809999999899674 ) ) ;
#45245 = EDGE_CURVE ( 'NONE', #24787, #296, #11911, .T. ) ;
#45246 = CARTESIAN_POINT ( 'NONE',  ( 776.9254006560222479, -212.1908817542436623, 314.8983024940802125 ) ) ;
#45247 = CARTESIAN_POINT ( 'NONE',  ( 759.7806653035534055, -102.9982390220565520, 324.8639956371180801 ) ) ;
#45248 = ORIENTED_EDGE ( 'NONE', *, *, #44060, .T. ) ;
#45249 = CARTESIAN_POINT ( 'NONE',  ( 757.0176451133909268, -13.09997266333522248, -349.9200121543848354 ) ) ;
#45250 = VECTOR ( 'NONE', #29735, 1000.000000000000000 ) ;
#45251 = CARTESIAN_POINT ( 'NONE',  ( 811.0346526505617248, -86.63460265842024910, -323.0537975583478101 ) ) ;
#45252 = CARTESIAN_POINT ( 'NONE',  ( 754.8983024940795303, -282.8965053807776258, 336.9254006560228163 ) ) ;
#45253 = CARTESIAN_POINT ( 'NONE',  ( 781.7834795799800531, -418.8164208402374129, -315.0636971347436202 ) ) ;
#45254 = CARTESIAN_POINT ( 'NONE',  ( 795.1360043628808398, -44.08914811296585157, -360.2193346964456282 ) ) ;
#45255 = CARTESIAN_POINT ( 'NONE',  ( 768.9521613784389729, -9.827245390607961539, 373.2346286133773106 ) ) ;
#45256 = CARTESIAN_POINT ( 'NONE',  ( 754.9967657858570647, -193.5436935675108714, -365.0032342141425374 ) ) ;
#45257 = CARTESIAN_POINT ( 'NONE',  ( 763.2262854647970016, -176.6346026584199933, 309.2812353651462445 ) ) ;
#45258 = CARTESIAN_POINT ( 'NONE',  ( 756.5762568750052424, -75.18005720387485269, 348.7366044899774238 ) ) ;
#45259 = DIRECTION ( 'NONE',  ( 1.000000000000000000, -0.000000000000000000, 0.000000000000000000 ) ) ;
#45260 = CARTESIAN_POINT ( 'NONE',  ( 571.1634899080285095, 239.9999999999999432, -197.2499999999982947 ) ) ;
#45261 = CARTESIAN_POINT ( 'NONE',  ( 788.7631598425961101, -265.4419599262323004, -305.7194118038759143 ) ) ;
#45262 = VECTOR ( 'NONE', #6372, 1000.000000000000000 ) ;
#45263 = CARTESIAN_POINT ( 'NONE',  ( 812.3518521366052028, -433.0999726633339151, 326.5853460496235243 ) ) ;
#45264 = EDGE_CURVE ( 'NONE', #44204, #31386, #15054, .T. ) ;
#45265 = CARTESIAN_POINT ( 'NONE',  ( 787.4397851343537695, -285.7255117493286889, -374.2001403089903988 ) ) ;
#45266 = FACE_OUTER_BOUND ( 'NONE', #15363, .T. ) ;
#45267 = CARTESIAN_POINT ( 'NONE',  ( 755.2512626584698410, -391.5436935675101608, 315.2512626584710915 ) ) ;
#45268 = CARTESIAN_POINT ( 'NONE',  ( 787.5162901302840055, -11.36187538569323863, 305.4481719005793252 ) ) ;
#45269 = CARTESIAN_POINT ( 'NONE',  ( 803.4237431249931660, -399.1800572038738437, -331.2633955100225194 ) ) ;
#45270 = CARTESIAN_POINT ( 'NONE',  ( 766.7756240680305382, -14.53286901714214707, 361.5560724626415663 ) ) ;
#45271 = EDGE_CURVE ( 'NONE', #38059, #24078, #33374, .T. ) ;
#45272 = CARTESIAN_POINT ( 'NONE',  ( 776.2433038121456548, -60.89650538077837894, -374.8207195650711014 ) ) ;
#45273 = CARTESIAN_POINT ( 'NONE',  ( 801.3366627262608972, -152.5328690171416781, -353.0897708529566899 ) ) ;
#45274 = CARTESIAN_POINT ( 'NONE',  ( 744.9990715423526808, -186.3510508353234343, 341.2370466360926002 ) ) ;
#45275 = CARTESIAN_POINT ( 'NONE',  ( 774.6312213355098493, -23.36187538569319244, 364.6798772138717482 ) ) ;
#45276 = CARTESIAN_POINT ( 'NONE',  ( 813.9316612368132837, -175.4419599262325562, 348.6739635108323228 ) ) ;
#45277 = EDGE_LOOP ( 'NONE', ( #16714, #38573, #27, #39055 ) ) ;
#45278 = CARTESIAN_POINT ( 'NONE',  ( 792.1044303154645831, -60.45278447660215448, -317.8323909638837677 ) ) ;
#45279 = CARTESIAN_POINT ( 'NONE',  ( 770.0799878456142551, -181.9874144716870887, -362.9823548866085616 ) ) ;
#45280 = CARTESIAN_POINT ( 'NONE',  ( 785.3687786644884454, -179.3618753856927128, 315.3201227861279676 ) ) ;
#45281 = CARTESIAN_POINT ( 'NONE',  ( 766.5853460496234675, 10.01258552831232329, -372.3518521366060554 ) ) ;
#45282 = CARTESIAN_POINT ( 'NONE',  ( 804.6798772138710092, -303.7255117493286889, 334.6312213355106451 ) ) ;
#45283 = VECTOR ( 'NONE', #9360, 1000.000000000000000 ) ;
#45284 = DIRECTION ( 'NONE',  ( -1.000000000000000000, -0.000000000000000000, -0.000000000000000000 ) ) ;
#45285 = VECTOR ( 'NONE', #26892, 1000.000000000000000 ) ;
#45286 = ORIENTED_EDGE ( 'NONE', *, *, #4645, .F. ) ;
#45287 = CARTESIAN_POINT ( 'NONE',  ( 783.0433043558608688, -0.8965053807785533513, 315.1538015810313027 ) ) ;
#45288 = CARTESIAN_POINT ( 'NONE',  ( 811.3240766477731540, -292.3726999360616219, -355.6651683502462902 ) ) ;
#45289 = EDGE_CURVE ( 'NONE', #29488, #8383, #44000, .T. ) ;
#45290 = CARTESIAN_POINT ( 'NONE',  ( 745.4481719005789273, -243.7255117493288310, 347.5162901302853697 ) ) ;
#45291 = EDGE_CURVE ( 'NONE', #27172, #45689, #35678, .T. ) ;
#45292 = CARTESIAN_POINT ( 'NONE',  ( 755.3028492785439312, -327.2817908451525000, 335.9200461376539693 ) ) ;
#45293 = CARTESIAN_POINT ( 'NONE',  ( 790.8726784830453198, -418.7146871989590409, 362.5472867521010585 ) ) ;
#45294 = CARTESIAN_POINT ( 'NONE',  ( 755.3028492785439312, -159.2817908451529547, -335.9200461376539693 ) ) ;
#45295 = CARTESIAN_POINT ( 'NONE',  ( 785.3141322388236176, -165.7255117493291152, -364.4286716492789537 ) ) ;
#45296 = CARTESIAN_POINT ( 'NONE',  ( 781.7834795799800531, -298.8164208402377540, -315.0636971347436202 ) ) ;
#45297 = VERTEX_POINT ( 'NONE', #30142 ) ;
#45298 = AXIS2_PLACEMENT_3D ( 'NONE', #43986, #26211, #12363 ) ;
#45299 = CARTESIAN_POINT ( 'NONE',  ( 804.9511171171677688, -341.8055962898683333, 335.8780910478229202 ) ) ;
#45300 = DIRECTION ( 'NONE',  ( 0.000000000000000000, 0.000000000000000000, 1.000000000000000000 ) ) ;
#45301 = ADVANCED_FACE ( 'NONE', ( #8900 ), #22967, .F. ) ;
#45302 = CARTESIAN_POINT ( 'NONE',  ( 773.4516893846965786, -139.6454272087893571, 315.8398074228977066 ) ) ;
#45303 = ORIENTED_EDGE ( 'NONE', *, *, #13183, .F. ) ;
#45304 = CARTESIAN_POINT ( 'NONE',  ( 788.6739635108323228, -367.6454272087886466, -373.9316612368139090 ) ) ;
#45305 = CARTESIAN_POINT ( 'NONE',  ( 879.9999999999992042, 469.9999999999998863, -350.0000000000000000 ) ) ;
#45306 = CARTESIAN_POINT ( 'NONE',  ( 755.8990559732751535, -227.4636090269709143, 365.9055244015606831 ) ) ;
#45307 = CARTESIAN_POINT ( 'NONE',  ( 772.3691319403857278, -191.2601417444143976, 315.8894580844506663 ) ) ;
#45308 = CARTESIAN_POINT ( 'NONE',  ( 764.8639956371174549, -344.0891481129647786, -319.7806653035542013 ) ) ;
#45309 = DIRECTION ( 'NONE',  ( 0.000000000000000000, 0.000000000000000000, -1.000000000000000000 ) ) ;
#45310 = CARTESIAN_POINT ( 'NONE',  ( 796.1575198192839480, -222.0090635724254184, -359.4546378042384163 ) ) ;
#45311 = CARTESIAN_POINT ( 'NONE',  ( 777.4774526936600978, -82.27096629478388934, 304.7301800767027657 ) ) ;
#45312 = CARTESIAN_POINT ( 'NONE',  ( 790.0183182880230106, -452.9681489794449476, 362.9048749981275250 ) ) ;
#45313 = CARTESIAN_POINT ( 'NONE',  ( 782.4968714119720516, -418.8164208402374129, -305.0891759886411023 ) ) ;
#45314 = VECTOR ( 'NONE', #28204, 1000.000000000000000 ) ;
#45315 = CARTESIAN_POINT ( 'NONE',  ( 799.9999999999993179, -512.9681489794448908, -309.9999999999998863 ) ) ;
#45316 = EDGE_CURVE ( 'NONE', #44956, #4358, #40764, .T. ) ;
#45317 = CARTESIAN_POINT ( 'NONE',  ( 814.8207195650702488, -338.1908817542433212, 336.2433038121456548 ) ) ;
#45318 = EDGE_CURVE ( 'NONE', #19255, #1155, #37530, .T. ) ;
#45319 = DIRECTION ( 'NONE',  ( 1.000000000000000000, 0.000000000000000000, 0.000000000000000000 ) ) ;
#45320 = CARTESIAN_POINT ( 'NONE',  ( 745.7998596910086917, -293.3618753856923718, 332.5602148656461168 ) ) ;
#45321 = CARTESIAN_POINT ( 'NONE',  ( 772.5602148656447525, -57.72551174932945628, -305.7998596910095443 ) ) ;
#45322 = CARTESIAN_POINT ( 'NONE',  ( 785.3687786644884454, -275.3618753856923149, -315.3201227861279676 ) ) ;
#45323 = LINE ( 'NONE', #38867, #380 ) ;
#45324 = CARTESIAN_POINT ( 'NONE',  ( 785.3141322388236176, -381.7255117493284615, 364.4286716492789537 ) ) ;
#45325 = CARTESIAN_POINT ( 'NONE',  ( 804.6971507214547046, -147.2817908451529547, 344.0799538623459739 ) ) ;
#45326 = CARTESIAN_POINT ( 'NONE',  ( 750.9282345327678740, -16.91815448151702839, -319.8311093483690115 ) ) ;
#45327 = CARTESIAN_POINT ( 'NONE',  ( 759.2295555964440155, -64.16923265350563099, -353.9708237608231229 ) ) ;
#45328 = CARTESIAN_POINT ( 'NONE',  ( 815.0009284576459549, -78.35105083532376113, 338.7629533639073429 ) ) ;
#45329 = CARTESIAN_POINT ( 'NONE',  ( 803.6646147819162707, -377.9073299311465917, 348.8264449731211130 ) ) ;
#45330 = CARTESIAN_POINT ( 'NONE',  ( 782.4968714119720516, 13.18357915976123174, 305.0891759886411023 ) ) ;
#45331 = AXIS2_PLACEMENT_3D ( 'NONE', #470, #910, #42950 ) ;
#45332 = CARTESIAN_POINT ( 'NONE',  ( 804.6798772138708955, -423.7255117493281205, 334.6312213355107019 ) ) ;
#45333 = ORIENTED_EDGE ( 'NONE', *, *, #45098, .F. ) ;
#45334 = CARTESIAN_POINT ( 'NONE',  ( 794.9819416627830151, -60.99823902205671544, -319.9864689768909898 ) ) ;
#45335 = CIRCLE ( 'NONE', #1084, 2.749999999999863665 ) ;
#45336 = CARTESIAN_POINT ( 'NONE',  ( 770.0799878456142551, -349.9874144716865771, -362.9823548866085616 ) ) ;
#45338 = CARTESIAN_POINT ( 'NONE',  ( 797.8594530101009923, -205.5436935675108145, 322.1405469898982119 ) ) ;
#45337 = CARTESIAN_POINT ( 'NONE',  ( 795.1360043628807261, -236.0891481129651766, 360.2193346964456282 ) ) ;
#45339 = ORIENTED_EDGE ( 'NONE', *, *, #25811, .T. ) ;
#45340 = CARTESIAN_POINT ( 'NONE',  ( 746.7653713866222915, -401.2601417444137155, -351.0478386215610271 ) ) ;
#45342 = EDGE_CURVE ( 'NONE', #19960, #39647, #37152, .T. ) ;
#45341 = CARTESIAN_POINT ( 'NONE',  ( -769.9999999999992042, 205.0000000000000568, -350.0000000000000000 ) ) ;
#45343 = EDGE_LOOP ( 'NONE', ( #13207, #13493, #17791, #34488 ) ) ;
#45344 = CARTESIAN_POINT ( 'NONE',  ( 755.5713283507202505, -389.3618753856919739, 334.6858677611754729 ) ) ;
#45345 = ADVANCED_FACE ( 'NONE', ( #13055 ), #10485, .T. ) ;
#45346 = EDGE_CURVE ( 'NONE', #35548, #27191, #40857, .T. ) ;
#45347 = EDGE_LOOP ( 'NONE', ( #2669, #8657, #4849, #19375 ) ) ;
#45348 = SHAPE_REPRESENTATION_RELATIONSHIP ( 'NONE' , 'NONE' ,  #28315, #13364 ) ;
#45349 = CARTESIAN_POINT ( 'NONE',  ( 808.0189434323515343, -230.0891481129652618, -319.0252816721025511 ) ) ;
#45350 = CARTESIAN_POINT ( 'NONE',  ( 747.2067596250078623, -147.1800572038746395, 352.2312462859687230 ) ) ;
#45351 = EDGE_CURVE ( 'NONE', #7814, #69, #27821, .T. ) ;
#45352 = EDGE_LOOP ( 'NONE', ( #19157, #29433, #23065, #26758 ) ) ;
#45353 = CARTESIAN_POINT ( 'NONE',  ( 813.9316612368132837, -199.4419599262324709, 348.6739635108323228 ) ) ;
#45354 = CARTESIAN_POINT ( 'NONE',  ( 762.1405469898973024, -217.5436935675107293, -357.8594530101016176 ) ) ;
#45355 = CIRCLE ( 'NONE', #25429, 6.119000000000013095 ) ;
#45356 = EDGE_LOOP ( 'NONE', ( #20837, #18645 ) ) ;
#45357 = CARTESIAN_POINT ( 'NONE',  ( 804.6798772138708955, -375.7255117493283478, -334.6312213355107019 ) ) ;
#45358 = CARTESIAN_POINT ( 'NONE',  ( 788.8264449731200330, 2.819942796124898177, -363.6646147819171233 ) ) ;
#45359 = CARTESIAN_POINT ( 'NONE',  ( 769.1273215169530886, -214.7146871989597230, 317.4527132478988847 ) ) ;
#45360 = ADVANCED_FACE ( 'NONE', ( #3580 ), #7034, .F. ) ;
#45361 = FACE_OUTER_BOUND ( 'NONE', #28643, .T. ) ;
#45362 = DIRECTION ( 'NONE',  ( -1.000000000000000000, -0.000000000000000000, -0.000000000000000000 ) ) ;
#45363 = ORIENTED_EDGE ( 'NONE', *, *, #25547, .T. ) ;
#45364 = CARTESIAN_POINT ( 'NONE',  ( 785.3141322388236176, 2.274488250670355871, -364.4286716492789537 ) ) ;
#45365 = CARTESIAN_POINT ( 'NONE',  ( 187.1337867209877857, 56.78581973499402835, 212.6378164459127049 ) ) ;
#45366 = VERTEX_POINT ( 'NONE', #38443 ) ;
#45367 = CARTESIAN_POINT ( 'NONE',  ( 814.8207195650702488, -290.1908817542434349, -336.2433038121456548 ) ) ;
#45368 = CARTESIAN_POINT ( 'NONE',  ( 799.9636004259356241, -142.9181544815166376, 311.2241431872006956 ) ) ;
#45369 = VECTOR ( 'NONE', #44068, 1000.000000000000000 ) ;
#45371 = CARTESIAN_POINT ( 'NONE',  ( 774.6312213355099630, -215.3618753856925423, -364.6798772138717482 ) ) ;
#45370 = CARTESIAN_POINT ( 'NONE',  ( 786.4999999999993179, -292.9981031064102126, 121.3637880562633171 ) ) ;
#45372 = CARTESIAN_POINT ( 'NONE',  ( 805.0264073115434940, -390.3510508353227237, -339.4763451958999099 ) ) ;
#45373 = LINE ( 'NONE', #34961, #27445 ) ;
#45374 = DIRECTION ( 'NONE',  ( 0.000000000000000000, 0.000000000000000000, 1.000000000000000000 ) ) ;
#45375 = CARTESIAN_POINT ( 'NONE',  ( 804.4086373105744769, -73.64542720878957027, -333.3843516231986541 ) ) ;
#45376 = CIRCLE ( 'NONE', #2557, 2.749999999999919176 ) ;
#45377 = AXIS2_PLACEMENT_3D ( 'NONE', #8891, #16273, #44444 ) ;
#45378 = DIRECTION ( 'NONE',  ( -0.000000000000000000, -0.6438296778008192334, 0.7651688349527135946 ) ) ;
#45379 = CARTESIAN_POINT ( 'NONE',  ( 768.8385539511368734, 24.73985825558500551, -306.4236121716840557 ) ) ;
#45380 = CARTESIAN_POINT ( 'NONE',  ( 814.5518280994195948, -303.7255117493286889, -332.4837098697145166 ) ) ;
#45381 = FILL_AREA_STYLE_COLOUR ( '', #1739 ) ;
#45382 = DIRECTION ( 'NONE',  ( 0.000000000000000000, 0.000000000000000000, 1.000000000000000000 ) ) ;
#45383 = CARTESIAN_POINT ( 'NONE',  ( 800.2193346964447755, -90.99823902205663728, -355.1360043628815788 ) ) ;
#45384 = CARTESIAN_POINT ( 'NONE',  ( 768.9521613784389729, -249.8272453906072315, 373.2346286133773106 ) ) ;
#45385 = CARTESIAN_POINT ( 'NONE',  ( 751.2241431872005251, -160.1692326535053326, -359.9636004259367610 ) ) ;
#45386 = CARTESIAN_POINT ( 'NONE',  ( 746.8695393053150156, -173.9073299311472169, 327.6429770376306010 ) ) ;
#45387 = CARTESIAN_POINT ( 'NONE',  ( 795.8262568251477660, 1.627300063937458408, -308.3538107759623585 ) ) ;
#45388 = CARTESIAN_POINT ( 'NONE',  ( 831.1634899080286232, 259.9999999999998863, -199.9999999999999432 ) ) ;
#45389 = VECTOR ( 'NONE', #2830, 1000.000000000000000 ) ;
#45390 = CARTESIAN_POINT ( 'NONE',  ( 771.1735550268778070, -297.1800572038740711, 316.3353852180827630 ) ) ;
#45391 = CARTESIAN_POINT ( 'NONE',  ( 804.6971507214547046, -51.28179084515328867, 344.0799538623459739 ) ) ;
#45392 = CARTESIAN_POINT ( 'NONE',  ( 788.7366044899766848, -419.9073299311465348, -316.5762568750059813 ) ) ;
#45393 = CIRCLE ( 'NONE', #3315, 19.99999999999990763 ) ;
#45394 = CARTESIAN_POINT ( 'NONE',  ( 181.9156952255813735, 290.0000000000001137, -274.9999999999999432 ) ) ;
#45395 = DIRECTION ( 'NONE',  ( 0.000000000000000000, 0.000000000000000000, -1.000000000000000000 ) ) ;
#45397 = CARTESIAN_POINT ( 'NONE',  ( 768.0187753319979720, -320.6346026584195670, 318.0580252608186242 ) ) ;
#45396 = CARTESIAN_POINT ( 'NONE',  ( 803.8651313633788504, -125.2601417444145255, 332.4468031744301015 ) ) ;
#45398 = ORIENTED_EDGE ( 'NONE', *, *, #23048, .F. ) ;
#45399 = CARTESIAN_POINT ( 'NONE',  ( 754.9735926884551418, -258.3510508353231785, -340.5236548041000333 ) ) ;
#45400 = CARTESIAN_POINT ( 'NONE',  ( 800.0135310231082713, -86.08914811296573077, 325.0180583372163028 ) ) ;
#45401 = VECTOR ( 'NONE', #21396, 1000.000000000000000 ) ;
#45402 = CARTESIAN_POINT ( 'NONE',  ( 800.1688906516307043, -274.1692326535049915, -369.0717654672308186 ) ) ;
#45403 = DIRECTION ( 'NONE',  ( -1.000000000000000000, -0.000000000000000000, -0.000000000000000000 ) ) ;
#45404 = CARTESIAN_POINT ( 'NONE',  ( 746.0683387631852383, -403.4419599262317888, 331.3260364891676204 ) ) ;
#45405 = ORIENTED_EDGE ( 'NONE', *, *, #27310, .T. ) ;
#45406 = CARTESIAN_POINT ( 'NONE',  ( 804.9363028652555840, -280.2709662947833067, 338.2165204200192079 ) ) ;
#45407 = VECTOR ( 'NONE', #43774, 1000.000000000000000 ) ;
#45408 = CARTESIAN_POINT ( 'NONE',  ( 794.1144889064781864, -34.16923265350572336, -360.9840315886528401 ) ) ;
#45409 = CARTESIAN_POINT ( 'NONE',  ( 756.3353852180819104, -173.9073299311472169, -331.1735550268788302 ) ) ;
#45410 = CARTESIAN_POINT ( 'NONE',  ( 757.8323909638827445, -218.6346026584197944, -352.1044303154654358 ) ) ;
#45411 = CARTESIAN_POINT ( 'NONE',  ( 795.1360043628807261, -404.0891481129646081, 360.2193346964456282 ) ) ;
#45412 = CIRCLE ( 'NONE', #4815, 20.00000000000001776 ) ;
#45413 = CARTESIAN_POINT ( 'NONE',  ( 812.7932403749906598, -111.1800572038747532, -327.7687537140311633 ) ) ;
#45414 = CARTESIAN_POINT ( 'NONE',  ( 797.6776695296629214, -91.54369356751116982, -357.6776695296636603 ) ) ;
#45415 = ORIENTED_EDGE ( 'NONE', *, *, #35997, .T. ) ;
#45416 = CARTESIAN_POINT ( 'NONE',  ( 769.9779781133707957, -43.09997266333511590, -316.7813123517150871 ) ) ;
#45417 = CARTESIAN_POINT ( 'NONE',  ( 769.9779781133707957, -403.0999726633339719, -316.7813123517150871 ) ) ;
#45419 = CARTESIAN_POINT ( 'NONE',  ( 787.5531968255692163, -429.8272453906067199, 316.1348686366205811 ) ) ;
#45418 = CARTESIAN_POINT ( 'NONE',  ( 800.2193346964447755, -114.9982390220565236, 355.1360043628815788 ) ) ;
#45420 = CARTESIAN_POINT ( 'NONE',  ( 803.2186876482843445, -103.9874144716873161, 350.0220218866286928 ) ) ;
#45423 = CARTESIAN_POINT ( 'NONE',  ( 811.6461892240364477, -340.7146871989592114, 324.1737431748509835 ) ) ;
#45422 = DIRECTION ( 'NONE',  ( 1.000000000000000000, 0.000000000000000000, -0.000000000000000000 ) ) ;
#45421 = LINE ( 'NONE', #30867, #44673 ) ;
#45424 = ORIENTED_EDGE ( 'NONE', *, *, #19317, .F. ) ;
#45425 = CARTESIAN_POINT ( 'NONE',  ( 766.0291762391763086, -346.9181544815160123, -360.7704444035551319 ) ) ;
#45426 = CARTESIAN_POINT ( 'NONE',  ( 788.7366044899766848, -347.9073299311467053, -316.5762568750059813 ) ) ;
#45427 = CARTESIAN_POINT ( 'NONE',  ( 810.4231160770870019, -144.5545181178802636, -321.9338519418446936 ) ) ;
#45428 = CARTESIAN_POINT ( 'NONE',  ( 745.1792804349281596, -38.19088175424422360, 343.7566961878542884 ) ) ;
#45429 = AXIS2_PLACEMENT_3D ( 'NONE', #4062, #28545, #21605 ) ;
#45431 = LINE ( 'NONE', #27403, #35828 ) ;
#45430 = FACE_OUTER_BOUND ( 'NONE', #26683, .T. ) ;
#45432 = CARTESIAN_POINT ( 'NONE',  ( 795.9930595647434757, -291.0783235625957559, -320.7433823573372820 ) ) ;
#45433 = LINE ( 'NONE', #38970, #6280 ) ;
#45434 = CARTESIAN_POINT ( 'NONE',  ( 754.3581564841646241, -137.4636090269711985, -316.1443688327762516 ) ) ;
#45435 = CYLINDRICAL_SURFACE ( 'NONE', #39998, 8.024999999999948841 ) ;
#45436 = CARTESIAN_POINT ( 'NONE',  ( -28.63011601220122415, -365.3551492539851893, -18.13243251470705886 ) ) ;
#45437 = CONICAL_SURFACE ( 'NONE', #11506, 8.025000000000003908, 0.7853981633974428389 ) ;
#45438 = CARTESIAN_POINT ( 'NONE',  ( 769.9779781133707957, -355.0999726633341993, 316.7813123517150871 ) ) ;
#45439 = CARTESIAN_POINT ( 'NONE',  ( 745.7194118038753459, -325.6454272087888739, 348.7631598425976449 ) ) ;
#45440 = CARTESIAN_POINT ( 'NONE',  ( 792.3570229623691148, -189.1800572038744690, -373.1304606946836770 ) ) ;
#45441 = CARTESIAN_POINT ( 'NONE',  ( 939.9999999999993179, -600.0000000000001137, 350.0000000000000000 ) ) ;
#45442 = VECTOR ( 'NONE', #26406, 1000.000000000000000 ) ;
#45443 = CARTESIAN_POINT ( 'NONE',  ( 799.9636004259356241, -94.91815448151677970, 311.2241431872006956 ) ) ;
#45444 = CARTESIAN_POINT ( 'NONE',  ( 777.4774526936600978, -298.2709662947830793, -304.7301800767027657 ) ) ;
#45445 = AXIS2_PLACEMENT_3D ( 'NONE', #44430, #40531, #8880 ) ;
#45446 = DIRECTION ( 'NONE',  ( -0.000000000000000000, -0.000000000000000000, 1.000000000000000000 ) ) ;
#45447 = LINE ( 'NONE', #13118, #5042 ) ;
#45448 = CARTESIAN_POINT ( 'NONE',  ( 805.1927285166397041, -184.8164208402380950, 341.8018195045277707 ) ) ;
#45449 = ORIENTED_EDGE ( 'NONE', *, *, #25580, .T. ) ;
#45450 = CARTESIAN_POINT ( 'NONE',  ( 760.0363995740630116, -418.9181544815157849, 368.7758568127991907 ) ) ;
#45451 = CARTESIAN_POINT ( 'NONE',  ( 793.4146539503750546, -361.9874144716864635, -307.6481478633938877 ) ) ;
#45452 = CARTESIAN_POINT ( 'NONE',  ( 782.4968714119720516, -130.8164208402383224, -305.0891759886411023 ) ) ;
#45453 = CARTESIAN_POINT ( 'NONE',  ( 805.0032342141412300, -397.5436935675100472, -314.9967657858571783 ) ) ;
#45454 = CARTESIAN_POINT ( 'NONE',  ( 786.4999999999993179, -365.3551492539851893, -18.13243251470705886 ) ) ;
#45455 = CARTESIAN_POINT ( 'NONE',  ( 786.2056067578752163, 12.19440371013049784, 374.4686193811670023 ) ) ;
#45456 = VERTEX_POINT ( 'NONE', #17191 ) ;
#45457 = CARTESIAN_POINT ( 'NONE',  ( 786.2056067578752163, -155.8055962898689586, -374.4686193811670023 ) ) ;
#45458 = CARTESIAN_POINT ( 'NONE',  ( 998.9999999999992042, 479.9999999999999432, 199.9999999999999716 ) ) ;
#45459 = CARTESIAN_POINT ( 'NONE',  ( 788.7631598425961101, -313.4419599262320730, 305.7194118038759143 ) ) ;
#45460 = CARTESIAN_POINT ( 'NONE',  ( 800.0135310231082713, -134.0891481129655745, 325.0180583372163028 ) ) ;
#45461 = ORIENTED_EDGE ( 'NONE', *, *, #20695, .F. ) ;
#45462 = VECTOR ( 'NONE', #5394, 1000.000000000000000 ) ;
#45463 = CARTESIAN_POINT ( 'NONE',  ( 804.4286716492782716, -305.3618753856922581, 345.3141322388244703 ) ) ;
#45464 = VECTOR ( 'NONE', #15383, 1000.000000000000114 ) ;
#45465 = CARTESIAN_POINT ( 'NONE',  ( 777.5031285880264704, -22.81642084023865280, -374.9108240113588408 ) ) ;
#45466 = EDGE_CURVE ( 'NONE', #2958, #40161, #23649, .T. ) ;
#45467 = CARTESIAN_POINT ( 'NONE',  ( 779.9999999999992042, -452.9681489794448339, 339.9999999999999432 ) ) ;
#45468 = ORIENTED_EDGE ( 'NONE', *, *, #43860, .F. ) ;
#45469 = CARTESIAN_POINT ( 'NONE',  ( 795.1360043628807261, -188.0891481129653187, -360.2193346964456282 ) ) ;
#45470 = CARTESIAN_POINT ( 'NONE',  ( 762.1177392798416577, -426.5545181178794678, -309.8865473780659272 ) ) ;
#45471 = VECTOR ( 'NONE', #44302, 1000.000000000000000 ) ;
#45472 = ORIENTED_EDGE ( 'NONE', *, *, #45271, .T. ) ;
#45473 = CARTESIAN_POINT ( 'NONE',  ( 788.7366044899766848, -11.90732993114778182, 316.5762568750059813 ) ) ;
#45474 = CARTESIAN_POINT ( 'NONE',  ( 785.3141322388236176, -261.7255117493288026, -364.4286716492789537 ) ) ;
#45475 = VECTOR ( 'NONE', #19957, 1000.000000000000000 ) ;
#45477 = CARTESIAN_POINT ( 'NONE',  ( 811.6461892240364477, -244.7146871989596093, 324.1737431748509835 ) ) ;
#45476 = CARTESIAN_POINT ( 'NONE',  ( 796.9462024416508257, -348.4527844766012095, 308.9653473494370246 ) ) ;
#45478 = CARTESIAN_POINT ( 'NONE',  ( 786.5483106153019435, -247.6454272087890160, -364.1601925771022366 ) ) ;
#45479 = CARTESIAN_POINT ( 'NONE',  ( 797.6776695296629214, -259.5436935675106156, -357.6776695296636603 ) ) ;
#45480 = CARTESIAN_POINT ( 'NONE',  ( 805.1927285166399315, -448.8164208402372424, -341.8018195045277707 ) ) ;
#45481 = CARTESIAN_POINT ( 'NONE',  ( 771.2633955100217236, -95.90732993114751537, -363.4237431249939618 ) ) ;
#45482 = CARTESIAN_POINT ( 'NONE',  ( 767.8955696845333705, -240.4527844766015221, 362.1676090361162323 ) ) ;
#45483 = CARTESIAN_POINT ( 'NONE',  ( 747.2067596250078623, -387.1800572038738437, 352.2312462859687230 ) ) ;
#45484 = DIRECTION ( 'NONE',  ( -1.000000000000000000, -1.644774851296528363E-16, -0.000000000000000000 ) ) ;
#45485 = CARTESIAN_POINT ( 'NONE',  ( 752.7379699480933368, -36.00906357242605793, -361.9858362298580232 ) ) ;
#45486 = LINE ( 'NONE', #17989, #35198 ) ;
#45487 = FACE_OUTER_BOUND ( 'NONE', #14510, .T. ) ;
#45488 = CARTESIAN_POINT ( 'NONE',  ( 755.5913626894240451, -229.6454272087890729, 346.6156483768012890 ) ) ;
#45489 = CARTESIAN_POINT ( 'NONE',  ( 792.1044303154645831, -108.4527844766019911, 317.8323909638837677 ) ) ;
#45490 = ADVANCED_FACE ( 'NONE', ( #6347 ), #16749, .F. ) ;
#45491 = VERTEX_POINT ( 'NONE', #37760 ) ;
#45492 = CARTESIAN_POINT ( 'NONE',  ( 805.2837595273609850, -2.736336299698892027, -340.5290396650784714 ) ) ;
#45493 = CARTESIAN_POINT ( 'NONE',  ( 810.7187646348534145, -66.45278447660216159, -356.7737145352016341 ) ) ;
#45494 = CARTESIAN_POINT ( 'NONE',  ( 802.7791456095903868, -292.7146871989594956, 329.0155153010375102 ) ) ;
#45495 = CARTESIAN_POINT ( 'NONE',  ( 771.1735550268778070, -417.1800572038736163, -316.3353852180827630 ) ) ;
#45496 = CARTESIAN_POINT ( 'NONE',  ( 786.2694204179717872, 2.718209154846545683, 305.1769319972829067 ) ) ;
#45498 = VECTOR ( 'NONE', #23742, 1000.000000000000000 ) ;
#45497 = CARTESIAN_POINT ( 'NONE',  ( 801.1904061080336987, -212.0891481129652902, -368.3070685750235498 ) ) ;
#45499 = CARTESIAN_POINT ( 'NONE',  ( 810.7187646348534145, -186.4527844766017779, 356.7737145352016341 ) ) ;
#45500 = CARTESIAN_POINT ( 'NONE',  ( 801.9419747391806368, -66.45278447660216159, 351.9812246680014027 ) ) ;
#45501 = VECTOR ( 'NONE', #14290, 1000.000000000000000 ) ;
#45502 = DIRECTION ( 'NONE',  ( 0.000000000000000000, -0.9238795325112835188, 0.3826834323650978309 ) ) ;
#45503 = LINE ( 'NONE', #23992, #33538 ) ;
#45504 = CARTESIAN_POINT ( 'NONE',  ( 756.1443688327750579, -285.6237781080502600, -314.3581564841659315 ) ) ;
#45505 = AXIS2_PLACEMENT_3D ( 'NONE', #9514, #41843, #45300 ) ;
#45506 = CARTESIAN_POINT ( 'NONE',  ( 795.8262568251477660, -430.3726999360611671, 308.3538107759623585 ) ) ;
#45507 = CARTESIAN_POINT ( 'NONE',  ( 777.5031285880264704, -286.8164208402378677, -374.9108240113588408 ) ) ;
#45508 = CARTESIAN_POINT ( 'NONE',  ( 779.9999999999992042, -452.9681489794448339, -339.9999999999999432 ) ) ;
#45509 = CARTESIAN_POINT ( 'NONE',  ( 764.0069404352550464, -351.0783235625955854, 359.2566176426627180 ) ) ;
#45510 = CARTESIAN_POINT ( 'NONE',  ( 777.5031285880264704, -46.81642084023858530, 374.9108240113588408 ) ) ;
#45511 = CARTESIAN_POINT ( 'NONE',  ( 765.0180583372156207, -384.9982390220556567, -360.0135310231089534 ) ) ;
#45512 = CIRCLE ( 'NONE', #25591, 9.999999999999982236 ) ;
#45513 = CARTESIAN_POINT ( 'NONE',  ( 756.7813123517142913, -19.98741447168758256, 329.9779781133712504 ) ) ;
#45514 = CARTESIAN_POINT ( 'NONE',  ( 771.1735550268778070, -201.1800572038744690, -316.3353852180827630 ) ) ;
#45515 = CARTESIAN_POINT ( 'NONE',  ( 746.7653713866222915, -41.26014174441479554, -351.0478386215610271 ) ) ;
#45516 = CARTESIAN_POINT ( 'NONE',  ( 798.7617431975189675, -195.6237781080506863, -323.0428371773161871 ) ) ;
#45517 = CARTESIAN_POINT ( 'NONE',  ( 814.8230680027162407, -173.8055962898689302, 333.7305795820267917 ) ) ;
#45518 = VERTEX_POINT ( 'NONE', #20649 ) ;
#45519 = CARTESIAN_POINT ( 'NONE',  ( 763.2154366446407039, -189.6237781080507148, -321.4292242960311228 ) ) ;
#45520 = UNCERTAINTY_MEASURE_WITH_UNIT (LENGTH_MEASURE( 1.000000000000000082E-05 ), #36091, 'distance_accuracy_value', 'NONE');
#45521 = CARTESIAN_POINT ( 'NONE',  ( 797.8594530101008786, -205.5436935675108430, 322.1405469898980982 ) ) ;
#45522 = EDGE_CURVE ( 'NONE', #18651, #36310, #6109, .T. ) ;
#45523 = CARTESIAN_POINT ( 'NONE',  ( 791.1614460488616487, -35.26014174441480264, -373.5763878283158874 ) ) ;
#45524 = CARTESIAN_POINT ( 'NONE',  ( 759.7806653035535192, -342.9982390220557704, 324.8639956371181370 ) ) ;
#45525 = LINE ( 'NONE', #20566, #10204 ) ;
#45526 = ORIENTED_EDGE ( 'NONE', *, *, #25849, .F. ) ;
#45527 = CARTESIAN_POINT ( 'NONE',  ( 780.5290396650775619, -36.35105083532390324, 365.2837595273619513 ) ) ;
#45528 = CARTESIAN_POINT ( 'NONE',  ( 750.9282345327678740, -304.9181544815161828, -319.8311093483690115 ) ) ;
#45529 = VECTOR ( 'NONE', #7369, 1000.000000000000000 ) ;
#45530 = CARTESIAN_POINT ( 'NONE',  ( 758.8095938919644823, -272.0891481129651197, 311.6929314249762797 ) ) ;
#45531 = CARTESIAN_POINT ( 'NONE',  ( 755.3028492785439312, -351.2817908451523294, 335.9200461376539693 ) ) ;
#45532 = CARTESIAN_POINT ( 'NONE',  ( 769.1273215169530886, -430.7146871989590409, 317.4527132478988847 ) ) ;
#45533 = CARTESIAN_POINT ( 'NONE',  ( 798.5707757039680246, -149.4636090269711417, -356.7845633553585003 ) ) ;
#45534 = CARTESIAN_POINT ( 'NONE',  ( 774.6858677611749044, -153.7255117493291721, -315.5713283507209894 ) ) ;
#45535 = CARTESIAN_POINT ( 'NONE',  ( 781.8018195045267476, -334.2709662947830793, -365.1927285166407273 ) ) ;
#45536 = ORIENTED_EDGE ( 'NONE', *, *, #39112, .T. ) ;
#45537 = CARTESIAN_POINT ( 'NONE',  ( 803.4237431249931660, -447.1800572038736732, -331.2633955100225194 ) ) ;
#45538 = CIRCLE ( 'NONE', #10882, 6.118999999999985562 ) ;
#45539 = CARTESIAN_POINT ( 'NONE',  ( 749.2812353651451076, -246.4527844766016074, 323.2262854647983090 ) ) ;
#45540 = CARTESIAN_POINT ( 'NONE',  ( 765.8855110935204493, -334.1692326535047073, 319.0159684113471599 ) ) ;
#45541 = CARTESIAN_POINT ( 'NONE',  ( 959.5497976682736407, 239.9999999999998863, 350.0000000000000000 ) ) ;
#45542 = CARTESIAN_POINT ( 'NONE',  ( 776.9254006560222479, -116.1908817542440033, 314.8983024940802125 ) ) ;
#45543 = CARTESIAN_POINT ( 'NONE',  ( 805.1927285166397041, -16.81642084023866701, 341.8018195045277707 ) ) ;
#45544 = ORIENTED_EDGE ( 'NONE', *, *, #37084, .T. ) ;
#45545 = CARTESIAN_POINT ( 'NONE',  ( 812.3518521366052028, -361.0999726633341425, -326.5853460496235243 ) ) ;
#45546 = PLANE ( 'NONE',  #10718 ) ;
#45547 = CARTESIAN_POINT ( 'NONE',  ( 763.0428371773158460, -227.4636090269709143, 358.7617431975195359 ) ) ;
#45548 = CARTESIAN_POINT ( 'NONE',  ( 814.8207195650702488, -242.1908817542435770, 336.2433038121456548 ) ) ;
#45549 = CARTESIAN_POINT ( 'NONE',  ( 799.4546378042377910, -177.0783235625961538, 356.1575198192848006 ) ) ;
#45550 = CARTESIAN_POINT ( 'NONE',  ( 800.2193346964447755, -330.9982390220558273, -355.1360043628815788 ) ) ;
#45551 = DIRECTION ( 'NONE',  ( 0.000000000000000000, 0.000000000000000000, 1.000000000000000000 ) ) ;
#45552 = CARTESIAN_POINT ( 'NONE',  ( 761.4292242960306112, -209.4636090269709996, -323.2154366446414429 ) ) ;
#45553 = CARTESIAN_POINT ( 'NONE',  ( 772.5602148656447525, -9.725511749329603717, 305.7998596910095443 ) ) ;
#45554 = CARTESIAN_POINT ( 'NONE',  ( 808.2983282543862060, -452.9681489794448908, 337.2950253338145785 ) ) ;
#45555 = CARTESIAN_POINT ( 'NONE',  ( 792.2312462859673587, -419.9073299311465348, -307.2067596250082602 ) ) ;
#45556 = FACE_OUTER_BOUND ( 'NONE', #16712, .T. ) ;
#45557 = CARTESIAN_POINT ( 'NONE',  ( 745.7194118038753459, -349.6454272087887603, 348.7631598425976449 ) ) ;
#45558 = CARTESIAN_POINT ( 'NONE',  ( 791.4804426738954817, -453.0432664090020580, -367.7164109511201673 ) ) ;
#45559 = CARTESIAN_POINT ( 'NONE',  ( 792.2312462859673587, -299.9073299311468759, 307.2067596250082602 ) ) ;
#45560 = CARTESIAN_POINT ( 'NONE',  ( 815.2698199232961542, -40.81642084023859951, -342.5225473063383106 ) ) ;
#45561 = CARTESIAN_POINT ( 'NONE',  ( 756.3353852180819104, -293.9073299311468759, -331.1735550268788302 ) ) ;
#45562 = ADVANCED_FACE ( 'NONE', ( #34524 ), #38224, .F. ) ;
#45563 = DIRECTION ( 'NONE',  ( 1.892425610156518354E-16, 1.000000000000000000, -0.000000000000000000 ) ) ;
#45564 = CARTESIAN_POINT ( 'NONE',  ( 754.8072714833581358, -388.8164208402374129, 338.1981804954720587 ) ) ;
#45565 = EDGE_CURVE ( 'NONE', #4358, #44996, #26109, .T. ) ;
#45566 = CARTESIAN_POINT ( 'NONE',  ( 755.3028492785439312, -159.2817908451529547, 335.9200461376539693 ) ) ;
#45567 = CARTESIAN_POINT ( 'NONE',  ( 783.7953271457878373, -32.19088175424425913, -375.1787889125761239 ) ) ;
#45568 = CARTESIAN_POINT ( 'NONE',  ( 793.2243759319678702, -98.53286901714187707, -318.4439275373583200 ) ) ;
#45569 = CARTESIAN_POINT ( 'NONE',  ( 791.1614460488616487, -83.26014174441466764, 373.5763878283158874 ) ) ;
#45570 = CARTESIAN_POINT ( 'NONE',  ( 771.1735550268780344, -393.1800572038737869, 316.3353852180828198 ) ) ;
#45571 = CIRCLE ( 'NONE', #2800, 2.749999999999919176 ) ;
#45572 = LINE ( 'NONE', #37937, #41718 ) ;
#45573 = CARTESIAN_POINT ( 'NONE',  ( 801.9419747391806368, -426.4527844766010389, 351.9812246680014027 ) ) ;
#45575 = ORIENTED_EDGE ( 'NONE', *, *, #38557, .F. ) ;
#45574 = CARTESIAN_POINT ( 'NONE',  ( 800.7704444035546203, -100.1692326535055315, -326.0291762391768771 ) ) ;
#45576 = CARTESIAN_POINT ( 'NONE',  ( 754.8072714833581358, -52.81642084023856398, -338.1981804954720587 ) ) ;
#45577 = ADVANCED_FACE ( 'NONE', ( #45619 ), #14452, .F. ) ;
#45578 = ADVANCED_FACE ( 'NONE', ( #4288 ), #18379, .T. ) ;
#45579 = CARTESIAN_POINT ( 'NONE',  ( 772.3691319403857278, -359.2601417444137724, -315.8894580844506663 ) ) ;
#45581 = CARTESIAN_POINT ( 'NONE',  ( 791.9812246680005501, -236.6346026584198228, 361.9419747391813189 ) ) ;
#45580 = CARTESIAN_POINT ( 'NONE',  ( 756.5762568750052424, -243.1800572038743269, 348.7366044899774238 ) ) ;
#45582 = CARTESIAN_POINT ( 'NONE',  ( 810.1134526219336749, -392.5328690171409107, -357.8822607201570349 ) ) ;
#45583 = LINE ( 'NONE', #36087, #593 ) ;
#45584 = ORIENTED_EDGE ( 'NONE', *, *, #34065, .T. ) ;
#45585 = CARTESIAN_POINT ( 'NONE',  ( 754.8072714833581358, -388.8164208402374129, 338.1981804954720587 ) ) ;
#45586 = ORIENTED_EDGE ( 'NONE', *, *, #41610, .T. ) ;
#45587 = CARTESIAN_POINT ( 'NONE',  ( 787.4397851343537695, -237.7255117493289163, -374.2001403089903988 ) ) ;
#45588 = CARTESIAN_POINT ( 'NONE',  ( 782.5225473063383106, -142.2709662947837330, 375.2698199232970637 ) ) ;
#45589 = ORIENTED_EDGE ( 'NONE', *, *, #10862, .F. ) ;
#45590 = CARTESIAN_POINT ( 'NONE',  ( 805.9055244015594326, -195.6237781080506863, 315.8990559732753240 ) ) ;
#45591 = CARTESIAN_POINT ( 'NONE',  ( 785.3141322388236176, -213.7255117493289731, -364.4286716492789537 ) ) ;
#45592 = ORIENTED_EDGE ( 'NONE', *, *, #38840, .T. ) ;
#45593 = EDGE_CURVE ( 'NONE', #27172, #18205, #43517, .T. ) ;
#45594 = CARTESIAN_POINT ( 'NONE',  ( 803.4237431249931660, -351.1800572038740142, -331.2633955100225194 ) ) ;
#45595 = CARTESIAN_POINT ( 'NONE',  ( 771.2633955100217236, 0.09267006885218045942, -363.4237431249939618 ) ) ;
#45596 = EDGE_CURVE ( 'NONE', #21264, #44330, #35717, .T. ) ;
#45597 = CARTESIAN_POINT ( 'NONE',  ( 772.3691319403857278, -215.2601417444141987, 315.8894580844506663 ) ) ;
#45598 = DIRECTION ( 'NONE',  ( 0.000000000000000000, 0.000000000000000000, 1.000000000000000000 ) ) ;
#45599 = DIRECTION ( 'NONE',  ( 1.000000000000000000, 0.000000000000000000, -0.000000000000000000 ) ) ;
#45600 = VERTEX_POINT ( 'NONE', #36601 ) ;
#45601 = CARTESIAN_POINT ( 'NONE',  ( 794.9819416627830151, 11.00176097794305541, -319.9864689768909898 ) ) ;
#45602 = DIRECTION ( 'NONE',  ( -0.3826814224632280603, -1.110223024625159854E-14, 0.9238803650373355048 ) ) ;
#45603 = CARTESIAN_POINT ( 'NONE',  ( 927.9999999999992042, 219.9999999999998863, 350.0000000000000000 ) ) ;
#45604 = ORIENTED_EDGE ( 'NONE', *, *, #4995, .F. ) ;
#45605 = CARTESIAN_POINT ( 'NONE',  ( 809.0717654672305343, -268.9181544815162397, -360.1688906516309885 ) ) ;
#45606 = CARTESIAN_POINT ( 'NONE',  ( 771.3260364891663130, -139.6454272087893571, 306.0683387631859773 ) ) ;
#45607 = AXIS2_PLACEMENT_3D ( 'NONE', #31189, #13643, #41829 ) ;
#45609 = CARTESIAN_POINT ( 'NONE',  ( 765.0180583372156207, -216.9982390220562252, -360.0135310231089534 ) ) ;
#45608 = DIRECTION ( 'NONE',  ( 0.000000000000000000, 0.000000000000000000, 1.000000000000000000 ) ) ;
#45610 = CARTESIAN_POINT ( 'NONE',  ( 769.1273215169530886, -406.7146871989590409, -317.4527132478988847 ) ) ;
#45611 = CARTESIAN_POINT ( 'NONE',  ( 775.4999999999993179, -365.3551492539851893, -18.13243251470705886 ) ) ;
#45612 = DIRECTION ( 'NONE',  ( 1.000000000000000000, -0.000000000000000000, -0.000000000000000000 ) ) ;
#45613 = CARTESIAN_POINT ( 'NONE',  ( 755.8894580844503253, -111.8272453906076151, -332.3691319403863531 ) ) ;
#45614 = CARTESIAN_POINT ( 'NONE',  ( 749.5768839229115201, -372.5545181178796383, 358.0661480581553064 ) ) ;
#45615 = CARTESIAN_POINT ( 'NONE',  ( -784.4999999999993179, -501.1515549466498669, -368.0974687824633520 ) ) ;
#45616 = CARTESIAN_POINT ( 'NONE',  ( 793.4146539503750546, 22.01258552831228599, -307.6481478633938877 ) ) ;
#45617 = CARTESIAN_POINT ( 'NONE',  ( 800.9747183278959710, -300.9982390220559409, -311.9810565676471583 ) ) ;
#45618 = DIRECTION ( 'NONE',  ( 0.000000000000000000, 0.000000000000000000, -1.000000000000000000 ) ) ;
#45619 = FACE_OUTER_BOUND ( 'NONE', #22903, .T. ) ;
#45620 = CARTESIAN_POINT ( 'NONE',  ( 805.1927285166397041, -88.81642084023842187, -341.8018195045277707 ) ) ;
#45621 = EDGE_CURVE ( 'NONE', #33196, #20005, #20964, .T. ) ;
#45622 = CARTESIAN_POINT ( 'NONE',  ( 757.7880784355613741, -258.0090635724253616, 312.4576283171834916 ) ) ;
#45623 = CARTESIAN_POINT ( 'NONE',  ( 793.4146539503750546, -217.9874144716870035, -307.6481478633938877 ) ) ;
#45624 = CARTESIAN_POINT ( 'NONE',  ( 787.5162901302840055, -179.3618753856927128, 305.4481719005792684 ) ) ;
#45625 = CARTESIAN_POINT ( 'NONE',  ( 746.8695393053150156, -437.9073299311463074, -327.6429770376306010 ) ) ;
#45626 = LINE ( 'NONE', #20878, #5489 ) ;
#45627 = ADVANCED_FACE ( 'NONE', ( #26633 ), #27109, .F. ) ;
#45628 = CARTESIAN_POINT ( 'NONE',  ( 756.5762568750052424, -291.1800572038741848, 348.7366044899774238 ) ) ;
#45629 = CARTESIAN_POINT ( 'NONE',  ( 755.5913626894240451, -85.64542720878952764, 346.6156483768012890 ) ) ;
#45630 = CARTESIAN_POINT ( 'NONE',  ( 762.3223304703356007, -439.5436935675101040, -322.3223304703362828 ) ) ;
#45631 = LINE ( 'NONE', #6804, #40941 ) ;
#45632 = CARTESIAN_POINT ( 'NONE',  ( 187.1337867209877857, 62.85347435602256638, 357.4246812887967053 ) ) ;
#45634 = CARTESIAN_POINT ( 'NONE',  ( 762.3223304703356007, -319.5436935675104451, 322.3223304703362828 ) ) ;
#45633 = CARTESIAN_POINT ( 'NONE',  ( 764.0069404352550464, -135.0783235625962959, 359.2566176426627180 ) ) ;
#45635 = VERTEX_POINT ( 'NONE', #33574 ) ;
#45636 = EDGE_CURVE ( 'NONE', #20535, #23353, #9175, .T. ) ;
#45637 = CARTESIAN_POINT ( 'NONE',  ( 798.7617431975189675, -267.6237781080504305, -323.0428371773161871 ) ) ;
#45638 = CARTESIAN_POINT ( 'NONE',  ( 791.9812246680005501, -92.63460265842026331, 361.9419747391813189 ) ) ;
#45639 = CARTESIAN_POINT ( 'NONE',  ( 751.2241431872005251, -304.1692326535048210, -359.9636004259367610 ) ) ;
#45640 = DIRECTION ( 'NONE',  ( -0.000000000000000000, -0.000000000000000000, -1.000000000000000000 ) ) ;
#45641 = CARTESIAN_POINT ( 'NONE',  ( 783.7566961878529810, -408.8965053807772847, 305.1792804349288417 ) ) ;
#45642 = VERTEX_POINT ( 'NONE', #44197 ) ;
#45643 = CARTESIAN_POINT ( 'NONE',  ( 767.8955696845333705, -288.4527844766014937, 362.1676090361162323 ) ) ;
#45644 = AXIS2_PLACEMENT_3D ( 'NONE', #11479, #21866, #28574 ) ;
#45645 = CARTESIAN_POINT ( 'NONE',  ( 803.2186876482843445, -55.98741447168748664, -350.0220218866286928 ) ) ;
#45646 = CARTESIAN_POINT ( 'NONE',  ( 804.4286716492782716, -161.3618753856927697, -345.3141322388244703 ) ) ;
#45647 = CARTESIAN_POINT ( 'NONE',  ( 803.6646147819161570, -209.9073299311470748, -348.8264449731210561 ) ) ;
#45648 = CARTESIAN_POINT ( 'NONE',  ( 768.0187753319979720, -392.6346026584193396, 318.0580252608186242 ) ) ;
#45649 = CARTESIAN_POINT ( 'NONE',  ( 814.9108240113580450, -112.2709662947838325, -337.5031285880265273 ) ) ;
#45650 = CARTESIAN_POINT ( 'NONE',  ( 755.3201227861273992, -123.7255117493292289, -345.3687786644892981 ) ) ;
#45651 = ORIENTED_EDGE ( 'NONE', *, *, #42114, .F. ) ;
#45652 = CARTESIAN_POINT ( 'NONE',  ( 796.9571628226829034, -383.4636090269704596, -321.2382568024804641 ) ) ;
#45653 = CARTESIAN_POINT ( 'NONE',  ( 786.5483106153019435, -439.6454272087884760, 364.1601925771022366 ) ) ;
#45654 = CARTESIAN_POINT ( 'NONE',  ( 804.9511171171677688, -125.8055962898690581, 335.8780910478229202 ) ) ;
#45657 = CARTESIAN_POINT ( 'NONE',  ( 749.8865473780648472, -404.5328690171409107, 322.1177392798429082 ) ) ;
#45656 = FACE_OUTER_BOUND ( 'NONE', #34933, .T. ) ;
#45655 = DIRECTION ( 'NONE',  ( 0.000000000000000000, 1.000000000000000000, 0.000000000000000000 ) ) ;
#45658 = ORIENTED_EDGE ( 'NONE', *, *, #19344, .T. ) ;
#45659 = CARTESIAN_POINT ( 'NONE',  ( 769.0155153010367712, -346.3726999360614514, -362.7791456095907279 ) ) ;
#45660 = CARTESIAN_POINT ( 'NONE',  ( 788.8264449731200330, -357.1800572038739006, -363.6646147819171233 ) ) ;
#45661 = CARTESIAN_POINT ( 'NONE',  ( 788.6739635108323228, -151.6454272087892718, -373.9316612368139090 ) ) ;
#45662 = CARTESIAN_POINT ( 'NONE',  ( 795.8262568251477660, -46.37269993606239638, 308.3538107759623585 ) ) ;
#45664 = CARTESIAN_POINT ( 'NONE',  ( 799.9999999999993179, 205.0000000000000568, -319.9999999999999432 ) ) ;
#45663 = CARTESIAN_POINT ( 'NONE',  ( 999.9999999999992042, 478.9999999999999432, -200.9999999999999432 ) ) ;
#45665 = CARTESIAN_POINT ( 'NONE',  ( 787.6308680596127942, -299.2601417444139997, -364.1105419155492768 ) ) ;
#45666 = DIRECTION ( 'NONE',  ( 1.000000000000000000, -1.880165489482579047E-16, 0.000000000000000000 ) ) ;
#45667 = CARTESIAN_POINT ( 'NONE',  ( 750.9282345327678740, -160.9181544815165807, -319.8311093483690115 ) ) ;
#45668 = FACE_BOUND ( 'NONE', #38510, .T. ) ;
#45669 = DIRECTION ( 'NONE',  ( 0.000000000000000000, 0.000000000000000000, 1.000000000000000000 ) ) ;
#45670 = CARTESIAN_POINT ( 'NONE',  ( 805.2837595273609850, -362.7363362996977116, 340.5290396650784714 ) ) ;
#45671 = CARTESIAN_POINT ( 'NONE',  ( 776.2046728542105711, -332.1908817542433781, 304.8212110874238761 ) ) ;
#45672 = CARTESIAN_POINT ( 'NONE',  ( 787.5162901302840055, -203.3618753856926276, -305.4481719005793252 ) ) ;
#45673 = CARTESIAN_POINT ( 'NONE',  ( -879.9999999999992042, 240.0000000000002274, -224.9999999999999716 ) ) ;
#45674 = AXIS2_PLACEMENT_3D ( 'NONE', #8580, #11592, #8343 ) ;
#45675 = EDGE_CURVE ( 'NONE', #5978, #43844, #37030, .T. ) ;
#45676 = CARTESIAN_POINT ( 'NONE',  ( 762.1177392798416577, -138.5545181178802636, 309.8865473780659272 ) ) ;
#45677 = CARTESIAN_POINT ( 'NONE',  ( 773.7943932421234194, -95.80559628986917176, -305.5313806188329409 ) ) ;
#45678 = CARTESIAN_POINT ( 'NONE',  ( 814.9108240113580450, -352.2709662947830225, -337.5031285880265273 ) ) ;
#45679 = LINE ( 'NONE', #42196, #4751 ) ;
#45680 = CARTESIAN_POINT ( 'NONE',  ( 786.4999999999993179, -512.9681489794448908, -339.9999999999999432 ) ) ;
#45681 = CARTESIAN_POINT ( 'NONE',  ( 781.8018195045266339, -190.2709662947835909, 365.1927285166406705 ) ) ;
#45682 = CARTESIAN_POINT ( 'NONE',  ( 759.9999999999992042, -512.9681489794448908, 350.0000000000000000 ) ) ;
#45683 = CARTESIAN_POINT ( 'NONE',  ( 797.8822607201568644, -462.5545181178792973, 370.1134526219340160 ) ) ;
#45684 = CARTESIAN_POINT ( 'NONE',  ( 803.8556311672234642, -393.6237781080500326, -365.6418435158340117 ) ) ;
#45685 = CARTESIAN_POINT ( 'NONE',  ( 759.0252816721024374, -144.9982390220564525, -368.0189434323527280 ) ) ;
#45686 = CARTESIAN_POINT ( 'NONE',  ( 767.7687537140311633, -431.9073299311464211, -372.7932403749916830 ) ) ;
#45687 = DIRECTION ( 'NONE',  ( 0.000000000000000000, -1.000000000000000000, 0.000000000000000000 ) ) ;
#45688 = CARTESIAN_POINT ( 'NONE',  ( 764.3348316497523456, 1.285312801039623753, 308.6759233522265617 ) ) ;
#45689 = VERTEX_POINT ( 'NONE', #30800 ) ;
#45690 = CARTESIAN_POINT ( 'NONE',  ( 771.2633955100217236, -263.9073299311469327, 363.4237431249939618 ) ) ;
#45691 = CARTESIAN_POINT ( 'NONE',  ( 751.2241431872005251, -184.1692326535052757, -359.9636004259367610 ) ) ;
#45692 = DIRECTION ( 'NONE',  ( -1.000000000000000000, 0.000000000000000000, 0.000000000000000000 ) ) ;
#45693 = CARTESIAN_POINT ( 'NONE',  ( 807.5423716828161105, -321.0783235625956991, 362.2119215644372048 ) ) ;
#45694 = CARTESIAN_POINT ( 'NONE',  ( 755.3201227861273992, -123.7255117493292289, 345.3687786644892981 ) ) ;
#45695 = EDGE_LOOP ( 'NONE', ( #36596, #42577 ) ) ;
#45696 = CARTESIAN_POINT ( 'NONE',  ( 800.0135310231082713, -302.0891481129650629, 325.0180583372163028 ) ) ;
#45697 = CARTESIAN_POINT ( 'NONE',  ( 744.7301800767019131, -4.816420840238714085, -337.4774526936615757 ) ) ;
#45698 = CYLINDRICAL_SURFACE ( 'NONE', #9914, 30.00000000000002842 ) ;
#45699 = ORIENTED_EDGE ( 'NONE', *, *, #20069, .T. ) ;
#45700 = CARTESIAN_POINT ( 'NONE',  ( 766.4474001241216001, -403.0999726633339719, -307.3154664389482491 ) ) ;
#45701 = VECTOR ( 'NONE', #25882, 1000.000000000000000 ) ;
#45702 = VERTEX_POINT ( 'NONE', #33344 ) ;
#45703 = ITEM_DEFINED_TRANSFORMATION ( 'NONE', 'NONE', #41529,  #26858 ) ;
#45704 = CARTESIAN_POINT ( 'NONE',  ( 805.1927285166397041, -16.81642084023866701, 341.8018195045277707 ) ) ;
#45705 = CARTESIAN_POINT ( 'NONE',  ( 764.8639956371174549, -248.0891481129651481, -319.7806653035542013 ) ) ;
#45707 = CARTESIAN_POINT ( 'NONE',  ( 778.7502325331095108, -240.3510508353232069, 304.6391490659818828 ) ) ;
#45706 = CARTESIAN_POINT ( 'NONE',  ( 808.0189434323515343, -350.0891481129648923, 319.0252816721025511 ) ) ;
#45708 = CARTESIAN_POINT ( 'NONE',  ( 800.1688906516307043, -58.16923265350564520, 369.0717654672308186 ) ) ;
#45709 = CARTESIAN_POINT ( 'NONE',  ( 758.0580252608178853, -246.4527844766016074, -328.0187753319985404 ) ) ;
#45710 = CARTESIAN_POINT ( 'NONE',  ( 794.9819416627830151, -444.9982390220554862, -319.9864689768909898 ) ) ;
#45711 = CARTESIAN_POINT ( 'NONE',  ( 768.0187753319979720, -104.6346026584202207, -318.0580252608186242 ) ) ;
#45712 = CARTESIAN_POINT ( 'NONE',  ( 803.4237431249931660, -255.1800572038742700, 331.2633955100225194 ) ) ;
#45713 = CARTESIAN_POINT ( 'NONE',  ( 811.0346526505616112, -374.6346026584192828, 323.0537975583477532 ) ) ;
#45714 = LINE ( 'NONE', #42233, #37382 ) ;
#45715 = CARTESIAN_POINT ( 'NONE',  ( 805.6418435158337843, -53.46360902697146855, -363.8556311672236916 ) ) ;
#45716 = CARTESIAN_POINT ( 'NONE',  ( 779.9999999999992042, 126.4563064324884465, -350.0000000000000000 ) ) ;
#45717 = LINE ( 'NONE', #28142, #32666 ) ;
#45718 = CARTESIAN_POINT ( 'NONE',  ( 800.9840315886518738, -244.9181544815162681, 354.1144889064786412 ) ) ;
#45719 = CARTESIAN_POINT ( 'NONE',  ( 774.6312213355099630, -119.3618753856928691, 364.6798772138717482 ) ) ;
#45720 = VERTEX_POINT ( 'NONE', #12557 ) ;
#45721 = CARTESIAN_POINT ( 'NONE',  ( 763.0428371773158460, -11.46360902697159290, -358.7617431975195359 ) ) ;
#45722 = CARTESIAN_POINT ( 'NONE',  ( 796.7737145352015204, -92.63460265842026331, -370.7187646348536987 ) ) ;
#45723 = CARTESIAN_POINT ( 'NONE',  ( 755.0488828828309806, -305.8055962898684470, 344.1219089521771934 ) ) ;
#45724 = LINE ( 'NONE', #42475, #12320 ) ;
#45725 = CARTESIAN_POINT ( 'NONE',  ( 780.5290396650775619, -36.35105083532390324, 365.2837595273619513 ) ) ;
#45726 = NEXT_ASSEMBLY_USAGE_OCCURRENCE ( 'NAUO1', ' ', ' ', #9831, #42550, $ ) ;
#45727 = NEXT_ASSEMBLY_USAGE_OCCURRENCE ( 'NAUO2', ' ', ' ', #9831, #39755, $ ) ;
#45728 = NEXT_ASSEMBLY_USAGE_OCCURRENCE ( 'NAUO3', ' ', ' ', #9831, #13196, $ ) ;
#45729 = NEXT_ASSEMBLY_USAGE_OCCURRENCE ( 'NAUO4', ' ', ' ', #9831, #33777, $ ) ;
#45730 = NEXT_ASSEMBLY_USAGE_OCCURRENCE ( 'NAUO5', ' ', ' ', #9831, #36333, $ ) ;
#45731 = NEXT_ASSEMBLY_USAGE_OCCURRENCE ( 'NAUO6', ' ', ' ', #9831, #28146, $ ) ;
#45732 = NEXT_ASSEMBLY_USAGE_OCCURRENCE ( 'NAUO7', ' ', ' ', #9831, #21378, $ ) ;
#45733 = NEXT_ASSEMBLY_USAGE_OCCURRENCE ( 'NAUO8', ' ', ' ', #9831, #23335, $ ) ;
#45734 = NEXT_ASSEMBLY_USAGE_OCCURRENCE ( 'NAUO9', ' ', ' ', #9831, #44518, $ ) ;
#45735 = NEXT_ASSEMBLY_USAGE_OCCURRENCE ( 'NAUO10', ' ', ' ', #9831, #3610, $ ) ;
#45736 = NEXT_ASSEMBLY_USAGE_OCCURRENCE ( 'NAUO11', ' ', ' ', #9831, #24214, $ ) ;
#45737 = NEXT_ASSEMBLY_USAGE_OCCURRENCE ( 'NAUO12', ' ', ' ', #9831, #22809, $ ) ;
#45738=COLOUR_RGB('Dark Blue',0.08,0.2,0.34);
#45739=FILL_AREA_STYLE_COLOUR('',#45738);
#45740=FILL_AREA_STYLE('',(#45739));
#45741=SURFACE_STYLE_FILL_AREA(#45740);
#45742=SURFACE_SIDE_STYLE('',(#45741));
#45743=SURFACE_STYLE_USAGE(.BOTH.,#45742);
#45744=PRESENTATION_STYLE_ASSIGNMENT((#45743));
#45745=COLOUR_RGB('Light Blue',0.38,0.62,0.78);
#45746=FILL_AREA_STYLE_COLOUR('',#45745);
#45747=FILL_AREA_STYLE('',(#45746));
#45748=SURFACE_STYLE_FILL_AREA(#45747);
#45749=SURFACE_SIDE_STYLE('',(#45748));
#45750=SURFACE_STYLE_USAGE(.BOTH.,#45749);
#45751=PRESENTATION_STYLE_ASSIGNMENT((#45750));
#45752=COLOUR_RGB('Sky Blue',0.24,0.69,0.87);
#45753=FILL_AREA_STYLE_COLOUR('',#45752);
#45754=FILL_AREA_STYLE('',(#45753));
#45755=SURFACE_STYLE_FILL_AREA(#45754);
#45756=SURFACE_SIDE_STYLE('',(#45755));
#45757=SURFACE_STYLE_USAGE(.BOTH.,#45756);
#45758=PRESENTATION_STYLE_ASSIGNMENT((#45757));
#45759=COLOUR_RGB('Grey',0.48,0.52,0.57);
#45760=FILL_AREA_STYLE_COLOUR('',#45759);
#45761=FILL_AREA_STYLE('',(#45760));
#45762=SURFACE_STYLE_FILL_AREA(#45761);
#45763=SURFACE_SIDE_STYLE('',(#45762));
#45764=SURFACE_STYLE_USAGE(.BOTH.,#45763);
#45765=PRESENTATION_STYLE_ASSIGNMENT((#45764));
#45766=COLOUR_RGB('Black',0.12,0.14,0.17);
#45767=FILL_AREA_STYLE_COLOUR('',#45766);
#45768=FILL_AREA_STYLE('',(#45767));
#45769=SURFACE_STYLE_FILL_AREA(#45768);
#45770=SURFACE_SIDE_STYLE('',(#45769));
#45771=SURFACE_STYLE_USAGE(.BOTH.,#45770);
#45772=PRESENTATION_STYLE_ASSIGNMENT((#45771));
#45773=COLOUR_RGB('Off White',0.89,0.88,0.83);
#45774=FILL_AREA_STYLE_COLOUR('',#45773);
#45775=FILL_AREA_STYLE('',(#45774));
#45776=SURFACE_STYLE_FILL_AREA(#45775);
#45777=SURFACE_SIDE_STYLE('',(#45776));
#45778=SURFACE_STYLE_USAGE(.BOTH.,#45777);
#45779=PRESENTATION_STYLE_ASSIGNMENT((#45778));
ENDSEC;
END-ISO-10303-21;
